#38155 = CARTESIAN_POINT ( 'NONE',  ( 13.53749999999999964, -2.886751345948125991, -5.000000000000000000 ) ) ;
#38156 = CARTESIAN_POINT ( 'NONE',  ( 17.62500000000000000, 6.123233995736764310E-16, -4.999999999999998224 ) ) ;
#38157 = CARTESIAN_POINT ( 'NONE',  ( 13.72500000122903074, 2.886751345948129099, -4.999999999999998224 ) ) ;
#38158 = CARTESIAN_POINT ( 'NONE',  ( 12.36562500061451608, -6.054752690667223547, -1.112240025338166033E-15 ) ) ;
#38159 = VERTEX_POINT ( 'NONE', #56050 ) ;
#38160 = CARTESIAN_POINT ( 'NONE',  ( -1.071796769724485010, 17.05490381179669868, -25.99999999999999289 ) ) ;
#38161 = CARTESIAN_POINT ( 'NONE',  ( 2.121784821874999061, 17.00937500061451857, -33.67503911421598417 ) ) ;
#38162 = CARTESIAN_POINT ( 'NONE',  ( 4.453125000614517326, 4.541064518000418104, -2.621784821874998173 ) ) ;
#38163 = CARTESIAN_POINT ( 'NONE',  ( -7.967954043666661671E-16, 15.67812499938548143, 34.33755215474603517 ) ) ;
#38164 = CARTESIAN_POINT ( 'NONE',  ( 10.20000000000000107, 0.000000000000000000, 4.999999999999998224 ) ) ;
#38165 = DIRECTION ( 'NONE',  ( 0.000000000000000000, 0.000000000000000000, -1.000000000000000000 ) ) ;
#38166 = ORIENTED_EDGE ( 'NONE', *, *, #3334, .F. ) ;
#38167 = CARTESIAN_POINT ( 'NONE',  ( 23.69062500061451004, -3.027376345333610441, -5.243569643749999898 ) ) ;
#38168 = CARTESIAN_POINT ( 'NONE',  ( 29.51249999999999929, 2.886751345948106007, 5.000000000000033751 ) ) ;
#38169 = CARTESIAN_POINT ( 'NONE',  ( -3.756430356250000102, 18.71562499938548285, 30.00000000000000000 ) ) ;
#38170 = CARTESIAN_POINT ( 'NONE',  ( 20.29687500061451644, 6.054752690667223547, 3.707466751127219781E-16 ) ) ;
#38171 = CARTESIAN_POINT ( 'NONE',  ( 20.09062500061451573, -3.027376345333610441, -5.243569643749999898 ) ) ;
#38172 = CARTESIAN_POINT ( 'NONE',  ( -4.243569643749998122, 13.09062500061459389, -27.54997392385601174 ) ) ;
#38173 = CARTESIAN_POINT ( 'NONE',  ( 7.303125000614516082, 0.000000000000000000, 5.243569643749999010 ) ) ;
#38174 = CARTESIAN_POINT ( 'NONE',  ( 4.528125000614516615, 4.541064518000418104, 2.621784821874999949 ) ) ;
#38175 = CARTESIAN_POINT ( 'NONE',  ( 25.35937500061451644, 0.000000000000000000, 4.756430356249998326 ) ) ;
#38176 = CARTESIAN_POINT ( 'NONE',  ( 21.62812500061451360, 4.541064518000418104, 2.621784821874999949 ) ) ;
#38177 = CYLINDRICAL_SURFACE ( 'NONE', #15023, 3.999999999999996447 ) ;
#38178 = CARTESIAN_POINT ( 'NONE',  ( 3.756430356250000102, 18.94062499938548427, 30.00000000000000000 ) ) ;
#38179 = CARTESIAN_POINT ( 'NONE',  ( 14.33437500061451786, 6.421520780324663323E-16, -5.243569643749999010 ) ) ;
#38180 = CARTESIAN_POINT ( 'NONE',  ( 14.48437500061451821, 4.541064518000418104, 2.621784821874999949 ) ) ;
#38181 = CARTESIAN_POINT ( 'NONE',  ( 22.32187500061451502, -6.054752690667223547, -1.112240025338166033E-15 ) ) ;
#38182 = VERTEX_POINT ( 'NONE', #73038 ) ;
#38183 = CARTESIAN_POINT ( 'NONE',  ( -4.243569643749998122, 11.34687500061451892, 32.45002607614398471 ) ) ;
#38184 = CARTESIAN_POINT ( 'NONE',  ( 3.778125000614519280, -4.541064518000419881, 2.621784821874995952 ) ) ;
#38185 = CARTESIAN_POINT ( 'NONE',  ( 26.35312500061451857, -4.541064518000417216, -2.621784821875001281 ) ) ;
#38186 = CARTESIAN_POINT ( 'NONE',  ( 26.16562500061451502, 3.027376345333611329, 5.243569643749999010 ) ) ;
#38187 = CARTESIAN_POINT ( 'NONE',  ( 1.071796769724495002, 15.10759618943233562, 34.00000000000000000 ) ) ;
#38188 = LINE ( 'NONE', #10125, #19331 ) ;
#38189 = CARTESIAN_POINT ( 'NONE',  ( 4.809375000614516615, -4.541064518000417216, -2.621784821875001281 ) ) ;
#38190 = CARTESIAN_POINT ( 'NONE',  ( 15.26250000122903216, 0.000000000000000000, 4.999999999999998224 ) ) ;
#38191 = CARTESIAN_POINT ( 'NONE',  ( 9.112500001229033586, -4.330127018922190985, -2.500000000000001332 ) ) ;
#38192 = CARTESIAN_POINT ( 'NONE',  ( 29.13750000122903216, 4.330127018922191873, 2.499999999999999556 ) ) ;
#38193 = CARTESIAN_POINT ( 'NONE',  ( 2.000000000000000444, 16.11874999877096570, 26.53589838486224650 ) ) ;
#38194 = CARTESIAN_POINT ( 'NONE',  ( 19.10625000122903216, 4.330127018922192761, -2.499999999999997780 ) ) ;
#38195 = CARTESIAN_POINT ( 'NONE',  ( 12.34687500061452070, -3.027376345333614438, 5.243569643749998122 ) ) ;
#38196 = CARTESIAN_POINT ( 'NONE',  ( 11.88749999999999929, 5.773502691896255534, 3.535250795749688401E-16 ) ) ;
#38197 = VERTEX_POINT ( 'NONE', #5442 ) ;
#38198 = CARTESIAN_POINT ( 'NONE',  ( 19.26562500061451644, 3.027376345333613106, -5.243569643749998122 ) ) ;
#38199 = CARTESIAN_POINT ( 'NONE',  ( 16.84687500061451715, -3.027376345333614438, 5.243569643749998122 ) ) ;
#38200 = CARTESIAN_POINT ( 'NONE',  ( 6.103125000614515905, -4.541064518000417216, -2.621784821875001281 ) ) ;
#38201 = CARTESIAN_POINT ( 'NONE',  ( 21.23437500061451644, 4.541064518000418104, 2.621784821874999949 ) ) ;
#38202 = CARTESIAN_POINT ( 'NONE',  ( 5.803125000614517859, 4.541064518000418104, -2.621784821874998173 ) ) ;
#38203 = CARTESIAN_POINT ( 'NONE',  ( 20.81249999999999645, 2.886751345948157077, -4.999999999999949374 ) ) ;
#38204 = CARTESIAN_POINT ( 'NONE',  ( 7.725000001229034297, -5.773502691896255534, -1.060575238724906372E-15 ) ) ;
#38205 = CARTESIAN_POINT ( 'NONE',  ( 23.65312500061451573, -4.541064518000417216, -2.621784821875001281 ) ) ;
#38206 = CARTESIAN_POINT ( 'NONE',  ( -3.999999999999999112, 18.76250000122903216, -30.00000000000000000 ) ) ;
#38207 = CARTESIAN_POINT ( 'NONE',  ( 6.787500001229032520, -4.330127018922194537, 2.499999999999995559 ) ) ;
#38208 = CARTESIAN_POINT ( 'NONE',  ( 19.22812500061451502, 6.421520780324663323E-16, -5.243569643749999010 ) ) ;
#38209 = CARTESIAN_POINT ( 'NONE',  ( 14.57812500061451644, -4.541064518000419881, 2.621784821874995952 ) ) ;
#38210 = CARTESIAN_POINT ( 'NONE',  ( 24.94687500061451502, -2.746126346562646425, 4.756430356249996549 ) ) ;
#38211 = CARTESIAN_POINT ( 'NONE',  ( 15.48749999999999893, 5.773502691896255534, 3.535250795749688894E-16 ) ) ;
#38212 = CARTESIAN_POINT ( 'NONE',  ( 11.13750000122903216, 4.330127018922191873, 2.499999999999999556 ) ) ;
#38213 = CARTESIAN_POINT ( 'NONE',  ( 8.540625000614518569, 6.054752690667223547, 3.707466751127219781E-16 ) ) ;
#38214 = CARTESIAN_POINT ( 'NONE',  ( 11.31562500061451892, 3.027376345333611329, 5.243569643749999010 ) ) ;
#38215 = EDGE_CURVE ( 'NONE', #18194, #18095, #29226, .T. ) ;
#38216 = CARTESIAN_POINT ( 'NONE',  ( 21.03750000122903074, 4.330127018922191873, 2.499999999999999556 ) ) ;
#38217 = CARTESIAN_POINT ( 'NONE',  ( 4.243569643749999898, 14.64687500061451964, -27.54997392385601529 ) ) ;
#38218 = CARTESIAN_POINT ( 'NONE',  ( 20.14687500061451786, -3.027376345333610441, -5.243569643749999898 ) ) ;
#38219 = CARTESIAN_POINT ( 'NONE',  ( 21.26249999999999574, 2.886751345948129099, -4.999999999999997335 ) ) ;
#38220 = CARTESIAN_POINT ( 'NONE',  ( 4.987500001229032698, -4.330127018922194537, 2.499999999999995559 ) ) ;
#38221 = CARTESIAN_POINT ( 'NONE',  ( 5.259375000614518569, -4.541064518000417216, -2.621784821875001281 ) ) ;
#38222 = CARTESIAN_POINT ( 'NONE',  ( 21.79687500061451644, -3.027376345333614438, 5.243569643749998122 ) ) ;
#38223 = CARTESIAN_POINT ( 'NONE',  ( 5.212500000000002132, 2.886751345948126879, 4.999999999999998224 ) ) ;
#38224 = CARTESIAN_POINT ( 'NONE',  ( 18.85312500061451502, 4.541064518000418104, -2.621784821874998173 ) ) ;
#38225 = CARTESIAN_POINT ( 'NONE',  ( 12.01875000122903181, 2.886751345948126879, 4.999999999999999112 ) ) ;
#38226 = CARTESIAN_POINT ( 'NONE',  ( 13.35000000000000142, 0.000000000000000000, 4.999999999999998224 ) ) ;
#38227 = CARTESIAN_POINT ( 'NONE',  ( 4.544497808834801589, -2.085075457992688897, -4.544497808831748920 ) ) ;
#38228 = CARTESIAN_POINT ( 'NONE',  ( 27.60937500061451644, 0.000000000000000000, 5.243569643749999010 ) ) ;
#38229 = CARTESIAN_POINT ( 'NONE',  ( 20.74687500061451217, 0.000000000000000000, 4.756430356249998326 ) ) ;
#38230 = VECTOR ( 'NONE', #33492, 1000.000000000000000 ) ;
#38231 = CARTESIAN_POINT ( 'NONE',  ( 13.86562500061451431, 3.027376345333613106, -5.243569643749998122 ) ) ;
#38232 = CARTESIAN_POINT ( 'NONE',  ( 13.69687500061451679, -3.027376345333614438, 5.243569643749998122 ) ) ;
#38233 = ORIENTED_EDGE ( 'NONE', *, *, #33218, .F. ) ;
#38234 = CARTESIAN_POINT ( 'NONE',  ( 10.70625000122903536, 0.000000000000000000, 4.999999999999998224 ) ) ;
#38235 = CARTESIAN_POINT ( 'NONE',  ( 22.94062500061451715, 6.054752690667223547, 3.707466751127219781E-16 ) ) ;
#38236 = FACE_OUTER_BOUND ( 'NONE', #9222, .T. ) ;
#38237 = CARTESIAN_POINT ( 'NONE',  ( 1.626862140677534273E-15, 11.67500000122903181, -26.00000000000000355 ) ) ;
#38238 = CARTESIAN_POINT ( 'NONE',  ( 12.52500000000000213, -4.330127018922194537, 2.499999999999995559 ) ) ;
#38239 = CARTESIAN_POINT ( 'NONE',  ( 23.10000000122903074, -2.886751345948125991, -5.000000000000000000 ) ) ;
#38240 = CARTESIAN_POINT ( 'NONE',  ( 18.02812500061451573, 4.541064518000418104, 2.621784821874999949 ) ) ;
#38241 = ORIENTED_EDGE ( 'NONE', *, *, #24606, .T. ) ;
#38242 = CARTESIAN_POINT ( 'NONE',  ( 21.26249999999999574, 2.886751345948129099, -4.999999999999998224 ) ) ;
#38243 = CARTESIAN_POINT ( 'NONE',  ( 23.89687500061451786, 6.054752690667223547, 3.707466751127219781E-16 ) ) ;
#38244 = ORIENTED_EDGE ( 'NONE', *, *, #69367, .F. ) ;
#38245 = CARTESIAN_POINT ( 'NONE',  ( 19.98749999999999716, 5.773502691896255534, 3.535250795749688401E-16 ) ) ;
#38246 = CARTESIAN_POINT ( 'NONE',  ( 9.815625000614518925, 3.027376345333613106, -5.243569643749998122 ) ) ;
#38247 = CARTESIAN_POINT ( 'NONE',  ( 12.30000000000000249, 4.330127018922192761, -2.499999999999997780 ) ) ;
#38248 = CARTESIAN_POINT ( 'NONE',  ( 13.13437500061451679, -2.746126346562646425, 4.756430356249996549 ) ) ;
#38249 = CARTESIAN_POINT ( 'NONE',  ( 16.12500000000000000, -4.330127018922194537, 2.499999999999995559 ) ) ;
#38250 = CARTESIAN_POINT ( 'NONE',  ( 24.78750000000000497, -2.886751345948125991, -5.000000000000000000 ) ) ;
#38251 = CARTESIAN_POINT ( 'NONE',  ( 4.243569643749999898, 19.09062500061451573, 32.45002607614398471 ) ) ;
#38252 = CARTESIAN_POINT ( 'NONE',  ( 3.984375000614517326, 6.421520780324663323E-16, -5.243569643749999010 ) ) ;
#38253 = CARTESIAN_POINT ( 'NONE',  ( 16.32187500061451502, 3.027376345333611329, 5.243569643749999010 ) ) ;
#38254 = CARTESIAN_POINT ( 'NONE',  ( 29.78437500061451715, 4.541064518000418104, 2.621784821874999949 ) ) ;
#38255 = ORIENTED_EDGE ( 'NONE', *, *, #13474, .T. ) ;
#38256 = CARTESIAN_POINT ( 'NONE',  ( 25.30312500061451431, 0.000000000000000000, 5.243569643749999010 ) ) ;
#38257 = CARTESIAN_POINT ( 'NONE',  ( 27.15937500061451360, 0.000000000000000000, 5.243569643749999010 ) ) ;
#38259 = EDGE_CURVE ( 'NONE', #59156, #57451, #1357, .T. ) ;
#38258 = CARTESIAN_POINT ( 'NONE',  ( 17.00625000122903074, 0.000000000000000000, 4.999999999999998224 ) ) ;
#38260 = CARTESIAN_POINT ( 'NONE',  ( 14.92500000000000071, 6.123233995736764310E-16, -4.999999999999998224 ) ) ;
#38261 = CARTESIAN_POINT ( 'NONE',  ( 12.47812500061451502, 6.421520780324663323E-16, -5.243569643749999010 ) ) ;
#38262 = CARTESIAN_POINT ( 'NONE',  ( 3.722276561693393937, 3.338418630728691827, 4.014037966420130665 ) ) ;
#38263 = CARTESIAN_POINT ( 'NONE',  ( 3.242103837493086330E-14, 11.33750000000000213, 26.00000000000000711 ) ) ;
#38264 = CARTESIAN_POINT ( 'NONE',  ( 28.00312500061451715, 0.000000000000000000, 5.243569643749999010 ) ) ;
#38265 = CARTESIAN_POINT ( 'NONE',  ( 15.75000000122902932, -2.886751345948129988, 4.999999999999997335 ) ) ;
#38266 = LINE ( 'NONE', #26094, #47788 ) ;
#38267 = CARTESIAN_POINT ( 'NONE',  ( 14.37187500061451928, 2.746126346562645981, -4.756430356249997438 ) ) ;
#38268 = CARTESIAN_POINT ( 'NONE',  ( 4.378125000614518925, 6.421520780324663323E-16, -5.243569643749999010 ) ) ;
#38269 = CARTESIAN_POINT ( 'NONE',  ( 21.60937500061451644, 4.541064518000418104, -2.621784821874998173 ) ) ;
#38270 = CARTESIAN_POINT ( 'NONE',  ( 2.121784821874999061, 16.55937500061451573, 26.32496088578401583 ) ) ;
#38271 = CARTESIAN_POINT ( 'NONE',  ( 22.73437500061451644, -4.541064518000419881, 2.621784821874995952 ) ) ;
#38272 = CARTESIAN_POINT ( 'NONE',  ( 29.63437500061451502, 6.421520780324663323E-16, -5.243569643749999010 ) ) ;
#38273 = CARTESIAN_POINT ( 'NONE',  ( -4.243569643749998122, 18.09687500061451715, 32.45002607614398471 ) ) ;
#38274 = CARTESIAN_POINT ( 'NONE',  ( 11.27812500061451573, 4.541064518000418104, 2.621784821874999949 ) ) ;
#38275 = CARTESIAN_POINT ( 'NONE',  ( 3.150000001229034119, -2.886751345948129988, 4.999999999999997335 ) ) ;
#38276 = CARTESIAN_POINT ( 'NONE',  ( 6.946875000614517681, -3.027376345333614438, 5.243569643749998122 ) ) ;
#38277 = CARTESIAN_POINT ( 'NONE',  ( 12.93750000000000178, -2.886751345948130876, 4.999999999999996447 ) ) ;
#38278 = CARTESIAN_POINT ( 'NONE',  ( 8.840625000614515727, -3.027376345333610441, -5.243569643749999898 ) ) ;
#38279 = CARTESIAN_POINT ( 'NONE',  ( 13.28437500061451715, -4.541064518000419881, 2.621784821874995952 ) ) ;
#38280 = CARTESIAN_POINT ( 'NONE',  ( 28.70625000122903003, 0.000000000000000000, 4.999999999999998224 ) ) ;
#38281 = CARTESIAN_POINT ( 'NONE',  ( 21.82500000122903572, 2.886751345948129099, -4.999999999999998224 ) ) ;
#38282 = CARTESIAN_POINT ( 'NONE',  ( 7.171875000614517326, 3.027376345333613106, -5.243569643749998122 ) ) ;
#38283 = CARTESIAN_POINT ( 'NONE',  ( 10.49062500061451431, -3.027376345333614438, 5.243569643749998122 ) ) ;
#38284 = CARTESIAN_POINT ( 'NONE',  ( 26.98125000122903216, -4.330127018922194537, 2.499999999999995559 ) ) ;
#38285 = CARTESIAN_POINT ( 'NONE',  ( 21.64687500061451786, 6.054752690667223547, 3.707466751127219781E-16 ) ) ;
#38286 = FACE_OUTER_BOUND ( 'NONE', #62334, .T. ) ;
#38287 =( BOUNDED_CURVE ( )  B_SPLINE_CURVE ( 2, ( #41313, #35032, #63471, #6963, #1797, #24307, #46854 ),
 .UNSPECIFIED., .F., .F. ) 
 B_SPLINE_CURVE_WITH_KNOTS ( ( 3, 2, 2, 3 ),
 ( 0.07000000000000000666, 0.07333333333333333370, 0.07666666666666664687, 0.07999999999999998779 ),
 .UNSPECIFIED. ) 
 CURVE ( )  GEOMETRIC_REPRESENTATION_ITEM ( )  RATIONAL_B_SPLINE_CURVE ( ( 1.000000000000000000, 0.8660254037844387076, 1.000000000000000000, 0.8660254037844387076, 1.000000000000000000, 0.8660254037844392627, 0.9999999999999994449 ) ) 
 REPRESENTATION_ITEM ( '' )  );
#38288 = CARTESIAN_POINT ( 'NONE',  ( -0.6906555412606038002, 4.953935347589259131, 33.94230526677440452 ) ) ;
#38289 = CARTESIAN_POINT ( 'NONE',  ( 29.22187500061451715, 3.027376345333612662, -5.243569643749998122 ) ) ;
#38290 = CARTESIAN_POINT ( 'NONE',  ( -3.000416591977282496E-16, 11.19687500061451679, -34.90005215228797653 ) ) ;
#38291 = CARTESIAN_POINT ( 'NONE',  ( 16.08750000122903501, 4.330127018922191873, 2.499999999999999556 ) ) ;
#38292 = CARTESIAN_POINT ( 'NONE',  ( -4.243569643749997233, 14.44062500061451715, -27.54997392385601174 ) ) ;
#38293 = CARTESIAN_POINT ( 'NONE',  ( 18.67500000122903714, 2.886751345948129099, -4.999999999999998224 ) ) ;
#38294 = CARTESIAN_POINT ( 'NONE',  ( 10.97812500061451679, -4.541064518000419881, 2.621784821874995952 ) ) ;
#38295 = VECTOR ( 'NONE', #7873, 1000.000000000000000 ) ;
#38296 = VERTEX_POINT ( 'NONE', #34224 ) ;
#38297 = CARTESIAN_POINT ( 'NONE',  ( 13.23750000000000071, 5.773502691896255534, 3.535250795749688894E-16 ) ) ;
#38298 = CARTESIAN_POINT ( 'NONE',  ( -1.999999999999997113, 13.77500000000000036, 33.46410161513775705 ) ) ;
#38299 = CARTESIAN_POINT ( 'NONE',  ( 23.87812500061451715, 4.541064518000418104, 2.621784821874999949 ) ) ;
#38300 = CARTESIAN_POINT ( 'NONE',  ( 10.09687500061451715, -3.027376345333614438, 5.243569643749998122 ) ) ;
#38301 = CARTESIAN_POINT ( 'NONE',  ( -2.498395430326213790E-14, 17.05624999877096926, 26.00000000000000000 ) ) ;
#38302 = CARTESIAN_POINT ( 'NONE',  ( 10.57500000122903572, 2.886751345948129099, -4.999999999999998224 ) ) ;
#38303 = CARTESIAN_POINT ( 'NONE',  ( 18.41250000122903430, 0.000000000000000000, 4.999999999999998224 ) ) ;
#38304 = CLOSED_SHELL ( 'NONE', ( #2216, #48570, #64448, #6708, #20115, #50433, #8046, #28701, #58821, #58549, #46169, #50768, #15966, #72319, #71451, #52232, #11530, #5648, #63632, #36115, #68116, #44592, #8217, #938, #40897, #9715, #18812, #38595, #7613, #67122, #65303, #48014, #1343, #21552, #1345, #31744, #26322, #29765, #18778, #12039, #31479, #67767, #63978, #42410, #69023, #63739, #5062, #45529, #63989, #63916, #58073, #13339, #30169, #9477, #58970, #24046, #56340, #26141, #28884, #36517, #68685, #34396, #20596, #10857, #53442, #10366, #8427, #70238, #47871, #18911, #56194, #63573, #11058, #6771, #36396, #3882, #34249, #39935, #43142, #21784, #32588, #43797, #59626, #4259, #38917, #70188, #46405, #64940, #49491, #59332, #53414, #31611, #8789, #54092, #11967, #35596, #8710, #58147, #27806, #12217, #43240, #46440, #59400, #26635, #22141, #30413, #30589, #13175, #14823, #15303, #61928, #13081, #52220, #72490, #41168 ) ) ;
#38305 = CARTESIAN_POINT ( 'NONE',  ( 15.59062500061451573, -3.027376345333610441, -5.243569643749999898 ) ) ;
#38306 = CARTESIAN_POINT ( 'NONE',  ( 17.87812500061451715, 6.421520780324663323E-16, -5.243569643749999010 ) ) ;
#38307 = CARTESIAN_POINT ( 'NONE',  ( 26.58750000122903145, -4.330127018922194537, 2.499999999999995559 ) ) ;
#38308 =( BOUNDED_CURVE ( )  B_SPLINE_CURVE ( 2, ( #71155, #20165, #9832, #10563, #43458, #37903, #37169, #48999, #27195, #54899, #32733, #26832, #71530, #20905, #25728, #70790, #60059, #4665, #54172, #15000, #71896, #48266, #43823, #65981, #42719, #15361, #59695, #44192, #26092, #3200, #10198, #66347, #32362, #3569, #37537, #65240, #14629, #61168, #15725, #60421, #9102, #21269, #9470, #4307, #31640, #32000, #55270, #49366, #38264, #48630, #33091, #54535, #3937, #60792, #49730, #20527, #72257, #21634, #66723, #16095, #38644, #5750, #68534, #218, #22723, #51177, #16818, #62971, #45276, #40101, #45997, #67809, #22367, #68176, #72985, #40455, #581, #23086, #17183, #45643, #62614, #17539, #61891, #28284, #39373, #12367, #6471, #944, #23451, #39742, #34171, #28639, #67093, #17895, #29006, #72623, #12011, #67455, #50816, #55630, #33816, #51543, #34534, #11296, #57064, #62259, #5024, #27561, #56360, #11656, #50092, #27925, #56707, #6108, #50458, #22007, #44563, #16452, #39010, #61525, #10923, #33450, #55994, #5387, #44919, #64789, #41185, #7549, #58143, #2027, #18978, #64425, #24538, #47082, #29368, #35262, #53344, #24171, #13437, #41539, #69973, #35987, #30083, #46723, #7916, #70337, #30453, #52982, #58871, #2378, #18620, #24896, #52621, #47441, #42266, #69258, #69616, #19343, #7193, #64057, #58506, #41898, #29721, #35623, #13817, #36357, #34902, #8281, #25261, #30811, #2742, #47808, #57429, #63694, #19714, #6833, #51900, #1298, #23808, #46359, #68893, #13085, #18250, #40823, #63340, #12726, #1662, #57784, #52259, #20445, #4217, #66257, #15635, #36714, #54811, #31914, #53716, #9382, #48175, #55184, #37080, #65895, #43733, #37814, #37454, #54450, #59236, #8644, #71070, #72169, #14180, #49278, #42630, #32277, #54088, #48910, #31173, #42995, #38176, #3849, #59973, #65154, #3486, #26370, #26004, #59604, #3108, #60700, #48543, #71441, #20816, #15275, #4579, #43371, #27109, #60334, #9743, #26745, #65526, #21548, #71811, #49642, #21181, #14912, #10113, #31548, #44103, #32643, #25637, #70699, #20074, #14544, #9018, #61078, #34085, #33005, #44475, #5298, #4940, #28202, #21919, #45189, #39654, #27474, #11923, #40012, #50731, #55906, #22639, #56626, #27844, #16732, #33370, #67006, #67721, #72900, #6020, #45556, #68087, #16006, #28555, #854, #33731, #134, #50006, #39287, #17454, #17094, #22996, #62173, #61801, #11204, #38555, #10476, #50375, #51451, #66629, #51090, #16367, #11570, #22282, #44834, #67369, #62526, #34448, #23361, #55544, #38922, #56277, #5666, #486, #56976, #72531, #6380, #28913, #61441, #10834, #58785, #69172, #12998, #24808, #63608, #41451, #7105, #53255, #35534, #30366, #36271, #58055, #12641, #58417, #63247, #30723, #63969, #13352, #7464, #35893, #52895, #52532, #40363, #7830, #29634, #2654, #69886, #64337, #13729, #29990, #24446, #18889, #57341, #8195, #19251, #62882, #2292, #57700, #18532, #45909, #24083, #1940, #47353, #40732, #41806, #41097, #68440, #17803, #52172, #46994, #12278, #18163, #69530, #34810, #35176, #6746, #29279, #51809, #1212, #23718, #1574, #46268, #68807, #46630, #25921, #55098, #31461, #70985, #48461, #65435, #9296, #54728, #14826, #37368, #59891, #3762, #15549, #20361, #38092, #42912, #31829, #20728, #59518, #32560, #54367, #60615, #48093, #26286, #21098, #48823, #43649, #71354, #14462, #64706, #4131, #43287, #65807, #15189, #54004, #37727, #8931, #25172, #49195, #66173, #53627, #26661, #3400, #60247, #9661, #32195, #42544, #71728, #36995, #10024, #47713, #70252, #19624, #42181, #14090, #36630, #59151, #8560, #31088, #3019, #25550, #19991, #70617, #65070, #21461, #39928, #17005, #49919, #5211, #39562, #45103, #4498, #50646, #67998, #11480, #22198, #27752, #34359, #10753, #50291, #38841, #72815, #55823, #49558, #60992, #61715, #66917, #33643, #67639, #16286, #44752, #44392, #4853, #5580, #33284, #62087, #56540, #5933, #27027, #34003, #11840, #67286, #39201, #38466, #16645, #28467, #56187, #51002, #28117, #11114, #50, #72079, #44016, #61356, #62442, #66538, #400, #32923, #22555, #22908, #45466, #17371, #15918, #10391, #55461, #27387, #72443, #21827, #6296, #24727, #69804, #45824, #13272, #46184, #23999, #46547, #69088, #51364, #57252, #2212, #68723, #7021, #23638, #6666, #57973, #63163, #46911, #35810, #58332, #28825, #24364, #1493, #23274, #52088, #17721, #47270, #29194, #56891, #63881, #69450, #51728, #18083, #766, #68360, #41724, #18807, #18449, #40281, #7743, #62802, #41371, #40644, #57618, #30279, #52811, #13639, #12195, #34722, #12558, #1129, #19170, #64251, #35093, #29552, #41014, #63529, #7380, #12916, #35449, #29911, #52451, #1857, #2935, #36183, #9209, #30639, #25837, #72642, #59066, #37281, #48739, #53539, #22025, #31745, #3676, #48374, #54282, #20642, #42825, #53171, #26200, #2568, #14008, #48008, #47631, #70901, #64621, #66744, #70536, #20273, #55649, #10584, #25088, #71262, #19911, #8840, #5045, #14377, #65349, #44212, #31006, #16114, #42099, #27581, #70164, #42464, #14739, #25464, #38666, #19541, #31376, #64986, #59803, #61189, #36546, #3310, #33111, #36912, #50113, #44582, #67114, #59432, #58701, #8471, #53917, #8111, #50836, #11674, #67828, #236, #599, #46016, #56724, #28657, #10945, #16837, #34920, #5770, #68194, #23104, #51560, #45661, #17911, #67474, #56378, #12028, #11315, #33467, #17557, #23825, #34190, #50477, #57447, #39391, #16471, #23470 ),
 .UNSPECIFIED., .F., .F. ) 
 B_SPLINE_CURVE_WITH_KNOTS ( ( 3, 2, 2, 2, 2, 2, 2, 2, 2, 2, 2, 2, 2, 2, 2, 2, 2, 2, 2, 2, 2, 2, 2, 2, 2, 2, 2, 2, 2, 2, 2, 2, 2, 2, 2, 2, 2, 2, 2, 2, 2, 2, 2, 2, 2, 2, 2, 2, 2, 2, 2, 2, 2, 2, 2, 2, 2, 2, 2, 2, 2, 2, 2, 2, 2, 2, 2, 2, 2, 2, 2, 2, 2, 2, 2, 2, 2, 2, 2, 2, 2, 2, 2, 2, 2, 2, 2, 2, 2, 2, 2, 2, 2, 2, 2, 2, 2, 2, 2, 2, 2, 2, 2, 2, 2, 2, 2, 2, 2, 2, 2, 2, 2, 2, 2, 2, 2, 2, 2, 2, 2, 2, 2, 2, 2, 2, 2, 2, 2, 2, 2, 2, 2, 2, 2, 2, 2, 2, 2, 2, 2, 2, 2, 2, 2, 2, 2, 2, 2, 2, 2, 2, 2, 2, 2, 2, 2, 2, 2, 2, 2, 2, 2, 2, 2, 2, 2, 2, 2, 2, 2, 2, 2, 2, 2, 2, 2, 2, 2, 2, 2, 2, 2, 2, 2, 2, 2, 2, 2, 2, 2, 2, 2, 2, 2, 2, 2, 2, 2, 2, 2, 2, 2, 2, 2, 2, 2, 2, 2, 2, 2, 2, 2, 2, 2, 2, 2, 2, 2, 2, 2, 2, 2, 2, 2, 2, 2, 2, 2, 2, 2, 2, 2, 2, 2, 2, 2, 2, 2, 2, 2, 2, 2, 2, 2, 2, 2, 2, 2, 2, 2, 2, 2, 2, 2, 2, 2, 2, 2, 2, 2, 2, 2, 2, 2, 2, 2, 2, 2, 2, 2, 2, 2, 2, 2, 2, 2, 2, 2, 2, 2, 2, 2, 2, 2, 2, 2, 2, 2, 2, 2, 2, 2, 2, 2, 2, 2, 2, 2, 2, 2, 2, 2, 2, 2, 2, 2, 2, 2, 2, 2, 2, 2, 2, 2, 2, 2, 2, 2, 2, 2, 2, 2, 2, 2, 2, 2, 2, 2, 2, 2, 2, 2, 3 ),
 ( 0.000000000000000000, 0.002777777777777777884, 0.005555555555555555768, 0.008333333333333333218, 0.01111111111111111154, 0.01388888888888888812, 0.01666666666666666644, 0.01944444444444444475, 0.02222222222222222307, 0.02500000000000000139, 0.02777777777777777624, 0.03055555555555555455, 0.03333333333333333287, 0.03611111111111111466, 0.03888888888888888951, 0.04166666666666666435, 0.04444444444444444614, 0.04722222222222222099, 0.05000000000000000278, 0.05277777777777777762, 0.05555555555555555247, 0.05833333333333333426, 0.06111111111111110911, 0.06388888888888888395, 0.06666666666666666574, 0.06944444444444444753, 0.07222222222222222932, 0.07499999999999999722, 0.07777777777777777901, 0.08055555555555556080, 0.08333333333333332871, 0.08611111111111111049, 0.08888888888888889228, 0.09166666666666666019, 0.09444444444444444198, 0.09722222222222222376, 0.1000000000000000056, 0.1027777777777777735, 0.1055555555555555552, 0.1083333333333333370, 0.1111111111111111049, 0.1138888888888888729, 0.1166666666666666685, 0.1194444444444444503, 0.1222222222222222182, 0.1250000000000000000, 0.1277777777777777679, 0.1305555555555555636, 0.1333333333333333315, 0.1361111111111110994, 0.1388888888888888951, 0.1416666666666666630, 0.1444444444444444586, 0.1472222222222222543, 0.1499999999999999944, 0.1527777777777777901, 0.1555555555555555580, 0.1583333333333333259, 0.1611111111111111216, 0.1638888888888888895, 0.1666666666666666574, 0.1694444444444444531, 0.1722222222222222210, 0.1749999999999999889, 0.1777777777777777846, 0.1805555555555555525, 0.1833333333333333204, 0.1861111111111111160, 0.1888888888888888840, 0.1916666666666666796, 0.1944444444444444475, 0.1972222222222222154, 0.2000000000000000111, 0.2027777777777777790, 0.2055555555555555469, 0.2083333333333333426, 0.2111111111111111105, 0.2138888888888888784, 0.2166666666666666741, 0.2194444444444444420, 0.2222222222222222099, 0.2250000000000000056, 0.2277777777777777457, 0.2305555555555555414, 0.2333333333333333370, 0.2361111111111111049, 0.2388888888888889006, 0.2416666666666666685, 0.2444444444444444364, 0.2472222222222222321, 0.2500000000000000000, 0.2527777777777777679, 0.2555555555555555358, 0.2583333333333333592, 0.2611111111111111271, 0.2638888888888888951, 0.2666666666666666630, 0.2694444444444444309, 0.2722222222222221988, 0.2750000000000000222, 0.2777777777777777901, 0.2805555555555555580, 0.2833333333333333259, 0.2861111111111110938, 0.2888888888888889173, 0.2916666666666666852, 0.2944444444444445086, 0.2972222222222222210, 0.2999999999999999889, 0.3027777777777777568, 0.3055555555555555802, 0.3083333333333333481, 0.3111111111111111160, 0.3138888888888888840, 0.3166666666666666519, 0.3194444444444444198, 0.3222222222222222432, 0.3250000000000000111, 0.3277777777777777790, 0.3305555555555554914, 0.3333333333333333148, 0.3361111111111110827, 0.3388888888888889062, 0.3416666666666666741, 0.3444444444444444420, 0.3472222222222222099, 0.3499999999999999778, 0.3527777777777778012, 0.3555555555555555691, 0.3583333333333333370, 0.3611111111111111049, 0.3638888888888888729, 0.3666666666666666408, 0.3694444444444444642, 0.3722222222222222321, 0.3750000000000000000, 0.3777777777777777679, 0.3805555555555555358, 0.3833333333333333592, 0.3861111111111111271, 0.3888888888888888951, 0.3916666666666666630, 0.3944444444444444309, 0.3972222222222221988, 0.4000000000000000222, 0.4027777777777777901, 0.4055555555555555580, 0.4083333333333333259, 0.4111111111111110938, 0.4138888888888889173, 0.4166666666666666852, 0.4194444444444445086, 0.4222222222222222210, 0.4249999999999999889, 0.4277777777777777568, 0.4305555555555555802, 0.4333333333333333481, 0.4361111111111111160, 0.4388888888888888840, 0.4416666666666666519, 0.4444444444444444198, 0.4472222222222222432, 0.4500000000000000111, 0.4527777777777777790, 0.4555555555555554914, 0.4583333333333333148, 0.4611111111111110827, 0.4638888888888889062, 0.4666666666666666741, 0.4694444444444444420, 0.4722222222222222099, 0.4749999999999999778, 0.4777777777777778012, 0.4805555555555555691, 0.4833333333333333370, 0.4861111111111111049, 0.4888888888888888729, 0.4916666666666666408, 0.4944444444444444642, 0.4972222222222222321, 0.5000000000000000000, 0.5027777777777777679, 0.5055555555555555358, 0.5083333333333333037, 0.5111111111111110716, 0.5138888888888888395, 0.5166666666666667185, 0.5194444444444444864, 0.5222222222222222543, 0.5250000000000000222, 0.5277777777777777901, 0.5305555555555555580, 0.5333333333333333259, 0.5361111111111110938, 0.5388888888888888618, 0.5416666666666667407, 0.5444444444444443976, 0.5472222222222222765, 0.5500000000000000444, 0.5527777777777778123, 0.5555555555555555802, 0.5583333333333333481, 0.5611111111111111160, 0.5638888888888888840, 0.5666666666666666519, 0.5694444444444444198, 0.5722222222222221877, 0.5749999999999999556, 0.5777777777777778345, 0.5805555555555556024, 0.5833333333333333703, 0.5861111111111111382, 0.5888888888888890172, 0.5916666666666666741, 0.5944444444444444420, 0.5972222222222222099, 0.5999999999999999778, 0.6027777777777777457, 0.6055555555555555136, 0.6083333333333332815, 0.6111111111111111605, 0.6138888888888889284, 0.6166666666666666963, 0.6194444444444444642, 0.6222222222222222321, 0.6250000000000001110, 0.6277777777777777679, 0.6305555555555555358, 0.6333333333333333037, 0.6361111111111110716, 0.6388888888888888395, 0.6416666666666667185, 0.6444444444444444864, 0.6472222222222222543, 0.6500000000000000222, 0.6527777777777777901, 0.6555555555555555580, 0.6583333333333333259, 0.6611111111111109828, 0.6638888888888888618, 0.6666666666666666297, 0.6694444444444443976, 0.6722222222222221655, 0.6750000000000000444, 0.6777777777777778123, 0.6805555555555555802, 0.6833333333333333481, 0.6861111111111111160, 0.6888888888888888840, 0.6916666666666666519, 0.6944444444444444198, 0.6972222222222221877, 0.6999999999999999556, 0.7027777777777777235, 0.7055555555555556024, 0.7083333333333332593, 0.7111111111111111382, 0.7138888888888889062, 0.7166666666666666741, 0.7194444444444444420, 0.7222222222222222099, 0.7249999999999999778, 0.7277777777777777457, 0.7305555555555555136, 0.7333333333333332815, 0.7361111111111111605, 0.7388888888888889284, 0.7416666666666666963, 0.7444444444444444642, 0.7472222222222222321, 0.7500000000000000000, 0.7527777777777777679, 0.7555555555555555358, 0.7583333333333333037, 0.7611111111111110716, 0.7638888888888888395, 0.7666666666666667185, 0.7694444444444444864, 0.7722222222222222543, 0.7750000000000000222, 0.7777777777777777901, 0.7805555555555555580, 0.7833333333333333259, 0.7861111111111110938, 0.7888888888888888618, 0.7916666666666667407, 0.7944444444444443976, 0.7972222222222222765, 0.8000000000000000444, 0.8027777777777778123, 0.8055555555555555802, 0.8083333333333333481, 0.8111111111111111160, 0.8138888888888888840, 0.8166666666666666519, 0.8194444444444444198, 0.8222222222222221877, 0.8249999999999999556, 0.8277777777777778345, 0.8305555555555556024, 0.8333333333333333703, 0.8361111111111111382, 0.8388888888888890172, 0.8416666666666666741, 0.8444444444444444420, 0.8472222222222222099, 0.8499999999999999778, 0.8527777777777777457, 0.8555555555555555136, 0.8583333333333332815, 0.8611111111111111605, 0.8638888888888889284, 0.8666666666666666963, 0.8694444444444444642, 0.8722222222222222321, 0.8749999999999998890, 0.8777777777777777679, 0.8805555555555555358, 0.8833333333333333037, 0.8861111111111110716, 0.8888888888888888395, 0.8916666666666667185, 0.8944444444444444864, 0.8972222222222222543, 0.9000000000000000222, 0.9027777777777777901, 0.9055555555555555580, 0.9083333333333333259, 0.9111111111111109828, 0.9138888888888888618, 0.9166666666666666297, 0.9194444444444443976, 0.9222222222222221655, 0.9243558487027168091 ),
 .UNSPECIFIED. ) 
 CURVE ( )  GEOMETRIC_REPRESENTATION_ITEM ( )  RATIONAL_B_SPLINE_CURVE ( ( 1.000000000000000000, 0.8660254037844387076, 1.000000000000000000, 0.8660254037844387076, 1.000000000000000000, 0.8660254037844387076, 1.000000000000000000, 0.8660254037844387076, 1.000000000000000000, 0.8660254037844387076, 1.000000000000000000, 0.8660254037844387076, 1.000000000000000000, 0.8660254037844387076, 1.000000000000000000, 0.8660254037844387076, 1.000000000000000000, 0.8660254037844387076, 1.000000000000000000, 0.8660254037844387076, 1.000000000000000000, 0.8660254037844387076, 1.000000000000000000, 0.8660254037844387076, 1.000000000000000000, 0.8660254037844387076, 1.000000000000000000, 0.8660254037844387076, 1.000000000000000000, 0.8660254037844387076, 1.000000000000000000, 0.8660254037844387076, 1.000000000000000000, 0.8660254037844387076, 1.000000000000000000, 0.8660254037844387076, 1.000000000000000000, 0.8660254037844387076, 1.000000000000000000, 0.8660254037844387076, 1.000000000000000000, 0.8660254037844387076, 1.000000000000000000, 0.8660254037844387076, 1.000000000000000000, 0.8660254037844387076, 1.000000000000000000, 0.8660254037844387076, 1.000000000000000000, 0.8660254037844387076, 1.000000000000000000, 0.8660254037844387076, 1.000000000000000000, 0.8660254037844387076, 1.000000000000000000, 0.8660254037844387076, 1.000000000000000000, 0.8660254037844387076, 1.000000000000000000, 0.8660254037844387076, 1.000000000000000000, 0.8660254037844387076, 1.000000000000000000, 0.8660254037844387076, 1.000000000000000000, 0.8660254037844387076, 1.000000000000000000, 0.8660254037844387076, 1.000000000000000000, 0.8660254037844387076, 1.000000000000000000, 0.8660254037844387076, 1.000000000000000000, 0.8660254037844387076, 1.000000000000000000, 0.8660254037844387076, 1.000000000000000000, 0.8660254037844387076, 1.000000000000000000, 0.8660254037844387076, 1.000000000000000000, 0.8660254037844387076, 1.000000000000000000, 0.8660254037844387076, 1.000000000000000000, 0.8660254037844387076, 1.000000000000000000, 0.8660254037844387076, 1.000000000000000000, 0.8660254037844387076, 1.000000000000000000, 0.8660254037844387076, 1.000000000000000000, 0.8660254037844387076, 1.000000000000000000, 0.8660254037844387076, 1.000000000000000000, 0.8660254037844387076, 1.000000000000000000, 0.8660254037844387076, 1.000000000000000000, 0.8660254037844387076, 1.000000000000000000, 0.8660254037844387076, 1.000000000000000000, 0.8660254037844387076, 1.000000000000000000, 0.8660254037844387076, 1.000000000000000000, 0.8660254037844387076, 1.000000000000000000, 0.8660254037844387076, 1.000000000000000000, 0.8660254037844387076, 1.000000000000000000, 0.8660254037844387076, 1.000000000000000000, 0.8660254037844387076, 1.000000000000000000, 0.8660254037844387076, 1.000000000000000000, 0.8660254037844387076, 1.000000000000000000, 0.8660254037844387076, 1.000000000000000000, 0.8660254037844387076, 1.000000000000000000, 0.8660254037844387076, 1.000000000000000000, 0.8660254037844387076, 1.000000000000000000, 0.8660254037844387076, 1.000000000000000000, 0.8660254037844387076, 1.000000000000000000, 0.8660254037844387076, 1.000000000000000000, 0.8660254037844387076, 1.000000000000000000, 0.8660254037844387076, 1.000000000000000000, 0.8660254037844387076, 1.000000000000000000, 0.8660254037844387076, 1.000000000000000000, 0.8660254037844387076, 1.000000000000000000, 0.8660254037844387076, 1.000000000000000000, 0.8660254037844387076, 1.000000000000000000, 0.8660254037844387076, 1.000000000000000000, 0.8660254037844387076, 1.000000000000000000, 0.8660254037844387076, 1.000000000000000000, 0.8660254037844387076, 1.000000000000000000, 0.8660254037844387076, 1.000000000000000000, 0.8660254037844387076, 1.000000000000000000, 0.8660254037844387076, 1.000000000000000000, 0.8660254037844387076, 1.000000000000000000, 0.8660254037844387076, 1.000000000000000000, 0.8660254037844387076, 1.000000000000000000, 0.8660254037844387076, 1.000000000000000000, 0.8660254037844387076, 1.000000000000000000, 0.8660254037844387076, 1.000000000000000000, 0.8660254037844387076, 1.000000000000000000, 0.8660254037844387076, 1.000000000000000000, 0.8660254037844387076, 1.000000000000000000, 0.8660254037844387076, 1.000000000000000000, 0.8660254037844387076, 1.000000000000000000, 0.8660254037844387076, 1.000000000000000000, 0.8660254037844387076, 1.000000000000000000, 0.8660254037844387076, 1.000000000000000000, 0.8660254037844387076, 1.000000000000000000, 0.8660254037844387076, 1.000000000000000000, 0.8660254037844387076, 1.000000000000000000, 0.8660254037844387076, 1.000000000000000000, 0.8660254037844387076, 1.000000000000000000, 0.8660254037844387076, 1.000000000000000000, 0.8660254037844387076, 1.000000000000000000, 0.8660254037844387076, 1.000000000000000000, 0.8660254037844387076, 1.000000000000000000, 0.8660254037844387076, 1.000000000000000000, 0.8660254037844387076, 1.000000000000000000, 0.8660254037844387076, 1.000000000000000000, 0.8660254037844387076, 1.000000000000000000, 0.8660254037844387076, 1.000000000000000000, 0.8660254037844387076, 1.000000000000000000, 0.8660254037844387076, 1.000000000000000000, 0.8660254037844387076, 1.000000000000000000, 0.8660254037844387076, 1.000000000000000000, 0.8660254037844387076, 1.000000000000000000, 0.8660254037844387076, 1.000000000000000000, 0.8660254037844387076, 1.000000000000000000, 0.8660254037844387076, 1.000000000000000000, 0.8660254037844387076, 1.000000000000000000, 0.8660254037844387076, 1.000000000000000000, 0.8660254037844387076, 1.000000000000000000, 0.8660254037844387076, 1.000000000000000000, 0.8660254037844387076, 1.000000000000000000, 0.8660254037844387076, 1.000000000000000000, 0.8660254037844387076, 1.000000000000000000, 0.8660254037844387076, 1.000000000000000000, 0.8660254037844387076, 1.000000000000000000, 0.8660254037844387076, 1.000000000000000000, 0.8660254037844387076, 1.000000000000000000, 0.8660254037844387076, 1.000000000000000000, 0.8660254037844387076, 1.000000000000000000, 0.8660254037844387076, 1.000000000000000000, 0.8660254037844387076, 1.000000000000000000, 0.8660254037844387076, 1.000000000000000000, 0.8660254037844387076, 1.000000000000000000, 0.8660254037844387076, 1.000000000000000000, 0.8660254037844387076, 1.000000000000000000, 0.8660254037844387076, 1.000000000000000000, 0.8660254037844387076, 1.000000000000000000, 0.8660254037844387076, 1.000000000000000000, 0.8660254037844387076, 1.000000000000000000, 0.8660254037844387076, 1.000000000000000000, 0.8660254037844387076, 1.000000000000000000, 0.8660254037844387076, 1.000000000000000000, 0.8660254037844387076, 1.000000000000000000, 0.8660254037844387076, 1.000000000000000000, 0.8660254037844387076, 1.000000000000000000, 0.8660254037844387076, 1.000000000000000000, 0.8660254037844387076, 1.000000000000000000, 0.8660254037844387076, 1.000000000000000000, 0.8660254037844387076, 1.000000000000000000, 0.8660254037844387076, 1.000000000000000000, 0.8660254037844387076, 1.000000000000000000, 0.8660254037844387076, 1.000000000000000000, 0.8660254037844387076, 1.000000000000000000, 0.8660254037844387076, 1.000000000000000000, 0.8660254037844387076, 1.000000000000000000, 0.8660254037844387076, 1.000000000000000000, 0.8660254037844387076, 1.000000000000000000, 0.8660254037844387076, 1.000000000000000000, 0.8660254037844387076, 1.000000000000000000, 0.8660254037844387076, 1.000000000000000000, 0.8660254037844387076, 1.000000000000000000, 0.8660254037844387076, 1.000000000000000000, 0.8660254037844387076, 1.000000000000000000, 0.8660254037844387076, 1.000000000000000000, 0.8660254037844387076, 1.000000000000000000, 0.8660254037844387076, 1.000000000000000000, 0.8660254037844387076, 1.000000000000000000, 0.8660254037844387076, 1.000000000000000000, 0.8660254037844387076, 1.000000000000000000, 0.8660254037844387076, 1.000000000000000000, 0.8660254037844387076, 1.000000000000000000, 0.8660254037844387076, 1.000000000000000000, 0.8660254037844387076, 1.000000000000000000, 0.8660254037844387076, 1.000000000000000000, 0.8660254037844387076, 1.000000000000000000, 0.8660254037844387076, 1.000000000000000000, 0.8660254037844387076, 1.000000000000000000, 0.8660254037844387076, 1.000000000000000000, 0.8660254037844387076, 1.000000000000000000, 0.8660254037844387076, 1.000000000000000000, 0.8660254037844387076, 1.000000000000000000, 0.8660254037844387076, 1.000000000000000000, 0.8660254037844387076, 1.000000000000000000, 0.8660254037844387076, 1.000000000000000000, 0.8660254037844387076, 1.000000000000000000, 0.8660254037844387076, 1.000000000000000000, 0.8660254037844387076, 1.000000000000000000, 0.8660254037844387076, 1.000000000000000000, 0.8660254037844387076, 1.000000000000000000, 0.8660254037844387076, 1.000000000000000000, 0.8660254037844387076, 1.000000000000000000, 0.8660254037844387076, 1.000000000000000000, 0.8660254037844387076, 1.000000000000000000, 0.8660254037844387076, 1.000000000000000000, 0.8660254037844387076, 1.000000000000000000, 0.8660254037844387076, 1.000000000000000000, 0.8660254037844387076, 1.000000000000000000, 0.8660254037844387076, 1.000000000000000000, 0.8660254037844387076, 1.000000000000000000, 0.8660254037844387076, 1.000000000000000000, 0.8660254037844387076, 1.000000000000000000, 0.8660254037844387076, 1.000000000000000000, 0.8660254037844387076, 1.000000000000000000, 0.8660254037844387076, 1.000000000000000000, 0.8660254037844387076, 1.000000000000000000, 0.8660254037844387076, 1.000000000000000000, 0.8660254037844387076, 1.000000000000000000, 0.8660254037844387076, 1.000000000000000000, 0.8660254037844387076, 1.000000000000000000, 0.8660254037844387076, 1.000000000000000000, 0.8660254037844387076, 1.000000000000000000, 0.8660254037844387076, 1.000000000000000000, 0.8660254037844387076, 1.000000000000000000, 0.8660254037844387076, 1.000000000000000000, 0.8660254037844387076, 1.000000000000000000, 0.8660254037844387076, 1.000000000000000000, 0.8660254037844387076, 1.000000000000000000, 0.8660254037844387076, 1.000000000000000000, 0.8660254037844387076, 1.000000000000000000, 0.8660254037844387076, 1.000000000000000000, 0.8660254037844387076, 1.000000000000000000, 0.8660254037844387076, 1.000000000000000000, 0.8660254037844387076, 1.000000000000000000, 0.8660254037844387076, 1.000000000000000000, 0.8660254037844387076, 1.000000000000000000, 0.8660254037844387076, 1.000000000000000000, 0.8660254037844387076, 1.000000000000000000, 0.8660254037844387076, 1.000000000000000000, 0.8660254037844387076, 1.000000000000000000, 0.8660254037844387076, 1.000000000000000000, 0.8660254037844387076, 1.000000000000000000, 0.8660254037844387076, 1.000000000000000000, 0.8660254037844387076, 1.000000000000000000, 0.8660254037844387076, 1.000000000000000000, 0.8660254037844387076, 1.000000000000000000, 0.8660254037844387076, 1.000000000000000000, 0.8660254037844387076, 1.000000000000000000, 0.8660254037844387076, 1.000000000000000000, 0.8660254037844387076, 1.000000000000000000, 0.8660254037844387076, 1.000000000000000000, 0.8660254037844387076, 1.000000000000000000, 0.8660254037844387076, 1.000000000000000000, 0.8660254037844387076, 1.000000000000000000, 0.8660254037844387076, 1.000000000000000000, 0.8660254037844387076, 1.000000000000000000, 0.8660254037844387076, 1.000000000000000000, 0.8660254037844387076, 1.000000000000000000, 0.8660254037844387076, 1.000000000000000000, 0.8660254037844387076, 1.000000000000000000, 0.8660254037844387076, 1.000000000000000000, 0.8660254037844387076, 1.000000000000000000, 0.8660254037844387076, 1.000000000000000000, 0.8660254037844387076, 1.000000000000000000, 0.8660254037844387076, 1.000000000000000000, 0.8660254037844387076, 1.000000000000000000, 0.8660254037844387076, 1.000000000000000000, 0.8660254037844387076, 1.000000000000000000, 0.8660254037844387076, 1.000000000000000000, 0.8660254037844387076, 1.000000000000000000, 0.8660254037844387076, 1.000000000000000000, 0.8660254037844387076, 1.000000000000000000, 0.8660254037844387076, 1.000000000000000000, 0.8660254037844387076, 1.000000000000000000, 0.8660254037844387076, 1.000000000000000000, 0.8660254037844387076, 1.000000000000000000, 0.8660254037844387076, 1.000000000000000000, 0.8660254037844387076, 1.000000000000000000, 0.8660254037844387076, 1.000000000000000000, 0.8660254037844387076, 1.000000000000000000, 0.8660254037844387076, 1.000000000000000000, 0.8660254037844387076, 1.000000000000000000, 0.8660254037844387076, 1.000000000000000000, 0.8660254037844387076, 1.000000000000000000, 0.8660254037844387076, 1.000000000000000000, 0.8660254037844387076, 1.000000000000000000, 0.8660254037844387076, 1.000000000000000000, 0.8660254037844387076, 1.000000000000000000, 0.8660254037844387076, 1.000000000000000000, 0.8660254037844387076, 1.000000000000000000, 0.8660254037844387076, 1.000000000000000000, 0.8660254037844387076, 1.000000000000000000, 0.8660254037844387076, 1.000000000000000000, 0.8660254037844387076, 1.000000000000000000, 0.8660254037844387076, 1.000000000000000000, 0.8660254037844387076, 1.000000000000000000, 0.8660254037844387076, 1.000000000000000000, 0.8660254037844387076, 1.000000000000000000, 0.8660254037844387076, 1.000000000000000000, 0.8660254037844387076, 1.000000000000000000, 0.8660254037844387076, 1.000000000000000000, 0.8660254037844387076, 1.000000000000000000, 0.8660254037844387076, 1.000000000000000000, 0.8660254037844387076, 1.000000000000000000, 0.8660254037844387076, 1.000000000000000000, 0.8660254037844387076, 1.000000000000000000, 0.8660254037844387076, 1.000000000000000000, 0.8660254037844387076, 1.000000000000000000, 0.8660254037844387076, 1.000000000000000000, 0.8660254037844387076, 1.000000000000000000, 0.8660254037844387076, 1.000000000000000000, 0.8660254037844387076, 1.000000000000000000, 0.8660254037844387076, 1.000000000000000000, 0.8660254037844387076, 1.000000000000000000, 0.8660254037844387076, 1.000000000000000000, 0.8660254037844387076, 1.000000000000000000, 0.8660254037844387076, 1.000000000000000000, 0.8660254037844387076, 1.000000000000000000, 0.8660254037844387076, 1.000000000000000000, 0.8660254037844387076, 1.000000000000000000, 0.8660254037844387076, 1.000000000000000000, 0.8660254037844387076, 1.000000000000000000, 0.8660254037844387076, 1.000000000000000000, 0.8660254037844387076, 1.000000000000000000, 0.8660254037844387076, 1.000000000000000000, 0.8660254037844387076, 1.000000000000000000, 0.8660254037844387076, 1.000000000000000000, 0.8660254037844387076, 1.000000000000000000, 0.8660254037844387076, 1.000000000000000000, 0.8660254037844387076, 1.000000000000000000, 0.8660254037844387076, 1.000000000000000000, 0.8660254037844387076, 1.000000000000000000, 0.8660254037844387076, 1.000000000000000000, 0.8660254037844387076, 1.000000000000000000, 0.8660254037844387076, 1.000000000000000000, 0.8660254037844387076, 1.000000000000000000, 0.8660254037844387076, 1.000000000000000000, 0.8660254037844387076, 1.000000000000000000, 0.8660254037844387076, 1.000000000000000000, 0.8660254037844387076, 1.000000000000000000, 0.8660254037844387076, 1.000000000000000000, 0.8970933713683293398, 0.9522730444008626893 ) ) 
 REPRESENTATION_ITEM ( '' )  );
#38309 = AXIS2_PLACEMENT_3D ( 'NONE', #61700, #72800, #44001 ) ;
#38310 = CARTESIAN_POINT ( 'NONE',  ( 29.02500000122903145, 2.886751345948129099, -4.999999999999998224 ) ) ;
#38311 = CARTESIAN_POINT ( 'NONE',  ( 23.55000000000000071, 4.330127018922192761, -2.499999999999997780 ) ) ;
#38312 = CARTESIAN_POINT ( 'NONE',  ( 1.878215178124997609, 13.91562499938548392, 33.25316411605952993 ) ) ;
#38313 = CARTESIAN_POINT ( 'NONE',  ( 24.64687500061451431, -3.027376345333610441, -5.243569643749999898 ) ) ;
#38314 = CARTESIAN_POINT ( 'NONE',  ( 1.626862140677534273E-15, 12.01250000000000107, -26.00000000000000355 ) ) ;
#38315 = CARTESIAN_POINT ( 'NONE',  ( 11.73750000122903181, -4.330127018922194537, 2.499999999999995559 ) ) ;
#38316 = CARTESIAN_POINT ( 'NONE',  ( 4.612500000000002487, 2.886751345948129099, -4.999999999999998224 ) ) ;
#38317 = EDGE_CURVE ( 'NONE', #18378, #1784, #33867, .T. ) ;
#38318 = FACE_OUTER_BOUND ( 'NONE', #72955, .T. ) ;
#38319 = CARTESIAN_POINT ( 'NONE',  ( 4.734375000614518214, -4.541064518000419881, 2.621784821874995952 ) ) ;
#38320 = CARTESIAN_POINT ( 'NONE',  ( 26.42812500061451431, 6.421520780324663323E-16, -5.243569643749999010 ) ) ;
#38321 =( BOUNDED_CURVE ( )  B_SPLINE_CURVE ( 2, ( #60265, #9679, #3039, #25570, #42561, #32212, #54746 ),
 .UNSPECIFIED., .F., .F. ) 
 B_SPLINE_CURVE_WITH_KNOTS ( ( 3, 2, 2, 3 ),
 ( 0.6333333333333333037, 0.6361111111111110716, 0.6388888888888889506, 0.6416666666666668295 ),
 .UNSPECIFIED. ) 
 CURVE ( )  GEOMETRIC_REPRESENTATION_ITEM ( )  RATIONAL_B_SPLINE_CURVE ( ( 1.000000000000000000, 0.8660254037844387076, 1.000000000000000000, 0.8660254037844387076, 1.000000000000000000, 0.8660254037844333785, 1.000000000000005329 ) ) 
 REPRESENTATION_ITEM ( '' )  );
#38322 = CARTESIAN_POINT ( 'NONE',  ( -3.756430356250000990, 13.01562499938548534, 32.16877607737301048 ) ) ;
#38323 = CARTESIAN_POINT ( 'NONE',  ( 11.33437500061451608, 4.541064518000418104, 2.621784821874999949 ) ) ;
#38324 = CARTESIAN_POINT ( 'NONE',  ( 3.678016528196605073, -3.387136381216779402, 3.825344076974688257 ) ) ;
#38325 = CARTESIAN_POINT ( 'NONE',  ( 3.084375000614519191, 6.421520780324663323E-16, -5.243569643749999010 ) ) ;
#38326 = CARTESIAN_POINT ( 'NONE',  ( 8.821875000614518569, -6.054752690667223547, -1.112240025338166033E-15 ) ) ;
#38327 = CARTESIAN_POINT ( 'NONE',  ( 28.02187500061451431, 3.027376345333611329, 5.243569643749999010 ) ) ;
#38328 = CARTESIAN_POINT ( 'NONE',  ( 4.243569643749999898, 12.34062500061459389, 32.45002607614398471 ) ) ;
#38329 = CARTESIAN_POINT ( 'NONE',  ( 22.50000000000000000, -4.330127018922190985, -2.500000000000001332 ) ) ;
#38330 = ORIENTED_EDGE ( 'NONE', *, *, #68955, .F. ) ;
#38331 = CARTESIAN_POINT ( 'NONE',  ( 29.39999999999999858, 4.330127018922192761, -2.499999999999997780 ) ) ;
#38332 = CARTESIAN_POINT ( 'NONE',  ( 3.937500000000000444, -2.886751345948129988, 4.999999999999997335 ) ) ;
#38333 = VERTEX_POINT ( 'NONE', #57117 ) ;
#38334 = CARTESIAN_POINT ( 'NONE',  ( 18.47812500061451857, 4.541064518000418104, 2.621784821874999949 ) ) ;
#38335 = CARTESIAN_POINT ( 'NONE',  ( 10.86562500061451431, 3.027376345333611329, 5.243569643749999010 ) ) ;
#38336 = CARTESIAN_POINT ( 'NONE',  ( 22.50937500061451502, 2.746126346562643317, 4.756430356249998326 ) ) ;
#38337 = CARTESIAN_POINT ( 'NONE',  ( 6.684375000614518392, 6.421520780324663323E-16, -5.243569643749999010 ) ) ;
#38338 = CARTESIAN_POINT ( 'NONE',  ( 18.11250000122903359, -4.330127018922190985, -2.500000000000001332 ) ) ;
#38339 = VECTOR ( 'NONE', #70525, 1000.000000000000000 ) ;
#38340 = CARTESIAN_POINT ( 'NONE',  ( 4.000000000000000000, 19.73749999999999716, 27.69059892324149885 ) ) ;
#38341 = CARTESIAN_POINT ( 'NONE',  ( 7.771875000614516971, 3.027376345333611329, 5.243569643749999010 ) ) ;
#38342 = CARTESIAN_POINT ( 'NONE',  ( 12.53437500061451537, 6.421520780324663323E-16, -5.243569643749999010 ) ) ;
#38343 = CARTESIAN_POINT ( 'NONE',  ( 23.82187500061451502, 3.027376345333613106, -5.243569643749998122 ) ) ;
#38344 = DIRECTION ( 'NONE',  ( 0.000000000000000000, 0.000000000000000000, -1.000000000000000000 ) ) ;
#38345 = ORIENTED_EDGE ( 'NONE', *, *, #36974, .T. ) ;
#38346 = CARTESIAN_POINT ( 'NONE',  ( 12.33750000000000036, 5.773502691896255534, 3.535250795749688894E-16 ) ) ;
#38347 = CARTESIAN_POINT ( 'NONE',  ( 16.99687500061451573, -3.027376345333610441, -5.243569643749999898 ) ) ;
#38348 = VECTOR ( 'NONE', #33593, 1000.000000000000000 ) ;
#38349 = CARTESIAN_POINT ( 'NONE',  ( 9.684375000614517504, -4.541064518000419881, 2.621784821874995952 ) ) ;
#38350 = CARTESIAN_POINT ( 'NONE',  ( 2.655984681222220721E-16, 14.10312499938548392, 25.66244784525396483 ) ) ;
#38351 = CARTESIAN_POINT ( 'NONE',  ( 20.58750000000000213, -2.886751345948129988, 4.999999999999997335 ) ) ;
#38352 = CARTESIAN_POINT ( 'NONE',  ( 3.999999999999998668, 16.96249999999999858, 32.30940107675850470 ) ) ;
#38353 = CARTESIAN_POINT ( 'NONE',  ( -4.243569643749999898, 10.82187500061451857, -32.45002607614398471 ) ) ;
#38354 = CARTESIAN_POINT ( 'NONE',  ( 22.58437500061451431, 4.119189519843966529, 2.378215178124999607 ) ) ;
#38355 = CARTESIAN_POINT ( 'NONE',  ( 12.51562500061451821, 3.027376345333613106, -5.243569643749998122 ) ) ;
#38356 = CARTESIAN_POINT ( 'NONE',  ( 3.337499999999999911, 5.773502691896255534, 3.535250795749688894E-16 ) ) ;
#38357 = CARTESIAN_POINT ( 'NONE',  ( -1.999999999999997113, 19.28750000122903430, -26.53589838486224295 ) ) ;
#38358 = CARTESIAN_POINT ( 'NONE',  ( 28.35937500061451289, 4.541064518000418104, -2.621784821874998173 ) ) ;
#38359 = CARTESIAN_POINT ( 'NONE',  ( 11.06250000000000000, 2.886751345948126879, 4.999999999999999112 ) ) ;
#38360 = CARTESIAN_POINT ( 'NONE',  ( -3.999999999999999556, 15.57500000122903216, 27.69059892324149530 ) ) ;
#38361 = CARTESIAN_POINT ( 'NONE',  ( 11.36250000122903536, -4.330127018922190985, -2.500000000000001332 ) ) ;
#38362 = AXIS2_PLACEMENT_3D ( 'NONE', #69373, #8028, #57172 ) ;
#38363 = CARTESIAN_POINT ( 'NONE',  ( 22.17187500061451644, 3.027376345333611329, 5.243569643749999010 ) ) ;
#38364 = CARTESIAN_POINT ( 'NONE',  ( 15.04687500061451644, -3.027376345333614438, 5.243569643749998122 ) ) ;
#38365 = DIRECTION ( 'NONE',  ( -1.000000000000000000, -0.000000000000000000, -0.000000000000000000 ) ) ;
#38366 = VERTEX_POINT ( 'NONE', #23505 ) ;
#38367 = CARTESIAN_POINT ( 'NONE',  ( 16.34062500061451573, -3.027376345333614438, 5.243569643749998122 ) ) ;
#38368 = VECTOR ( 'NONE', #9101, 1000.000000000000000 ) ;
#38369 = CARTESIAN_POINT ( 'NONE',  ( 29.17500000122903714, 2.886751345948126879, 4.999999999999999112 ) ) ;
#38370 = CARTESIAN_POINT ( 'NONE',  ( 15.75937500061451857, 4.541064518000418104, -2.621784821874998173 ) ) ;
#38371 = CARTESIAN_POINT ( 'NONE',  ( 2.516032931661824179, 9.680092174376738967, -24.54948276669228591 ) ) ;
#38372 = CARTESIAN_POINT ( 'NONE',  ( 15.92812500061451608, -4.541064518000419881, 2.621784821874995952 ) ) ;
#38373 = FACE_BOUND ( 'NONE', #7615, .T. ) ;
#38374 = EDGE_CURVE ( 'NONE', #58126, #40801, #50512, .T. ) ;
#38375 = CARTESIAN_POINT ( 'NONE',  ( 27.57187500061451857, 3.027376345333611329, 5.243569643749999010 ) ) ;
#38376 = CARTESIAN_POINT ( 'NONE',  ( 4.243569643749999898, 13.24062500061451786, 32.45002607614398471 ) ) ;
#38377 = CARTESIAN_POINT ( 'NONE',  ( 16.43437500061451573, -4.541064518000419881, 2.621784821874995952 ) ) ;
#38378 = CARTESIAN_POINT ( 'NONE',  ( 15.18750000122903465, 4.330127018922191873, 2.499999999999999556 ) ) ;
#38379 = CARTESIAN_POINT ( 'NONE',  ( 10.05937500061451750, 0.000000000000000000, 4.756430356249998326 ) ) ;
#38380 = EDGE_CURVE ( 'NONE', #20653, #42194, #44968, .T. ) ;
#38381 = CARTESIAN_POINT ( 'NONE',  ( 2.121784821874999061, 19.25937500061451857, -33.67503911421598417 ) ) ;
#38382 = CARTESIAN_POINT ( 'NONE',  ( 20.78437500061451715, 4.541064518000418104, 2.621784821874999949 ) ) ;
#38383 = CARTESIAN_POINT ( 'NONE',  ( 22.87500000122903288, 2.886751345948126879, 4.999999999999999112 ) ) ;
#38384 = CARTESIAN_POINT ( 'NONE',  ( 16.84687500061451715, -3.027376345333614438, 5.243569643749998122 ) ) ;
#38385 = CARTESIAN_POINT ( 'NONE',  ( 13.56562500061451892, 3.027376345333611329, 5.243569643749999010 ) ) ;
#38386 = CARTESIAN_POINT ( 'NONE',  ( 4.243569643749999898, 12.43437500061451750, 30.00000000000000000 ) ) ;
#38387 = CARTESIAN_POINT ( 'NONE',  ( 17.16562500061451502, 3.027376345333611329, 5.243569643749999010 ) ) ;
#38388 = ORIENTED_EDGE ( 'NONE', *, *, #14786, .T. ) ;
#38389 = EDGE_LOOP ( 'NONE', ( #2440, #21001, #695, #25704 ) ) ;
#38390 = CARTESIAN_POINT ( 'NONE',  ( 19.61249999999999716, 2.886751345948126879, 4.999999999999999112 ) ) ;
#38391 = CARTESIAN_POINT ( 'NONE',  ( 30.00000000000000000, 0.000000000000000000, 4.999999999999998224 ) ) ;
#38392 = CARTESIAN_POINT ( 'NONE',  ( 24.62812500061451715, 6.421520780324663323E-16, -5.243569643749999010 ) ) ;
#38393 = CARTESIAN_POINT ( 'NONE',  ( 6.028125000614517504, -4.541064518000419881, 2.621784821874995952 ) ) ;
#38394 = CARTESIAN_POINT ( 'NONE',  ( 17.73750000122903359, 6.123233995736764310E-16, -4.999999999999998224 ) ) ;
#38395 = CARTESIAN_POINT ( 'NONE',  ( 22.52812500061451573, 4.541064518000418104, 2.621784821874999949 ) ) ;
#38396 = CARTESIAN_POINT ( 'NONE',  ( 23.69999999999999929, 0.000000000000000000, 4.999999999999998224 ) ) ;
#38397 = CARTESIAN_POINT ( 'NONE',  ( 25.79062500061451502, -3.027376345333614438, 5.243569643749998122 ) ) ;
#38398 = CARTESIAN_POINT ( 'NONE',  ( 5.015625000614518214, 3.027376345333611329, 5.243569643749999010 ) ) ;
#38399 = ORIENTED_EDGE ( 'NONE', *, *, #11801, .T. ) ;
#38400 = CARTESIAN_POINT ( 'NONE',  ( 23.72812500061451502, 6.421520780324663323E-16, -5.243569643749999010 ) ) ;
#38401 = CARTESIAN_POINT ( 'NONE',  ( 4.898587196589412829E-16, 27.50000000000000000, 34.00000000000000000 ) ) ;
#38402 = AXIS2_PLACEMENT_3D ( 'NONE', #16902, #28016, #16185 ) ;
#38403 = CARTESIAN_POINT ( 'NONE',  ( 10.80937500061451928, 4.119189519843966529, -2.378215178124998275 ) ) ;
#38404 = CARTESIAN_POINT ( 'NONE',  ( 11.06250000122903288, 4.330127018922192761, -2.499999999999997780 ) ) ;
#38405 = CARTESIAN_POINT ( 'NONE',  ( -3.999999999999999556, 12.87500000122903465, -32.30940107675850470 ) ) ;
#38406 = CARTESIAN_POINT ( 'NONE',  ( -4.243569643749999898, 18.50937500061451857, -30.00000000000000000 ) ) ;
#38407 = AXIS2_PLACEMENT_3D ( 'NONE', #14443, #10735, #43632 ) ;
#38408 = EDGE_CURVE ( 'NONE', #71251, #20715, #51448, .T. ) ;
#38409 = CARTESIAN_POINT ( 'NONE',  ( 10.35000000000000142, -4.330127018922190985, -2.500000000000001332 ) ) ;
#38411 = CARTESIAN_POINT ( 'NONE',  ( 10.80937500061451928, 4.541064518000418104, -2.621784821874998173 ) ) ;
#38410 = VECTOR ( 'NONE', #23249, 1000.000000000000000 ) ;
#38412 = CARTESIAN_POINT ( 'NONE',  ( 6.412500001229036073, -4.330127018922190985, -2.500000000000001332 ) ) ;
#38413 = CARTESIAN_POINT ( 'NONE',  ( 12.12187500061451573, 3.027376345333613106, -5.243569643749998122 ) ) ;
#38414 = CARTESIAN_POINT ( 'NONE',  ( 6.384375000614516793, 4.541064518000418104, 2.621784821874999949 ) ) ;
#38415 = DIRECTION ( 'NONE',  ( 0.000000000000000000, 0.000000000000000000, 1.000000000000000000 ) ) ;
#38416 = DIRECTION ( 'NONE',  ( -0.000000000000000000, -1.000000000000000000, -0.000000000000000000 ) ) ;
#38417 = CARTESIAN_POINT ( 'NONE',  ( 10.47187500061451715, 3.027376345333611329, 5.243569643749999010 ) ) ;
#38418 = CARTESIAN_POINT ( 'NONE',  ( 3.617702362022032325, -3.451409801779584452, 3.617702362022032325 ) ) ;
#38419 = CARTESIAN_POINT ( 'NONE',  ( 18.74062500061451431, -3.027376345333610441, -5.243569643749999898 ) ) ;
#38420 = CARTESIAN_POINT ( 'NONE',  ( 45.00000000000000000, 0.000000000000000000, 0.000000000000000000 ) ) ;
#38421 = CARTESIAN_POINT ( 'NONE',  ( -4.243569643749999898, 19.35312500061459318, 30.00000000000000000 ) ) ;
#38422 = CARTESIAN_POINT ( 'NONE',  ( 23.85937500061451644, 4.541064518000418104, -2.621784821874998173 ) ) ;
#38423 = CARTESIAN_POINT ( 'NONE',  ( -3.999999999999999112, 13.81250000122903465, -30.00000000000000000 ) ) ;
#38424 = CARTESIAN_POINT ( 'NONE',  ( 29.28750000122903074, -4.330127018922194537, 2.499999999999995559 ) ) ;
#38425 = CARTESIAN_POINT ( 'NONE',  ( 19.99687500061451217, -4.119189519843965641, -2.378215178125001383 ) ) ;
#38426 = CARTESIAN_POINT ( 'NONE',  ( 24.44062500061451715, -3.027376345333614438, 5.243569643749998122 ) ) ;
#38427 = CARTESIAN_POINT ( 'NONE',  ( 17.16562500061451502, 3.027376345333611329, 5.243569643749999010 ) ) ;
#38428 = CARTESIAN_POINT ( 'NONE',  ( 13.44375000122903252, -2.886751345948129988, 4.999999999999997335 ) ) ;
#38429 = CARTESIAN_POINT ( 'NONE',  ( 13.80937500061451750, -4.541064518000417216, -2.621784821875001281 ) ) ;
#38430 = CARTESIAN_POINT ( 'NONE',  ( 7.396875000614516082, -4.119189519843965641, -2.378215178125001383 ) ) ;
#38431 = CARTESIAN_POINT ( 'NONE',  ( 26.70000000122903572, -2.886751345948125991, -5.000000000000000000 ) ) ;
#38432 = CARTESIAN_POINT ( 'NONE',  ( 4.621875000614516615, 3.027376345333611329, 5.243569643749999010 ) ) ;
#38433 = CARTESIAN_POINT ( 'NONE',  ( 15.15937500061451715, -4.541064518000417216, -2.621784821875001281 ) ) ;
#38434 = CARTESIAN_POINT ( 'NONE',  ( 21.18749999999999645, -2.886751345948126435, -5.000000000000000000 ) ) ;
#38435 = CARTESIAN_POINT ( 'NONE',  ( -6.275039685470489619E-15, 18.31250000000000000, -26.00000000000000355 ) ) ;
#38436 = CARTESIAN_POINT ( 'NONE',  ( 3.675000001229035362, -5.773502691896255534, -1.060575238724906372E-15 ) ) ;
#38437 = CARTESIAN_POINT ( 'NONE',  ( 24.68437500061451573, 6.421520780324663323E-16, -5.243569643749999010 ) ) ;
#38438 = CARTESIAN_POINT ( 'NONE',  ( 17.67187500061451644, 3.027376345333611329, 5.243569643749999010 ) ) ;
#38439 = CARTESIAN_POINT ( 'NONE',  ( 3.756430356250000546, 15.04062499938548392, 27.83122392262697886 ) ) ;
#38440 = CARTESIAN_POINT ( 'NONE',  ( 27.59999999999999787, 4.330127018922192761, -2.499999999999997780 ) ) ;
#38441 = CARTESIAN_POINT ( 'NONE',  ( 4.125000001229034652, -5.773502691896255534, -1.060575238724906372E-15 ) ) ;
#38442 = CARTESIAN_POINT ( 'NONE',  ( 5.400000000000002132, -4.330127018922190985, -2.500000000000001332 ) ) ;
#38443 = CARTESIAN_POINT ( 'NONE',  ( 29.37187500061451928, 2.746126346562643317, 4.756430356249998326 ) ) ;
#38444 = CARTESIAN_POINT ( 'NONE',  ( 19.97812500061451502, -4.541064518000419881, 2.621784821874995952 ) ) ;
#38445 = CARTESIAN_POINT ( 'NONE',  ( 10.05000000000000071, 4.330127018922192761, -2.499999999999997780 ) ) ;
#38446 = CARTESIAN_POINT ( 'NONE',  ( 3.740625000614516527, -3.027376345333614438, 5.243569643749998122 ) ) ;
#38447 = CARTESIAN_POINT ( 'NONE',  ( 19.57500000000000284, 4.330127018922191873, 2.499999999999999556 ) ) ;
#38448 = CARTESIAN_POINT ( 'NONE',  ( 45.00000000000000000, 0.000000000000000000, 0.000000000000000000 ) ) ;
#38449 = CARTESIAN_POINT ( 'NONE',  ( 23.85000000122903430, -2.886751345948129988, 4.999999999999997335 ) ) ;
#38450 = CARTESIAN_POINT ( 'NONE',  ( 5.989600911063004851, 8.007829439449656306, 30.40685004427880855 ) ) ;
#38451 = CARTESIAN_POINT ( 'NONE',  ( 28.80937500061451573, 4.541064518000418104, -2.621784821874998173 ) ) ;
#38452 = VECTOR ( 'NONE', #31319, 1000.000000000000000 ) ;
#38453 = ORIENTED_EDGE ( 'NONE', *, *, #71543, .T. ) ;
#38454 = CARTESIAN_POINT ( 'NONE',  ( 18.10312500061451502, 0.000000000000000000, 5.243569643749999010 ) ) ;
#38455 = CARTESIAN_POINT ( 'NONE',  ( 25.45312500061451644, -4.541064518000417216, -2.621784821875001281 ) ) ;
#38456 = CARTESIAN_POINT ( 'NONE',  ( 22.54687500061451999, 6.054752690667223547, 3.707466751127219781E-16 ) ) ;
#38457 = CARTESIAN_POINT ( 'NONE',  ( 7.275000000000000355, 6.123233995736764310E-16, -4.999999999999998224 ) ) ;
#38458 = CARTESIAN_POINT ( 'NONE',  ( 8.540625000614518569, 6.054752690667223547, 3.707466751127219781E-16 ) ) ;
#38459 = CARTESIAN_POINT ( 'NONE',  ( 27.06562500061451004, 3.027376345333611329, 5.243569643749999010 ) ) ;
#38460 = CARTESIAN_POINT ( 'NONE',  ( 15.83437500061451608, 4.541064518000418104, 2.621784821874999949 ) ) ;
#38461 = CARTESIAN_POINT ( 'NONE',  ( 19.62187500061451573, -6.054752690667223547, -1.112240025338166033E-15 ) ) ;
#38462 = CARTESIAN_POINT ( 'NONE',  ( 34.99999999999999289, 0.000000000000000000, 0.000000000000000000 ) ) ;
#38463 = CARTESIAN_POINT ( 'NONE',  ( -4.243569643749999898, 10.82187500061451857, 27.54997392385601529 ) ) ;
#38464 = CARTESIAN_POINT ( 'NONE',  ( 22.23750000122903003, 6.123233995736764310E-16, -4.999999999999998224 ) ) ;
#38465 = CARTESIAN_POINT ( 'NONE',  ( 17.44687500061451502, -2.746126346562641984, -4.756430356249999214 ) ) ;
#38466 = CARTESIAN_POINT ( 'NONE',  ( 11.65312500061451573, 4.541064518000418104, -2.621784821874998173 ) ) ;
#38467 = CARTESIAN_POINT ( 'NONE',  ( 7.846875000614518036, -3.027376345333614438, 5.243569643749998122 ) ) ;
#38468 = CARTESIAN_POINT ( 'NONE',  ( 8.334375000614516082, -4.541064518000419881, 2.621784821874995952 ) ) ;
#38469 =( BOUNDED_CURVE ( )  B_SPLINE_CURVE ( 2, ( #34309, #28775, #51315, #45779, #33234, #68314, #16593, #27698, #10701 ),
 .UNSPECIFIED., .F., .F. ) 
 B_SPLINE_CURVE_WITH_KNOTS ( ( 3, 2, 2, 2, 3 ),
 ( 0.05434782608695652717, 0.05797101449275362389, 0.06521739130434782428, 0.07246376811594203160, 0.07608695652173913526 ),
 .UNSPECIFIED. ) 
 CURVE ( )  GEOMETRIC_REPRESENTATION_ITEM ( )  RATIONAL_B_SPLINE_CURVE ( ( 0.9330127018922194093, 0.9330127018922194093, 1.000000000000000000, 0.8660254037844387076, 1.000000000000000000, 0.8660254037844387076, 1.000000000000000000, 0.9330127018922191873, 0.9330127018922192983 ) ) 
 REPRESENTATION_ITEM ( '' )  );
#38470 = ORIENTED_EDGE ( 'NONE', *, *, #48083, .T. ) ;
#38471 = EDGE_CURVE ( 'NONE', #24589, #5140, #3783, .T. ) ;
#38472 = CARTESIAN_POINT ( 'NONE',  ( 26.97187500061451360, 3.027376345333613106, -5.243569643749998122 ) ) ;
#38473 = CARTESIAN_POINT ( 'NONE',  ( 18.44062500061451715, 6.054752690667223547, 3.707466751127219781E-16 ) ) ;
#38474 = CARTESIAN_POINT ( 'NONE',  ( 29.02500000122903145, 2.886751345948129099, -4.999999999999998224 ) ) ;
#38475 = CARTESIAN_POINT ( 'NONE',  ( 3.159375000614518036, 4.541064518000418104, -2.621784821874998173 ) ) ;
#38476 = CARTESIAN_POINT ( 'NONE',  ( 24.75937500061451502, 4.541064518000418104, -2.621784821874998173 ) ) ;
#38477 = CARTESIAN_POINT ( 'NONE',  ( 19.64062500061451644, -3.027376345333610441, -5.243569643749999898 ) ) ;
#38478 = CARTESIAN_POINT ( 'NONE',  ( -2.000000000000000000, 10.92500000000000071, 26.53589838486224650 ) ) ;
#38479 = CARTESIAN_POINT ( 'NONE',  ( 23.69062500061451004, -3.027376345333610441, -5.243569643749999898 ) ) ;
#38480 = CARTESIAN_POINT ( 'NONE',  ( 5.737500001229033586, 4.330127018922191873, 2.499999999999999556 ) ) ;
#38481 = VERTEX_POINT ( 'NONE', #53403 ) ;
#38482 = CARTESIAN_POINT ( 'NONE',  ( 29.66249999999999432, -5.773502691896255534, -1.060575238724906372E-15 ) ) ;
#38483 = CARTESIAN_POINT ( 'NONE',  ( -3.999999999999999556, 15.91249999999999964, -32.30940107675850470 ) ) ;
#38484 = CARTESIAN_POINT ( 'NONE',  ( 3.756430356250000102, 18.15312499938548285, 30.00000000000000000 ) ) ;
#38485 = CARTESIAN_POINT ( 'NONE',  ( 5.109375000614518214, 0.000000000000000000, 5.243569643749999010 ) ) ;
#38486 = CYLINDRICAL_SURFACE ( 'NONE', #71515, 4.999999999999998224 ) ;
#38487 = CARTESIAN_POINT ( 'NONE',  ( 11.95312500061451644, -4.541064518000417216, -2.621784821875001281 ) ) ;
#38488 = CARTESIAN_POINT ( 'NONE',  ( 5.484375000614518214, 4.541064518000418104, 2.621784821874999949 ) ) ;
#38489 = CARTESIAN_POINT ( 'NONE',  ( 25.65000000122903145, -2.886751345948129988, 4.999999999999997335 ) ) ;
#38490 = CARTESIAN_POINT ( 'NONE',  ( 15.90937500061451892, 0.000000000000000000, 5.243569643749999010 ) ) ;
#38491 = CARTESIAN_POINT ( 'NONE',  ( 28.56562500061451715, -6.054752690667223547, -1.112240025338166033E-15 ) ) ;
#38492 = CARTESIAN_POINT ( 'NONE',  ( 30.00000000000000000, 0.000000000000000000, 4.999999999999998224 ) ) ;
#38493 = CARTESIAN_POINT ( 'NONE',  ( 26.18437500061451573, 4.541064518000418104, 2.621784821874999949 ) ) ;
#38494 = CARTESIAN_POINT ( 'NONE',  ( 14.40000000000000036, -4.330127018922190985, -2.500000000000001332 ) ) ;
#38495 = CARTESIAN_POINT ( 'NONE',  ( 13.11562500061451786, 3.027376345333611329, 5.243569643749999010 ) ) ;
#38496 = ORIENTED_EDGE ( 'NONE', *, *, #37306, .F. ) ;
#38497 = CARTESIAN_POINT ( 'NONE',  ( 11.12812500061451715, 6.421520780324663323E-16, -5.243569643749999010 ) ) ;
#38498 = CARTESIAN_POINT ( 'NONE',  ( 7.490625000614516082, -3.027376345333610441, -5.243569643749999898 ) ) ;
#38499 = CARTESIAN_POINT ( 'NONE',  ( 18.98437500061451644, 4.119189519843966529, 2.378215178124999607 ) ) ;
#38500 = CARTESIAN_POINT ( 'NONE',  ( 8.925000000000002487, -4.330127018922194537, 2.499999999999995559 ) ) ;
#38501 = CARTESIAN_POINT ( 'NONE',  ( 4.875000001229034652, 2.886751345948126879, 4.999999999999999112 ) ) ;
#38502 = CARTESIAN_POINT ( 'NONE',  ( 17.47499999999999787, -4.330127018922194537, 2.499999999999995559 ) ) ;
#38503 = EDGE_CURVE ( 'NONE', #37474, #60642, #65518, .T. ) ;
#38504 = CARTESIAN_POINT ( 'NONE',  ( 18.53437500061451715, 4.541064518000418104, 2.621784821874999949 ) ) ;
#38505 = CARTESIAN_POINT ( 'NONE',  ( 13.61250000122903359, -4.330127018922190985, -2.500000000000001332 ) ) ;
#38506 = CARTESIAN_POINT ( 'NONE',  ( 20.21250000000000213, -5.773502691896255534, -1.060575238724906372E-15 ) ) ;
#38507 = VECTOR ( 'NONE', #43967, 1000.000000000000000 ) ;
#38508 = CARTESIAN_POINT ( 'NONE',  ( 4.243569643749999010, 15.56562500061451715, -32.45002607614398471 ) ) ;
#38509 = CARTESIAN_POINT ( 'NONE',  ( 0.000000000000000000, 20.00000000000000000, -30.00000000000000000 ) ) ;
#38510 = CYLINDRICAL_SURFACE ( 'NONE', #7658, 4.999999999999998224 ) ;
#38511 = CARTESIAN_POINT ( 'NONE',  ( 28.37812500061451715, 4.541064518000418104, 2.621784821874999949 ) ) ;
#38512 = CARTESIAN_POINT ( 'NONE',  ( 28.38749999999999929, -2.886751345948126435, -5.000000000000000000 ) ) ;
#38513 = CARTESIAN_POINT ( 'NONE',  ( 17.62500000000000000, 6.123233995736764310E-16, -4.999999999999998224 ) ) ;
#38514 = CARTESIAN_POINT ( 'NONE',  ( 13.69687500061451679, -3.027376345333614438, 5.243569643749998122 ) ) ;
#38515 =( BOUNDED_CURVE ( )  B_SPLINE_CURVE ( 2, ( #70298, #42224, #61400, #10794, #32603, #42954, #72487, #10434, #33329 ),
 .UNSPECIFIED., .F., .F. ) 
 B_SPLINE_CURVE_WITH_KNOTS ( ( 3, 2, 2, 2, 3 ),
 ( 0.01086956521739130578, 0.01449275362318840597, 0.02173913043478260809, 0.02898550724637680848, 0.03260869565217391908 ),
 .UNSPECIFIED. ) 
 CURVE ( )  GEOMETRIC_REPRESENTATION_ITEM ( )  RATIONAL_B_SPLINE_CURVE ( ( 0.9330127018922194093, 0.9330127018922194093, 1.000000000000000000, 0.8660254037844387076, 1.000000000000000000, 0.8660254037844387076, 1.000000000000000000, 0.9330127018922191873, 0.9330127018922192983 ) ) 
 REPRESENTATION_ITEM ( '' )  );
#38516 = CARTESIAN_POINT ( 'NONE',  ( 26.21249999999999858, 2.886751345948129099, -4.999999999999998224 ) ) ;
#38517 = CARTESIAN_POINT ( 'NONE',  ( 10.34062500061451750, 6.054752690667223547, 3.707466751127219781E-16 ) ) ;
#38518 = CARTESIAN_POINT ( 'NONE',  ( 28.28437500061451360, 5.492252693125287522, 3.363034840372157021E-16 ) ) ;
#38519 = CARTESIAN_POINT ( 'NONE',  ( 21.38437500061451502, -4.541064518000419881, 2.621784821874995952 ) ) ;
#38520 = CARTESIAN_POINT ( 'NONE',  ( 12.68437500061451573, -2.746126346562646425, 4.756430356249996549 ) ) ;
#38521 = CARTESIAN_POINT ( 'NONE',  ( 7.790625000614518569, -3.027376345333614438, 5.243569643749998122 ) ) ;
#38522 = CARTESIAN_POINT ( 'NONE',  ( 12.15937500061451892, 4.541064518000418104, -2.621784821874998173 ) ) ;
#38523 = EDGE_LOOP ( 'NONE', ( #52115, #9665, #65862, #16932 ) ) ;
#38524 = CARTESIAN_POINT ( 'NONE',  ( 22.43437500061451573, 6.421520780324663323E-16, -5.243569643749999010 ) ) ;
#38525 = DIRECTION ( 'NONE',  ( 0.000000000000000000, 0.000000000000000000, 1.000000000000000000 ) ) ;
#38526 = CARTESIAN_POINT ( 'NONE',  ( 65.00000000000000000, 0.000000000000000000, 0.000000000000000000 ) ) ;
#38527 = CARTESIAN_POINT ( 'NONE',  ( 5.362500000000003375, -5.773502691896255534, -1.060575238724906372E-15 ) ) ;
#38528 = CARTESIAN_POINT ( 'NONE',  ( 14.10000000122903252, -2.886751345948125991, -5.000000000000000000 ) ) ;
#38529 = CARTESIAN_POINT ( 'NONE',  ( 20.79375000122903216, -2.886751345948126435, -5.000000000000000000 ) ) ;
#38530 = CARTESIAN_POINT ( 'NONE',  ( 10.98750000122903536, 6.123233995736764310E-16, -4.999999999999998224 ) ) ;
#38531 = ORIENTED_EDGE ( 'NONE', *, *, #64823, .T. ) ;
#38532 = CARTESIAN_POINT ( 'NONE',  ( 12.41249999999999964, 2.886751345948126879, 4.999999999999999112 ) ) ;
#38533 = CARTESIAN_POINT ( 'NONE',  ( 17.21249999999999858, 2.886751345948129099, -4.999999999999998224 ) ) ;
#38534 = CARTESIAN_POINT ( 'NONE',  ( 12.82500000122903394, 2.886751345948129099, -4.999999999999998224 ) ) ;
#38535 = CARTESIAN_POINT ( 'NONE',  ( 11.27812500061451573, 4.541064518000418104, 2.621784821874999949 ) ) ;
#38536 = ORIENTED_EDGE ( 'NONE', *, *, #14554, .T. ) ;
#38537 = CARTESIAN_POINT ( 'NONE',  ( 10.12500000000000178, 4.330127018922191873, 2.499999999999999556 ) ) ;
#38538 = CYLINDRICAL_SURFACE ( 'NONE', #20673, 3.999999999999996447 ) ;
#38539 = CARTESIAN_POINT ( 'NONE',  ( -4.243569643749999898, 13.52187500061451786, -32.45002607614398471 ) ) ;
#38540 = CARTESIAN_POINT ( 'NONE',  ( 3.403125000614518836, -4.541064518000417216, -2.621784821875001281 ) ) ;
#38541 = CARTESIAN_POINT ( 'NONE',  ( 3.756430356250000102, 14.44062499938548250, 30.00000000000000000 ) ) ;
#38542 = CARTESIAN_POINT ( 'NONE',  ( 8.737500000000002487, 5.773502691896255534, 3.535250795749688894E-16 ) ) ;
#38543 = CARTESIAN_POINT ( 'NONE',  ( 3.862500001229035362, 4.330127018922192761, -2.499999999999997780 ) ) ;
#38544 = ORIENTED_EDGE ( 'NONE', *, *, #71436, .F. ) ;
#38545 = CARTESIAN_POINT ( 'NONE',  ( 24.74062500061451786, 6.054752690667223547, 3.707466751127219781E-16 ) ) ;
#38546 = CARTESIAN_POINT ( 'NONE',  ( 29.28750000122903074, -4.330127018922194537, 2.499999999999995559 ) ) ;
#38547 = VECTOR ( 'NONE', #49482, 1000.000000000000000 ) ;
#38548 = CARTESIAN_POINT ( 'NONE',  ( 2.655984681222220721E-16, 19.95312499938548356, 25.66244784525396483 ) ) ;
#38549 = CARTESIAN_POINT ( 'NONE',  ( 22.05937500061451573, 4.541064518000418104, -2.621784821874998173 ) ) ;
#38550 = CARTESIAN_POINT ( 'NONE',  ( 17.87812500061451715, 6.421520780324663323E-16, -5.243569643749999010 ) ) ;
#38551 = CARTESIAN_POINT ( 'NONE',  ( -4.243569643749999898, 10.80312500061459424, -30.00000000000000000 ) ) ;
#38552 = CARTESIAN_POINT ( 'NONE',  ( 5.653125000614517504, -4.541064518000417216, -2.621784821875001281 ) ) ;
#38553 = CARTESIAN_POINT ( 'NONE',  ( 3.290625000614516793, -3.027376345333614438, 5.243569643749998122 ) ) ;
#38554 = CARTESIAN_POINT ( 'NONE',  ( 23.14687500061451786, -2.746126346562646425, 4.756430356249996549 ) ) ;
#38555 = CARTESIAN_POINT ( 'NONE',  ( 18.85312500061451502, 4.541064518000418104, -2.621784821874998173 ) ) ;
#38556 = CARTESIAN_POINT ( 'NONE',  ( 7.396875000614519635, -2.746126346562646425, 4.756430356249996549 ) ) ;
#38557 = CARTESIAN_POINT ( 'NONE',  ( 3.756430356249998770, 18.45312499938548001, 32.16877607737302469 ) ) ;
#38558 = CARTESIAN_POINT ( 'NONE',  ( 14.22187500061451537, -6.054752690667223547, -1.112240025338166033E-15 ) ) ;
#38559 = CARTESIAN_POINT ( 'NONE',  ( 14.33437500061451786, 6.421520780324663323E-16, -5.243569643749999010 ) ) ;
#38560 = CARTESIAN_POINT ( 'NONE',  ( 23.29687500061451644, -3.027376345333610441, -5.243569643749999898 ) ) ;
#38561 = VERTEX_POINT ( 'NONE', #30142 ) ;
#38562 = CARTESIAN_POINT ( 'NONE',  ( -3.000416591977282496E-16, 12.99687500061451750, 25.09994784771203058 ) ) ;
#38563 = CARTESIAN_POINT ( 'NONE',  ( 3.590625000614518836, 6.054752690667223547, 3.707466751127219781E-16 ) ) ;
#38564 = CARTESIAN_POINT ( 'NONE',  ( 26.54062500061451146, 6.054752690667223547, 3.707466751127219781E-16 ) ) ;
#38565 = CARTESIAN_POINT ( 'NONE',  ( 25.75312500061451715, 0.000000000000000000, 5.243569643749999010 ) ) ;
#38566 = CARTESIAN_POINT ( 'NONE',  ( 8.437500001229034652, 4.330127018922191873, 2.499999999999999556 ) ) ;
#38567 = CARTESIAN_POINT ( 'NONE',  ( 3.999999999999998668, 18.91249999999999787, 27.69059892324149175 ) ) ;
#38568 = CARTESIAN_POINT ( 'NONE',  ( 5.146875000614517859, -3.027376345333614438, 5.243569643749998122 ) ) ;
#38569 = DIRECTION ( 'NONE',  ( 1.000000000000000000, 0.000000000000000000, 0.000000000000000000 ) ) ;
#38570 = CARTESIAN_POINT ( 'NONE',  ( 12.18750000122903465, -4.330127018922194537, 2.499999999999995559 ) ) ;
#38571 = CARTESIAN_POINT ( 'NONE',  ( 8.400000001229035007, 5.773502691896255534, 3.535250795749688894E-16 ) ) ;
#38572 = CARTESIAN_POINT ( 'NONE',  ( 3.478125000614517237, 6.421520780324663323E-16, -5.243569643749999010 ) ) ;
#38573 = CARTESIAN_POINT ( 'NONE',  ( -4.000000000000000888, 15.40624999877096535, 32.30940107675850470 ) ) ;
#38574 = CARTESIAN_POINT ( 'NONE',  ( 19.55625000122903145, 4.330127018922192761, -2.499999999999997780 ) ) ;
#38575 = CARTESIAN_POINT ( 'NONE',  ( 12.15937500061451892, 4.541064518000418104, -2.621784821874998173 ) ) ;
#38576 = CARTESIAN_POINT ( 'NONE',  ( 26.00625000122903074, 0.000000000000000000, 4.999999999999998224 ) ) ;
#38577 = ORIENTED_EDGE ( 'NONE', *, *, #20103, .T. ) ;
#38578 = CARTESIAN_POINT ( 'NONE',  ( 19.97812500061451502, -4.541064518000419881, 2.621784821874995952 ) ) ;
#38579 = CARTESIAN_POINT ( 'NONE',  ( 13.02187500061451608, 3.027376345333613106, -5.243569643749998122 ) ) ;
#38580 = CARTESIAN_POINT ( 'NONE',  ( 5.503125000614516260, 0.000000000000000000, 5.243569643749999010 ) ) ;
#38581 = CARTESIAN_POINT ( 'NONE',  ( 21.34687500061451715, -3.027376345333614438, 5.243569643749998122 ) ) ;
#38582 = CARTESIAN_POINT ( 'NONE',  ( 6.253125000614517148, 4.541064518000418104, -2.621784821874998173 ) ) ;
#38583 = CARTESIAN_POINT ( 'NONE',  ( -1.243387493232115393E-14, 16.15624999877096712, 26.00000000000000000 ) ) ;
#38584 = CARTESIAN_POINT ( 'NONE',  ( 5.550000001229032698, -2.886751345948125991, -5.000000000000000000 ) ) ;
#38585 = CARTESIAN_POINT ( 'NONE',  ( 22.15312500061451573, 0.000000000000000000, 5.243569643749999010 ) ) ;
#38586 = CARTESIAN_POINT ( 'NONE',  ( 3.999999999999998668, 18.57500000122903216, -32.30940107675850470 ) ) ;
#38587 = CARTESIAN_POINT ( 'NONE',  ( 7.987500001229032698, 4.330127018922191873, 2.499999999999999556 ) ) ;
#38588 = CARTESIAN_POINT ( 'NONE',  ( 16.41562500061451857, -6.054752690667223547, -1.112240025338166033E-15 ) ) ;
#38589 = CARTESIAN_POINT ( 'NONE',  ( 14.95312500061451644, 0.000000000000000000, 5.243569643749999010 ) ) ;
#38590 = CARTESIAN_POINT ( 'NONE',  ( 27.04687500061451644, 5.492252693125287522, 3.363034840372157021E-16 ) ) ;
#38591 = CARTESIAN_POINT ( 'NONE',  ( 16.83749999999999858, 5.773502691896255534, 3.535250795749688894E-16 ) ) ;
#38592 = CARTESIAN_POINT ( 'NONE',  ( 10.57500000122903572, 2.886751345948129099, -4.999999999999998224 ) ) ;
#38593 = CARTESIAN_POINT ( 'NONE',  ( 8.465625000614515727, 3.027376345333613106, -5.243569643749998122 ) ) ;
#38594 = CARTESIAN_POINT ( 'NONE',  ( 10.34062500061451750, 6.054752690667223547, 3.707466751127219781E-16 ) ) ;
#38595 = ADVANCED_FACE ( 'NONE', ( #31233 ), #2795, .T. ) ;
#38596 = CARTESIAN_POINT ( 'NONE',  ( 21.78750000122903074, 6.123233995736764310E-16, -4.999999999999998224 ) ) ;
#38597 = CARTESIAN_POINT ( 'NONE',  ( -2.121784821874999949, 14.38437500061451679, -33.67503911421598417 ) ) ;
#38598 = DIRECTION ( 'NONE',  ( 0.000000000000000000, 0.000000000000000000, -1.000000000000000000 ) ) ;
#38599 = CARTESIAN_POINT ( 'NONE',  ( 5.212500001229032343, 4.330127018922192761, -2.499999999999997780 ) ) ;
#38600 = AXIS2_PLACEMENT_3D ( 'NONE', #26371, #48911, #20817 ) ;
#38601 = CARTESIAN_POINT ( 'NONE',  ( 4.471875000614518925, 3.027376345333613106, -5.243569643749998122 ) ) ;
#38602 = CARTESIAN_POINT ( 'NONE',  ( 21.15937500061451715, 4.541064518000418104, -2.621784821874998173 ) ) ;
#38603 = CARTESIAN_POINT ( 'NONE',  ( 8.849999999999999645, 0.000000000000000000, 4.999999999999998224 ) ) ;
#38604 = CARTESIAN_POINT ( 'NONE',  ( 16.64062500061451289, 6.054752690667223547, 3.707466751127219781E-16 ) ) ;
#38605 = B_SPLINE_CURVE_WITH_KNOTS ( 'NONE', 3,
 ( #27466, #66997, #43725, #72160, #44826, #22274, #60325, #49270, #32635, #66248 ),
 .UNSPECIFIED., .F., .F.,
 ( 4, 3, 3, 4 ),
 ( 4.336808689942017255E-19, 5.718089424411147026E-05, 8.577416319149967013E-05, 0.0001143682889712568761 ),
 .UNSPECIFIED. ) ;
#38606 = CARTESIAN_POINT ( 'NONE',  ( 11.45625000122903181, 4.330127018922192761, -2.499999999999997780 ) ) ;
#38607 = CARTESIAN_POINT ( 'NONE',  ( -1.071796769724488563, 15.59240381056766722, -26.00000000000000000 ) ) ;
#38608 = FACE_OUTER_BOUND ( 'NONE', #64694, .T. ) ;
#38609 = CARTESIAN_POINT ( 'NONE',  ( 29.07187500061451502, -6.054752690667223547, -1.112240025338166033E-15 ) ) ;
#38610 = CARTESIAN_POINT ( 'NONE',  ( 20.48437500061451289, -2.746126346562641984, -4.756430356249999214 ) ) ;
#38611 = CARTESIAN_POINT ( 'NONE',  ( 14.54062500061451679, -3.027376345333614438, 5.243569643749998122 ) ) ;
#38612 = CARTESIAN_POINT ( 'NONE',  ( 12.27187500061451786, 3.027376345333611329, 5.243569643749999010 ) ) ;
#38613 = ORIENTED_EDGE ( 'NONE', *, *, #71856, .T. ) ;
#38614 = CARTESIAN_POINT ( 'NONE',  ( 22.27499999999999858, 4.330127018922191873, 2.499999999999999556 ) ) ;
#38615 = CARTESIAN_POINT ( 'NONE',  ( 23.69062500061451004, -3.027376345333610441, -5.243569643749999898 ) ) ;
#38616 = CARTESIAN_POINT ( 'NONE',  ( 3.242103837493086330E-14, 11.33750000000000213, -34.00000000000000000 ) ) ;
#38617 = LINE ( 'NONE', #48973, #54928 ) ;
#38618 = CARTESIAN_POINT ( 'NONE',  ( 12.78749999999999964, 5.773502691896255534, 3.535250795749688894E-16 ) ) ;
#38619 = CARTESIAN_POINT ( 'NONE',  ( 25.27500000122903145, -5.773502691896255534, -1.060575238724906372E-15 ) ) ;
#38620 = CARTESIAN_POINT ( 'NONE',  ( 19.15312500061451573, -4.541064518000417216, -2.621784821875001281 ) ) ;
#38621 = CARTESIAN_POINT ( 'NONE',  ( 12.83437500061451786, -2.746126346562642428, -4.756430356249999214 ) ) ;
#38622 = VERTEX_POINT ( 'NONE', #36044 ) ;
#38623 = CARTESIAN_POINT ( 'NONE',  ( 20.88749999999999929, 5.773502691896255534, 3.535250795749688894E-16 ) ) ;
#38624 = CARTESIAN_POINT ( 'NONE',  ( 22.43437500061451573, 6.421520780324663323E-16, -5.243569643749999010 ) ) ;
#38625 = CARTESIAN_POINT ( 'NONE',  ( 28.56562500061451715, -6.054752690667223547, -1.112240025338166033E-15 ) ) ;
#38626 = VERTEX_POINT ( 'NONE', #53035 ) ;
#38627 = CARTESIAN_POINT ( 'NONE',  ( 3.999999999999998668, 18.01249999999999929, -32.30940107675850470 ) ) ;
#38628 = CARTESIAN_POINT ( 'NONE',  ( 10.15312500061451750, -4.541064518000417216, -2.621784821875001281 ) ) ;
#38629 = CARTESIAN_POINT ( 'NONE',  ( 3.390184931900214860, 3.675138926287994767, 3.390184931900133147 ) ) ;
#38630 = CARTESIAN_POINT ( 'NONE',  ( 14.74687500061451573, 4.119189519843966529, -2.378215178124998275 ) ) ;
#38631 = CARTESIAN_POINT ( 'NONE',  ( 16.87500000000000000, 4.330127018922191873, 2.499999999999999556 ) ) ;
#38632 = CARTESIAN_POINT ( 'NONE',  ( 25.42500000000000071, 4.330127018922191873, 2.499999999999999556 ) ) ;
#38633 = CARTESIAN_POINT ( 'NONE',  ( 3.505568899737581567, -3.565293584294087825, -3.783441448803638529 ) ) ;
#38634 = CARTESIAN_POINT ( 'NONE',  ( 4.021875000614516082, 3.027376345333613106, -5.243569643749998122 ) ) ;
#38635 = CARTESIAN_POINT ( 'NONE',  ( 27.42187500061451644, 3.027376345333613106, -5.243569643749998122 ) ) ;
#38636 = ORIENTED_EDGE ( 'NONE', *, *, #43935, .T. ) ;
#38637 = CARTESIAN_POINT ( 'NONE',  ( 25.67812500061451431, 4.541064518000418104, 2.621784821874999949 ) ) ;
#38638 = CARTESIAN_POINT ( 'NONE',  ( 27.72187500061451715, -6.054752690667223547, -1.112240025338166033E-15 ) ) ;
#38639 = CARTESIAN_POINT ( 'NONE',  ( -2.121784821874996840, 18.97812500061459318, -26.32496088578401583 ) ) ;
#38640 = CARTESIAN_POINT ( 'NONE',  ( 14.84999999999999964, -4.330127018922190985, -2.500000000000001332 ) ) ;
#38641 = CARTESIAN_POINT ( 'NONE',  ( 10.60312500061451679, -4.541064518000417216, -2.621784821875001281 ) ) ;
#38642 = CARTESIAN_POINT ( 'NONE',  ( 3.999999999999998668, 17.35624999877096641, 32.30940107675850470 ) ) ;
#38643 = CARTESIAN_POINT ( 'NONE',  ( 7.124999999999999112, -4.330127018922194537, 2.499999999999995559 ) ) ;
#38644 = CARTESIAN_POINT ( 'NONE',  ( 27.55312500061451786, 0.000000000000000000, 5.243569643749999010 ) ) ;
#38645 = CARTESIAN_POINT ( 'NONE',  ( 16.98750000122903359, 4.330127018922191873, 2.499999999999999556 ) ) ;
#38646 = CARTESIAN_POINT ( 'NONE',  ( 28.88437500061451502, -2.746126346562646425, 4.756430356249996549 ) ) ;
#38647 = CARTESIAN_POINT ( 'NONE',  ( 14.74687500061451573, -2.746126346562642428, -4.756430356249999214 ) ) ;
#38648 = CARTESIAN_POINT ( 'NONE',  ( 4.265625000614517326, -6.054752690667223547, -1.112240025338166033E-15 ) ) ;
#38649 = CARTESIAN_POINT ( 'NONE',  ( 21.23437500061451644, 4.541064518000418104, 2.621784821874999949 ) ) ;
#38650 = CARTESIAN_POINT ( 'NONE',  ( -3.000416591977282496E-16, 15.24687500061451928, 25.09994784771203058 ) ) ;
#38651 = CARTESIAN_POINT ( 'NONE',  ( 21.23437500061451644, 4.541064518000418104, 2.621784821874999949 ) ) ;
#38652 = CARTESIAN_POINT ( 'NONE',  ( 3.600000000000002309, -4.330127018922190985, -2.500000000000001332 ) ) ;
#38653 = CARTESIAN_POINT ( 'NONE',  ( -4.243569643749999898, 19.85937500061451644, 30.00000000000000000 ) ) ;
#38654 = CARTESIAN_POINT ( 'NONE',  ( 9.028125000614517504, 4.541064518000418104, 2.621784821874999949 ) ) ;
#38655 = CARTESIAN_POINT ( 'NONE',  ( 8.099999999999999645, -4.330127018922190985, -2.500000000000001332 ) ) ;
#38656 = EDGE_CURVE ( 'NONE', #69731, #493, #44344, .T. ) ;
#38657 = CARTESIAN_POINT ( 'NONE',  ( 7.959375000614516971, -4.541064518000417216, -2.621784821875001281 ) ) ;
#38658 = DIRECTION ( 'NONE',  ( 0.000000000000000000, 0.000000000000000000, 1.000000000000000000 ) ) ;
#38659 = ADVANCED_FACE ( 'NONE', ( #24590 ), #12781, .F. ) ;
#38660 = CARTESIAN_POINT ( 'NONE',  ( 7.678125000614516082, 4.541064518000418104, 2.621784821874999949 ) ) ;
#38661 = CARTESIAN_POINT ( 'NONE',  ( 12.53437500061451537, 6.421520780324663323E-16, -5.243569643749999010 ) ) ;
#38662 = CARTESIAN_POINT ( 'NONE',  ( 25.72499999999999787, 6.123233995736764310E-16, -4.999999999999998224 ) ) ;
#38663 = CARTESIAN_POINT ( 'NONE',  ( 20.81250000122903643, -4.330127018922190985, -2.500000000000001332 ) ) ;
#38664 = CARTESIAN_POINT ( 'NONE',  ( 7.059375000614518392, -4.541064518000417216, -2.621784821875001281 ) ) ;
#38665 = CARTESIAN_POINT ( 'NONE',  ( 10.56562500061451715, -6.054752690667223547, -1.112240025338166033E-15 ) ) ;
#38666 = CARTESIAN_POINT ( 'NONE',  ( 6.590625000614520168, -3.027376345333610441, -5.243569643749999898 ) ) ;
#38667 = CARTESIAN_POINT ( 'NONE',  ( 26.04375000122902861, -2.886751345948129988, 4.999999999999997335 ) ) ;
#38668 = CARTESIAN_POINT ( 'NONE',  ( 19.28437500061451360, 6.421520780324663323E-16, -5.243569643749999010 ) ) ;
#38669 = CARTESIAN_POINT ( 'NONE',  ( 4.000000000000000000, 13.10000000122903430, 32.30940107675849760 ) ) ;
#38670 = CARTESIAN_POINT ( 'NONE',  ( 12.06562500061451537, 3.027376345333613106, -5.243569643749998122 ) ) ;
#38671 = AXIS2_PLACEMENT_3D ( 'NONE', #4688, #26115, #54558 ) ;
#38672 = CARTESIAN_POINT ( 'NONE',  ( 28.50937500061451502, 0.000000000000000000, 5.243569643749999010 ) ) ;
#38673 = CARTESIAN_POINT ( 'NONE',  ( -4.243569643749998122, 12.69687500061451857, -27.54997392385601174 ) ) ;
#38674 = EDGE_CURVE ( 'NONE', #52475, #3090, #19035, .T. ) ;
#38675 = CARTESIAN_POINT ( 'NONE',  ( 15.78750000122903430, -4.330127018922194537, 2.499999999999995559 ) ) ;
#38676 = CARTESIAN_POINT ( 'NONE',  ( -3.000416591977282496E-16, 14.29062500061451679, -34.90005215228797653 ) ) ;
#38677 = CARTESIAN_POINT ( 'NONE',  ( 14.28750000122903430, 4.330127018922191873, 2.499999999999999556 ) ) ;
#38678 = CARTESIAN_POINT ( 'NONE',  ( 11.20312500061451644, 4.541064518000418104, -2.621784821874998173 ) ) ;
#38679 = ORIENTED_EDGE ( 'NONE', *, *, #33576, .T. ) ;
#38680 = CARTESIAN_POINT ( 'NONE',  ( 12.75000000000000178, 4.330127018922192761, -2.499999999999997780 ) ) ;
#38681 = CYLINDRICAL_SURFACE ( 'NONE', #58548, 4.999999999999998224 ) ;
#38682 = CARTESIAN_POINT ( 'NONE',  ( 22.26562500061451644, -6.054752690667223547, -1.112240025338166033E-15 ) ) ;
#38683 = CARTESIAN_POINT ( 'NONE',  ( 7.771875000614516082, 3.027376345333611329, 5.243569643749999010 ) ) ;
#38684 = EDGE_CURVE ( 'NONE', #16881, #46843, #58565, .T. ) ;
#38685 = CARTESIAN_POINT ( 'NONE',  ( 10.46250000122903323, -4.330127018922190985, -2.500000000000001332 ) ) ;
#38686 = CARTESIAN_POINT ( 'NONE',  ( 19.05000000122903359, -2.886751345948125991, -5.000000000000000000 ) ) ;
#38687 = CARTESIAN_POINT ( 'NONE',  ( 16.26562500061451289, 3.027376345333611329, 5.243569643749999010 ) ) ;
#38688 =( BOUNDED_CURVE ( )  B_SPLINE_CURVE ( 2, ( #71349, #25545, #20724, #60243, #2649, #65803, #37723 ),
 .UNSPECIFIED., .F., .F. ) 
 B_SPLINE_CURVE_WITH_KNOTS ( ( 3, 2, 2, 3 ),
 ( 0.8333333333333334814, 0.8361111111111112493, 0.8388888888888890172, 0.8416666666666667851 ),
 .UNSPECIFIED. ) 
 CURVE ( )  GEOMETRIC_REPRESENTATION_ITEM ( )  RATIONAL_B_SPLINE_CURVE ( ( 0.9999999999999946709, 0.8660254037844440367, 1.000000000000000000, 0.8660254037844387076, 1.000000000000000000, 0.8660254037844333785, 1.000000000000005329 ) ) 
 REPRESENTATION_ITEM ( '' )  );
#38689 = CARTESIAN_POINT ( 'NONE',  ( 19.07812500061451644, -4.541064518000419881, 2.621784821874995952 ) ) ;
#38690 = CARTESIAN_POINT ( 'NONE',  ( 26.06250000122903288, 0.000000000000000000, 4.999999999999998224 ) ) ;
#38691 = CARTESIAN_POINT ( 'NONE',  ( 27.26250000122903216, 4.330127018922192761, -2.499999999999997780 ) ) ;
#38692 = CARTESIAN_POINT ( 'NONE',  ( 22.05000000000000071, -4.330127018922190985, -2.500000000000001332 ) ) ;
#38693 = CARTESIAN_POINT ( 'NONE',  ( -1.878215178125001827, 14.74062499938548321, 33.25316411605952283 ) ) ;
#38694 = CARTESIAN_POINT ( 'NONE',  ( 26.07187500061451857, 3.027376345333613106, -5.243569643749998122 ) ) ;
#38695 = CARTESIAN_POINT ( 'NONE',  ( -1.626862140677534273E-15, 17.73124999877096641, 34.00000000000000000 ) ) ;
#38696 = CARTESIAN_POINT ( 'NONE',  ( 12.71250000122903145, -4.330127018922190985, -2.500000000000001332 ) ) ;
#38697 = CARTESIAN_POINT ( 'NONE',  ( 28.99687500061451573, -3.027376345333614438, 5.243569643749998122 ) ) ;
#38698 = CYLINDRICAL_SURFACE ( 'NONE', #7796, 4.999999999999998224 ) ;
#38699 = CARTESIAN_POINT ( 'NONE',  ( 4.246875000614519280, -3.027376345333614438, 5.243569643749998122 ) ) ;
#38700 = CARTESIAN_POINT ( 'NONE',  ( 24.62812500061451715, 6.421520780324663323E-16, -5.243569643749999010 ) ) ;
#38701 = CARTESIAN_POINT ( 'NONE',  ( 1.878215178124997609, 15.37812499938548427, 33.25316411605952993 ) ) ;
#38702 = CARTESIAN_POINT ( 'NONE',  ( -3.999999999999999112, 13.98124999877096641, 27.69059892324149530 ) ) ;
#38703 = CARTESIAN_POINT ( 'NONE',  ( 9.759375000614516793, -4.541064518000417216, -2.621784821875001281 ) ) ;
#38704 = LINE ( 'NONE', #27616, #57183 ) ;
#38705 = CARTESIAN_POINT ( 'NONE',  ( 3.196875000614516793, 6.054752690667223547, 3.707466751127219781E-16 ) ) ;
#38706 = CARTESIAN_POINT ( 'NONE',  ( 5.296875000614518214, -3.027376345333610441, -5.243569643749999898 ) ) ;
#38707 = CARTESIAN_POINT ( 'NONE',  ( 27.75937500061451502, -4.541064518000417216, -2.621784821875001281 ) ) ;
#38709 = CIRCLE ( 'NONE', #54047, 9.000000000000000000 ) ;
#38708 = CARTESIAN_POINT ( 'NONE',  ( -4.243569643749998122, 10.84062500061459389, 32.45002607614398471 ) ) ;
#38710 = CARTESIAN_POINT ( 'NONE',  ( 18.93750000000000000, -2.886751345948125991, -5.000000000000000000 ) ) ;
#38711 = ORIENTED_EDGE ( 'NONE', *, *, #9967, .T. ) ;
#38712 = CARTESIAN_POINT ( 'NONE',  ( 28.35000000000000142, -4.330127018922190985, -2.500000000000001332 ) ) ;
#38713 = CARTESIAN_POINT ( 'NONE',  ( 28.77187500061451431, 3.027376345333613106, -5.243569643749998122 ) ) ;
#38714 = ORIENTED_EDGE ( 'NONE', *, *, #68596, .F. ) ;
#38715 = CARTESIAN_POINT ( 'NONE',  ( 16.94062500061451715, -3.027376345333610441, -5.243569643749999898 ) ) ;
#38716 = CARTESIAN_POINT ( 'NONE',  ( 7.678125000614516082, 4.541064518000418104, 2.621784821874999949 ) ) ;
#38717 = CARTESIAN_POINT ( 'NONE',  ( 20.40937500061451360, -5.492252693125287522, -1.008910452111647106E-15 ) ) ;
#38718 = CARTESIAN_POINT ( 'NONE',  ( 5.971875000614516260, 3.027376345333611329, 5.243569643749999010 ) ) ;
#38719 = CARTESIAN_POINT ( 'NONE',  ( 17.47500000122903430, 2.886751345948126879, 4.999999999999999112 ) ) ;
#38720 = CARTESIAN_POINT ( 'NONE',  ( 7.509375000614517681, -4.541064518000417216, -2.621784821875001281 ) ) ;
#38721 = CARTESIAN_POINT ( 'NONE',  ( 11.29687500061451644, 6.054752690667223547, 3.707466751127219781E-16 ) ) ;
#38722 = CARTESIAN_POINT ( 'NONE',  ( 24.79687500061451999, 6.054752690667223547, 3.707466751127219781E-16 ) ) ;
#38723 = CARTESIAN_POINT ( 'NONE',  ( 7.429687500307258219, 0.000000000000000000, 4.878215178124998275 ) ) ;
#38724 = VERTEX_POINT ( 'NONE', #58200 ) ;
#38725 = CARTESIAN_POINT ( 'NONE',  ( 9.674999999999998934, 4.330127018922191873, 2.499999999999999556 ) ) ;
#38726 = CARTESIAN_POINT ( 'NONE',  ( 18.04687500061451999, 6.054752690667223547, 3.707466751127219781E-16 ) ) ;
#38727 =( BOUNDED_CURVE ( )  B_SPLINE_CURVE ( 2, ( #22810, #38736, #28723, #68263, #33180, #16543, #27647 ),
 .UNSPECIFIED., .F., .F. ) 
 B_SPLINE_CURVE_WITH_KNOTS ( ( 3, 2, 2, 3 ),
 ( 0.05000000000000005135, 0.05333333333333338533, 0.05666666666666670543, 0.06000000000000003941 ),
 .UNSPECIFIED. ) 
 CURVE ( )  GEOMETRIC_REPRESENTATION_ITEM ( )  RATIONAL_B_SPLINE_CURVE ( ( 0.9999999999999981126, 0.8660254037844407060, 1.000000000000000000, 0.8660254037844387076, 1.000000000000000000, 0.8660254037844370423, 1.000000000000001776 ) ) 
 REPRESENTATION_ITEM ( '' )  );
#38728 = CARTESIAN_POINT ( 'NONE',  ( 8.334375000614516082, -4.541064518000419881, 2.621784821874995952 ) ) ;
#38729 = CARTESIAN_POINT ( 'NONE',  ( -3.756430356250000102, 15.11562499938548321, 30.00000000000000000 ) ) ;
#38730 = CARTESIAN_POINT ( 'NONE',  ( 21.97500000000000142, -4.330127018922194537, 2.499999999999995559 ) ) ;
#38731 = CARTESIAN_POINT ( 'NONE',  ( 3.999999999999998668, 16.51249999999999929, 32.30940107675850470 ) ) ;
#38732 = CARTESIAN_POINT ( 'NONE',  ( -3.999999999999997335, 9.800000001229033586, -27.69059892324149530 ) ) ;
#38733 = CARTESIAN_POINT ( 'NONE',  ( 22.88437500061451857, 5.824947211148865298E-16, -4.756430356249998326 ) ) ;
#38734 = CARTESIAN_POINT ( 'NONE',  ( 11.72812500061451857, 4.541064518000418104, 2.621784821874999949 ) ) ;
#38735 = CARTESIAN_POINT ( 'NONE',  ( 27.98437500061451289, 4.541064518000418104, 2.621784821874999949 ) ) ;
#38736 = CARTESIAN_POINT ( 'NONE',  ( 28.44375000122902719, -2.886751345948149972, -4.999999999999956479 ) ) ;
#38737 = CARTESIAN_POINT ( 'NONE',  ( 27.94687500061451502, 6.054752690667223547, 3.707466751127219781E-16 ) ) ;
#38738 = CARTESIAN_POINT ( 'NONE',  ( 10.23750000000000071, -2.886751345948129988, 4.999999999999997335 ) ) ;
#38739 = CARTESIAN_POINT ( 'NONE',  ( -3.999999999999999112, 15.61250000122903359, 30.00000000000000000 ) ) ;
#38740 = CARTESIAN_POINT ( 'NONE',  ( 9.787500001229036073, 4.330127018922191873, 2.499999999999999556 ) ) ;
#38741 = CARTESIAN_POINT ( 'NONE',  ( 21.08437500061451786, 6.421520780324663323E-16, -5.243569643749999010 ) ) ;
#38742 = CARTESIAN_POINT ( 'NONE',  ( 13.28437500061451715, -4.541064518000419881, 2.621784821874995952 ) ) ;
#38743 = CARTESIAN_POINT ( 'NONE',  ( -1.071796769724488563, 12.44240381056766864, 34.00000000000000000 ) ) ;
#38744 = ORIENTED_EDGE ( 'NONE', *, *, #25043, .T. ) ;
#38745 = CARTESIAN_POINT ( 'NONE',  ( 15.40312500061451573, 0.000000000000000000, 5.243569643749999010 ) ) ;
#38746 = CARTESIAN_POINT ( 'NONE',  ( 27.56250000122902932, -4.330127018922190985, -2.500000000000001332 ) ) ;
#38747 = CARTESIAN_POINT ( 'NONE',  ( 14.44687500061451679, 6.054752690667223547, 3.707466751127219781E-16 ) ) ;
#38748 = CARTESIAN_POINT ( 'NONE',  ( 2.990625000614519191, -3.027376345333610441, -5.243569643749999898 ) ) ;
#38749 = CARTESIAN_POINT ( 'NONE',  ( 18.10312500061451502, 0.000000000000000000, 5.243569643749999010 ) ) ;
#38750 = CARTESIAN_POINT ( 'NONE',  ( 2.000000000000000444, 20.16874999877096641, 26.53589838486224650 ) ) ;
#38751 = CARTESIAN_POINT ( 'NONE',  ( 25.13437500061451502, 6.421520780324663323E-16, -5.243569643749999010 ) ) ;
#38752 = CARTESIAN_POINT ( 'NONE',  ( -2.121784821874999949, 11.62812500061451715, 26.32496088578401938 ) ) ;
#38753 = CARTESIAN_POINT ( 'NONE',  ( 16.39687500061451786, -3.027376345333614438, 5.243569643749998122 ) ) ;
#38754 = CARTESIAN_POINT ( 'NONE',  ( 14.17500000122903536, 2.886751345948129099, -4.999999999999998224 ) ) ;
#38755 = CARTESIAN_POINT ( 'NONE',  ( 9.421875000614518214, 2.746126346562645981, -4.756430356249997438 ) ) ;
#38756 = CARTESIAN_POINT ( 'NONE',  ( 4.243569643749999898, 18.24687500061451928, -27.54997392385601529 ) ) ;
#38757 = ADVANCED_FACE ( 'NONE', ( #64480 ), #47138, .F. ) ;
#38758 = CARTESIAN_POINT ( 'NONE',  ( 19.92187500061451644, 3.027376345333611329, 5.243569643749999010 ) ) ;
#38759 = CARTESIAN_POINT ( 'NONE',  ( 22.57500000122903572, -5.773502691896255534, -1.060575238724906372E-15 ) ) ;
#38760 =( BOUNDED_CURVE ( )  B_SPLINE_CURVE ( 2, ( #28420, #356, #55775, #61667, #29151, #23230, #44703 ),
 .UNSPECIFIED., .F., .T. ) 
 B_SPLINE_CURVE_WITH_KNOTS ( ( 3, 2, 2, 3 ),
 ( 0.9770077471373426192, 0.9777777777777777457, 0.9805555555555555136, 0.9812411888349016342 ),
 .UNSPECIFIED. ) 
 CURVE ( )  GEOMETRIC_REPRESENTATION_ITEM ( )  RATIONAL_B_SPLINE_CURVE ( ( 0.9463123399370627631, 0.9628607641146736951, 1.000000000000000000, 0.8660254037844387076, 1.000000000000000000, 0.9669313209691547950, 0.9501871924685547643 ) ) 
 REPRESENTATION_ITEM ( '' )  );
#38761 = CARTESIAN_POINT ( 'NONE',  ( 17.48437500061451999, 6.421520780324663323E-16, -5.243569643749999010 ) ) ;
#38762 = CARTESIAN_POINT ( 'NONE',  ( 2.121784821874999061, 12.50937500061451857, 26.32496088578401583 ) ) ;
#38763 = CARTESIAN_POINT ( 'NONE',  ( 17.09062500061451573, 6.054752690667223547, 3.707466751127219781E-16 ) ) ;
#38764 = ORIENTED_EDGE ( 'NONE', *, *, #70404, .T. ) ;
#38765 = ORIENTED_EDGE ( 'NONE', *, *, #41986, .F. ) ;
#38766 = CARTESIAN_POINT ( 'NONE',  ( 21.07499999999999929, -4.330127018922194537, 2.499999999999995559 ) ) ;
#38767 = CARTESIAN_POINT ( 'NONE',  ( 28.23750000122903359, 4.330127018922191873, 2.499999999999999556 ) ) ;
#38768 = CARTESIAN_POINT ( 'NONE',  ( 25.45312500061451644, -4.541064518000417216, -2.621784821875001281 ) ) ;
#38769 = CARTESIAN_POINT ( 'NONE',  ( 4.715625000614516615, -6.054752690667223547, -1.112240025338166033E-15 ) ) ;
#38770 = CARTESIAN_POINT ( 'NONE',  ( 16.57500000122903216, 2.886751345948126879, 4.999999999999999112 ) ) ;
#38771 = CARTESIAN_POINT ( 'NONE',  ( 22.97812500061451857, 4.541064518000418104, 2.621784821874999949 ) ) ;
#38772 = CARTESIAN_POINT ( 'NONE',  ( 19.83750000000000213, -2.886751345948125991, -5.000000000000000000 ) ) ;
#38773 = CARTESIAN_POINT ( 'NONE',  ( 26.61562500061451786, 3.027376345333611329, 5.243569643749999010 ) ) ;
#38774 = CARTESIAN_POINT ( 'NONE',  ( 4.940625000614515372, 6.054752690667223547, 3.707466751127219781E-16 ) ) ;
#38775 = ORIENTED_EDGE ( 'NONE', *, *, #52924, .T. ) ;
#38776 = CARTESIAN_POINT ( 'NONE',  ( 26.85000000122903430, 5.773502691896255534, 3.535250795749688401E-16 ) ) ;
#38777 = CARTESIAN_POINT ( 'NONE',  ( 3.290625000614516793, -3.027376345333614438, 5.243569643749998122 ) ) ;
#38778 =( BOUNDED_CURVE ( )  B_SPLINE_CURVE ( 2, ( #17029, #39587, #34026, #56563, #5959, #49582, #28493 ),
 .UNSPECIFIED., .F., .F. ) 
 B_SPLINE_CURVE_WITH_KNOTS ( ( 3, 2, 2, 3 ),
 ( 0.5500000000000000444, 0.5527777777777778123, 0.5555555555555555802, 0.5583333333333333481 ),
 .UNSPECIFIED. ) 
 CURVE ( )  GEOMETRIC_REPRESENTATION_ITEM ( )  RATIONAL_B_SPLINE_CURVE ( ( 1.000000000000000000, 0.8660254037844387076, 1.000000000000000000, 0.8660254037844387076, 1.000000000000000000, 0.8660254037844387076, 1.000000000000000000 ) ) 
 REPRESENTATION_ITEM ( '' )  );
#38779 = CARTESIAN_POINT ( 'NONE',  ( 10.43437500061451750, 4.119189519843966529, 2.378215178124999607 ) ) ;
#38780 = CYLINDRICAL_SURFACE ( 'NONE', #24096, 3.999999999999996447 ) ;
#38781 = CARTESIAN_POINT ( 'NONE',  ( -3.999999999999997335, 10.70000000122903394, -27.69059892324149175 ) ) ;
#38782 = CARTESIAN_POINT ( 'NONE',  ( -4.243569643749999898, 18.92187500061451644, -32.45002607614398471 ) ) ;
#38783 = EDGE_CURVE ( 'NONE', #40333, #8864, #69371, .T. ) ;
#38784 = CARTESIAN_POINT ( 'NONE',  ( 7.800000000000001599, 4.330127018922192761, -2.499999999999997780 ) ) ;
#38785 = CARTESIAN_POINT ( 'NONE',  ( 8.859375000614518214, -4.541064518000417216, -2.621784821875001281 ) ) ;
#38786 = CARTESIAN_POINT ( 'NONE',  ( 6.075000001229034829, 2.886751345948129099, -4.999999999999998224 ) ) ;
#38787 = CARTESIAN_POINT ( 'NONE',  ( 13.09687500061451892, 6.054752690667223547, 3.707466751127219781E-16 ) ) ;
#38788 = CARTESIAN_POINT ( 'NONE',  ( 4.021875000614516082, 3.027376345333613106, -5.243569643749998122 ) ) ;
#38789 = DIRECTION ( 'NONE',  ( 0.000000000000000000, 0.000000000000000000, -1.000000000000000000 ) ) ;
#38790 = CARTESIAN_POINT ( 'NONE',  ( 19.65000000000000213, 0.000000000000000000, 4.999999999999998224 ) ) ;
#38791 = CARTESIAN_POINT ( 'NONE',  ( 10.17187500061451999, -6.054752690667223547, -1.112240025338166033E-15 ) ) ;
#38792 = CARTESIAN_POINT ( 'NONE',  ( 13.27500000000000213, 4.330127018922191873, 2.499999999999999556 ) ) ;
#38793 = EDGE_CURVE ( 'NONE', #47914, #11866, #66561, .T. ) ;
#38794 = CARTESIAN_POINT ( 'NONE',  ( 19.41562500061451146, 3.027376345333611329, 5.243569643749999010 ) ) ;
#38795 = CARTESIAN_POINT ( 'NONE',  ( 45.00000000000000000, 6.123233995736764310E-16, -4.999999999999998224 ) ) ;
#38796 = CARTESIAN_POINT ( 'NONE',  ( 19.93125000122903145, 6.123233995736764310E-16, -4.999999999999998224 ) ) ;
#38797 = CARTESIAN_POINT ( 'NONE',  ( 24.72187500061451360, 3.027376345333613106, -5.243569643749998122 ) ) ;
#38798 = CARTESIAN_POINT ( 'NONE',  ( 1.071796769724490783, 19.41740381056767006, 26.00000000000000355 ) ) ;
#38799 = CARTESIAN_POINT ( 'NONE',  ( 28.08750000122903145, 6.123233995736764310E-16, -4.999999999999998224 ) ) ;
#38800 = CARTESIAN_POINT ( 'NONE',  ( 20.10937500061451644, 2.746126346562645981, -4.756430356249997438 ) ) ;
#38801 = CARTESIAN_POINT ( 'NONE',  ( 26.01562500061451289, 3.027376345333613106, -5.243569643749998122 ) ) ;
#38802 = CARTESIAN_POINT ( 'NONE',  ( 16.56562500061451715, 3.027376345333613106, -5.243569643749998122 ) ) ;
#38803 = CARTESIAN_POINT ( 'NONE',  ( 14.23125000122903394, 4.330127018922191873, 2.499999999999999556 ) ) ;
#38804 = CARTESIAN_POINT ( 'NONE',  ( 13.47187500061451537, 3.027376345333613106, -5.243569643749998122 ) ) ;
#38805 = CARTESIAN_POINT ( 'NONE',  ( 7.509375000614516793, 2.746126346562645981, -4.756430356249997438 ) ) ;
#38806 = CARTESIAN_POINT ( 'NONE',  ( 25.05000000122903714, 5.773502691896255534, 3.535250795749688894E-16 ) ) ;
#38807 = CARTESIAN_POINT ( 'NONE',  ( 4.171875000614517326, 3.027376345333611329, 5.243569643749999010 ) ) ;
#38808 = CARTESIAN_POINT ( 'NONE',  ( 13.35937500061451821, -4.541064518000417216, -2.621784821875001281 ) ) ;
#38809 = CARTESIAN_POINT ( 'NONE',  ( 0.000000000000000000, 27.50000000000000000, 30.00000000000000000 ) ) ;
#38810 = DIRECTION ( 'NONE',  ( 0.000000000000000000, 1.000000000000000000, 0.000000000000000000 ) ) ;
#38811 = CARTESIAN_POINT ( 'NONE',  ( 18.33749999999999858, -2.886751345948130876, 4.999999999999996447 ) ) ;
#38812 = CARTESIAN_POINT ( 'NONE',  ( 25.47187500061451715, -6.054752690667223547, -1.112240025338166033E-15 ) ) ;
#38813 = CARTESIAN_POINT ( 'NONE',  ( 15.75937500061451857, 4.541064518000418104, -2.621784821874998173 ) ) ;
#38814 = CARTESIAN_POINT ( 'NONE',  ( 3.756430356249998770, 16.76562499938548356, 32.16877607737302469 ) ) ;
#38815 = CARTESIAN_POINT ( 'NONE',  ( 27.07499999999999929, 6.123233995736764310E-16, -4.999999999999998224 ) ) ;
#38816 = CARTESIAN_POINT ( 'NONE',  ( 1.071796769724489895, 10.41740381056766473, 26.00000000000000355 ) ) ;
#38817 = CARTESIAN_POINT ( 'NONE',  ( 5.924999999999999822, 6.123233995736764310E-16, -4.999999999999998224 ) ) ;
#38818 = CARTESIAN_POINT ( 'NONE',  ( 29.74687500061451217, 5.492252693125287522, 3.363034840372157021E-16 ) ) ;
#38819 = CARTESIAN_POINT ( 'NONE',  ( 18.92812500061451431, 4.541064518000418104, 2.621784821874999949 ) ) ;
#38820 = CARTESIAN_POINT ( 'NONE',  ( 8.925000000000002487, -4.330127018922194537, 2.499999999999995559 ) ) ;
#38821 = CARTESIAN_POINT ( 'NONE',  ( 3.178125000614515638, 4.541064518000418104, 2.621784821874999949 ) ) ;
#38822 = CARTESIAN_POINT ( 'NONE',  ( 17.55000000000000071, -4.330127018922190985, -2.500000000000001332 ) ) ;
#38823 = CARTESIAN_POINT ( 'NONE',  ( -2.000000000000000000, 17.22500000000000142, 26.53589838486224650 ) ) ;
#38825 = CARTESIAN_POINT ( 'NONE',  ( 21.26250000122903572, -4.330127018922190985, -2.500000000000001332 ) ) ;
#38824 = B_SPLINE_CURVE_WITH_KNOTS ( 'NONE', 3,
 ( #38010, #33556, #67202, #50206, #39477, #28036, #27304, #27667, #32840, #21743 ),
 .UNSPECIFIED., .F., .F.,
 ( 4, 3, 3, 4 ),
 ( 1.727079271278346568E-16, 2.812506120703778600E-05, 5.881405194855023478E-05, 8.950367042444256477E-05 ),
 .UNSPECIFIED. ) ;
#38826 = CARTESIAN_POINT ( 'NONE',  ( 15.15000000000000036, 0.000000000000000000, 4.999999999999998224 ) ) ;
#38827 = CARTESIAN_POINT ( 'NONE',  ( 27.79687500061451999, -3.027376345333610441, -5.243569643749999898 ) ) ;
#38828 = ORIENTED_EDGE ( 'NONE', *, *, #54584, .T. ) ;
#38829 = CARTESIAN_POINT ( 'NONE',  ( 16.71562500061451573, 3.027376345333611329, 5.243569643749999010 ) ) ;
#38830 = CARTESIAN_POINT ( 'NONE',  ( 23.84062500061451928, 6.054752690667223547, 3.707466751127219781E-16 ) ) ;
#38831 = CARTESIAN_POINT ( 'NONE',  ( 23.44687500061451502, 6.054752690667223547, 3.707466751127219781E-16 ) ) ;
#38832 = CARTESIAN_POINT ( 'NONE',  ( 5.850000000000001421, -4.330127018922190985, -2.500000000000001332 ) ) ;
#38833 = CARTESIAN_POINT ( 'NONE',  ( 9.365625000614519635, 3.027376345333613106, -5.243569643749998122 ) ) ;
#38834 = CARTESIAN_POINT ( 'NONE',  ( 25.00312500061451715, -4.541064518000417216, -2.621784821875001281 ) ) ;
#38835 = CARTESIAN_POINT ( 'NONE',  ( 14.22187500061451537, -6.054752690667223547, -1.112240025338166033E-15 ) ) ;
#38836 = CARTESIAN_POINT ( 'NONE',  ( 18.49687500061452283, 6.054752690667223547, 3.707466751127219781E-16 ) ) ;
#38837 = CARTESIAN_POINT ( 'NONE',  ( 30.00000000000000000, 0.000000000000000000, 4.999999999999998224 ) ) ;
#38838 = CARTESIAN_POINT ( 'NONE',  ( -3.000416591977282496E-16, 19.24062500061451431, 25.09994784771203058 ) ) ;
#38839 = CARTESIAN_POINT ( 'NONE',  ( 22.08750000122903501, -4.330127018922194537, 2.499999999999995559 ) ) ;
#38840 = CARTESIAN_POINT ( 'NONE',  ( 18.00937500061451502, 4.119189519843966529, -2.378215178124998275 ) ) ;
#38841 = CARTESIAN_POINT ( 'NONE',  ( 12.51562500061451821, 3.027376345333612662, -5.243569643749998122 ) ) ;
#38842 = CARTESIAN_POINT ( 'NONE',  ( 9.159375000614515372, 0.000000000000000000, 5.243569643749999010 ) ) ;
#38843 = CARTESIAN_POINT ( 'NONE',  ( 6.571875000614517681, -6.054752690667223547, -1.112240025338166033E-15 ) ) ;
#38844 = ORIENTED_EDGE ( 'NONE', *, *, #24606, .F. ) ;
#38845 = CARTESIAN_POINT ( 'NONE',  ( 28.80937500061451573, 4.541064518000418104, -2.621784821874998173 ) ) ;
#38846 = CARTESIAN_POINT ( 'NONE',  ( 20.05312500061451431, -4.541064518000417216, -2.621784821875001281 ) ) ;
#38847 = CARTESIAN_POINT ( 'NONE',  ( 3.253125000614518036, 0.000000000000000000, 5.243569643749999010 ) ) ;
#38848 = CARTESIAN_POINT ( 'NONE',  ( 28.04062500061451502, -3.027376345333614438, 5.243569643749998122 ) ) ;
#38849 = CARTESIAN_POINT ( 'NONE',  ( 24.15937500061451715, -4.541064518000417216, -2.621784821875001281 ) ) ;
#38850 = CARTESIAN_POINT ( 'NONE',  ( 19.26562500061451644, 3.027376345333613106, -5.243569643749998122 ) ) ;
#38851 = CARTESIAN_POINT ( 'NONE',  ( -3.000416591977282496E-16, 19.29687500061451644, 25.09994784771203058 ) ) ;
#38852 = CARTESIAN_POINT ( 'NONE',  ( 25.71562500061451573, 3.027376345333611329, 5.243569643749999010 ) ) ;
#38853 = CARTESIAN_POINT ( 'NONE',  ( 3.525000001229034119, 2.886751345948126879, 4.999999999999999112 ) ) ;
#38854 = VERTEX_POINT ( 'NONE', #32332 ) ;
#38855 = CARTESIAN_POINT ( 'NONE',  ( 27.48749999999999716, -2.886751345948125991, -5.000000000000000000 ) ) ;
#38856 = CARTESIAN_POINT ( 'NONE',  ( 3.999999999999998668, 16.21250000000000213, -32.30940107675850470 ) ) ;
#38857 = CARTESIAN_POINT ( 'NONE',  ( 1.878215178124997609, 17.62812499938548427, 33.25316411605952993 ) ) ;
#38858 = CARTESIAN_POINT ( 'NONE',  ( 3.909375000614518481, -4.541064518000417216, -2.621784821875001281 ) ) ;
#38859 = CARTESIAN_POINT ( 'NONE',  ( 13.71562500061451750, -6.054752690667223547, -1.112240025338166033E-15 ) ) ;
#38860 = CARTESIAN_POINT ( 'NONE',  ( 6.459375000614518747, 0.000000000000000000, 5.243569643749999010 ) ) ;
#38861 = CARTESIAN_POINT ( 'NONE',  ( 24.56250000122903288, 4.330127018922192761, -2.499999999999997780 ) ) ;
#38862 = CARTESIAN_POINT ( 'NONE',  ( 15.72187500061451892, 3.027376345333612662, -5.243569643749998122 ) ) ;
#38863 = CARTESIAN_POINT ( 'NONE',  ( 3.159375000614518036, 4.541064518000418104, -2.621784821874998173 ) ) ;
#38864 = CARTESIAN_POINT ( 'NONE',  ( 5.000000000000000000, 39.99999999999999289, 15.00000000000000178 ) ) ;
#38865 = CARTESIAN_POINT ( 'NONE',  ( 25.69687500061451502, 6.054752690667223547, 3.707466751127219781E-16 ) ) ;
#38866 = CARTESIAN_POINT ( 'NONE',  ( 12.55312500061451786, 4.541064518000418104, -2.621784821874998173 ) ) ;
#38867 = ORIENTED_EDGE ( 'NONE', *, *, #43418, .T. ) ;
#38868 = CARTESIAN_POINT ( 'NONE',  ( 10.37812500061451715, 4.541064518000418104, 2.621784821874999949 ) ) ;
#38869 = CARTESIAN_POINT ( 'NONE',  ( 7.415625000614516793, -6.054752690667223547, -1.112240025338166033E-15 ) ) ;
#38870 = CARTESIAN_POINT ( 'NONE',  ( 19.47187500061451360, 2.746126346562643317, 4.756430356249998326 ) ) ;
#38871 = CARTESIAN_POINT ( 'NONE',  ( 8.550000000000002487, -4.330127018922190985, -2.500000000000001332 ) ) ;
#38872 = CARTESIAN_POINT ( 'NONE',  ( 2.962500001229034119, 4.330127018922192761, -2.499999999999997780 ) ) ;
#38873 = CARTESIAN_POINT ( 'NONE',  ( 18.56250000000000000, 2.886751345948129099, -4.999999999999998224 ) ) ;
#38874 = CARTESIAN_POINT ( 'NONE',  ( 18.83437500061451431, 6.421520780324663323E-16, -5.243569643749999010 ) ) ;
#38875 = CARTESIAN_POINT ( 'NONE',  ( 14.40000000122903323, -2.886751345948129988, 4.999999999999997335 ) ) ;
#38876 = CARTESIAN_POINT ( 'NONE',  ( 19.61249999999999716, 2.886751345948126879, 4.999999999999999112 ) ) ;
#38877 = CARTESIAN_POINT ( 'NONE',  ( -2.121784821874999949, 14.77812500061451750, -33.67503911421598417 ) ) ;
#38878 = CARTESIAN_POINT ( 'NONE',  ( -4.000000000000000888, 19.96250000000000213, 32.30940107675850470 ) ) ;
#38879 = CARTESIAN_POINT ( 'NONE',  ( 25.20937500061451431, 2.746126346562643317, 4.756430356249998326 ) ) ;
#38880 = DIRECTION ( 'NONE',  ( 0.000000000000000000, 0.000000000000000000, 1.000000000000000000 ) ) ;
#38881 = EDGE_CURVE ( 'NONE', #70720, #30507, #67003, .T. ) ;
#38882 = CARTESIAN_POINT ( 'NONE',  ( 27.21562500061451928, -6.054752690667223547, -1.112240025338166033E-15 ) ) ;
#38883 = CARTESIAN_POINT ( 'NONE',  ( 30.00000000000000000, 0.000000000000000000, 4.999999999999998224 ) ) ;
#38884 = CARTESIAN_POINT ( 'NONE',  ( 0.000000000000000000, 10.00000000000000000, 24.00000000000000000 ) ) ;
#38885 = CARTESIAN_POINT ( 'NONE',  ( 27.15000000000000213, 4.330127018922192761, -2.499999999999997780 ) ) ;
#38886 = CARTESIAN_POINT ( 'NONE',  ( 8.540625000614518569, 6.054752690667223547, 3.707466751127219781E-16 ) ) ;
#38887 = CARTESIAN_POINT ( 'NONE',  ( 26.25937500061451502, -5.492252693125287522, -1.008910452111647106E-15 ) ) ;
#38888 = CARTESIAN_POINT ( 'NONE',  ( 21.30937500061451573, 0.000000000000000000, 5.243569643749999010 ) ) ;
#38889 = CARTESIAN_POINT ( 'NONE',  ( 13.13437500061451502, -2.746126346562646425, 4.756430356249996549 ) ) ;
#38890 = CARTESIAN_POINT ( 'NONE',  ( 5.090625000614516615, -3.027376345333614438, 5.243569643749998122 ) ) ;
#38891 = CARTESIAN_POINT ( 'NONE',  ( 10.13437500061451679, -4.541064518000419881, 2.621784821874995952 ) ) ;
#38892 = VERTEX_POINT ( 'NONE', #9799 ) ;
#38893 = CARTESIAN_POINT ( 'NONE',  ( 22.58437500061451431, 4.541064518000418104, 2.621784821874999949 ) ) ;
#38894 = CARTESIAN_POINT ( 'NONE',  ( 28.91250000000000497, 2.886751345948099789, -5.000000000000048850 ) ) ;
#38895 = CARTESIAN_POINT ( 'NONE',  ( 28.94999999999999929, 4.330127018922192761, -2.499999999999997780 ) ) ;
#38896 = CARTESIAN_POINT ( 'NONE',  ( 4.800000000000002487, 0.000000000000000000, 4.999999999999998224 ) ) ;
#38897 = CARTESIAN_POINT ( 'NONE',  ( 14.66250000122903252, 4.330127018922192761, -2.499999999999997780 ) ) ;
#38898 = DIRECTION ( 'NONE',  ( 0.000000000000000000, 0.000000000000000000, -1.000000000000000000 ) ) ;
#38899 = CARTESIAN_POINT ( 'NONE',  ( 14.58750000122903323, 6.123233995736764310E-16, -4.999999999999998224 ) ) ;
#38900 = ORIENTED_EDGE ( 'NONE', *, *, #10308, .T. ) ;
#38901 = CARTESIAN_POINT ( 'NONE',  ( 11.66249999999999964, -5.773502691896255534, -1.060575238724906372E-15 ) ) ;
#38902 = CARTESIAN_POINT ( 'NONE',  ( 16.42500000000000071, 4.330127018922191873, 2.499999999999999556 ) ) ;
#38903 = CARTESIAN_POINT ( 'NONE',  ( 12.33750000122903145, 6.123233995736764310E-16, -4.999999999999998224 ) ) ;
#38904 = CARTESIAN_POINT ( 'NONE',  ( 10.94062500061451537, -3.027376345333614438, 5.243569643749998122 ) ) ;
#38905 = CARTESIAN_POINT ( 'NONE',  ( 8.137500000000002842, -2.886751345948125991, -5.000000000000000000 ) ) ;
#38906 = FACE_OUTER_BOUND ( 'NONE', #63070, .T. ) ;
#38907 = CARTESIAN_POINT ( 'NONE',  ( -2.121784821874999949, 15.28437500061451892, -33.67503911421598417 ) ) ;
#38908 = CARTESIAN_POINT ( 'NONE',  ( 29.13750000122903216, 4.330127018922191873, 2.499999999999999556 ) ) ;
#38909 = CARTESIAN_POINT ( 'NONE',  ( 2.655984681222220721E-16, 15.45312499938548356, 25.66244784525396483 ) ) ;
#38910 = CARTESIAN_POINT ( 'NONE',  ( 10.42500000000000071, 6.123233995736764310E-16, -4.999999999999998224 ) ) ;
#38911 = CARTESIAN_POINT ( 'NONE',  ( 3.486133158594716510E-16, 19.88749999999999929, -34.00000000000000000 ) ) ;
#38912 = ORIENTED_EDGE ( 'NONE', *, *, #10796, .T. ) ;
#38913 = CARTESIAN_POINT ( 'NONE',  ( 24.25312500061451715, 4.541064518000418104, -2.621784821874998173 ) ) ;
#38914 = CARTESIAN_POINT ( 'NONE',  ( 29.78437500061451715, 4.541064518000418104, 2.621784821874999949 ) ) ;
#38915 = CARTESIAN_POINT ( 'NONE',  ( 20.97187500061451715, -6.054752690667223547, -1.112240025338166033E-15 ) ) ;
#38916 = CARTESIAN_POINT ( 'NONE',  ( 16.26562500061451289, 3.027376345333611329, 5.243569643749999010 ) ) ;
#38917 = ADVANCED_FACE ( 'NONE', ( #48233 ), #49701, .T. ) ;
#38918 = CARTESIAN_POINT ( 'NONE',  ( 4.243569643749999010, 11.51562500061459282, -32.45002607614398471 ) ) ;
#38919 = CARTESIAN_POINT ( 'NONE',  ( 7.565625000614518036, 3.027376345333613106, -5.243569643749998122 ) ) ;
#38920 = CARTESIAN_POINT ( 'NONE',  ( 29.06250000122903288, 4.330127018922192761, -2.499999999999997780 ) ) ;
#38921 = CARTESIAN_POINT ( 'NONE',  ( 23.85937500061451644, 4.119189519843966529, -2.378215178124998275 ) ) ;
#38922 = CARTESIAN_POINT ( 'NONE',  ( 18.29062500061451502, -3.027376345333610441, -5.243569643749999898 ) ) ;
#38923 = CARTESIAN_POINT ( 'NONE',  ( 8.371875000614515727, -5.492252693125287522, -1.008910452111647106E-15 ) ) ;
#38924 = CARTESIAN_POINT ( 'NONE',  ( -1.878215178124999163, 19.09062499938548285, 26.74683588394047007 ) ) ;
#38925 = CARTESIAN_POINT ( 'NONE',  ( 16.17187500061451644, 3.027376345333613106, -5.243569643749998122 ) ) ;
#38926 = CARTESIAN_POINT ( 'NONE',  ( 14.82187500061451679, 3.027376345333613106, -5.243569643749998122 ) ) ;
#38927 = CARTESIAN_POINT ( 'NONE',  ( 22.39687500061451075, -3.027376345333610441, -5.243569643749999898 ) ) ;
#38928 = ORIENTED_EDGE ( 'NONE', *, *, #61885, .F. ) ;
#38929 = CARTESIAN_POINT ( 'NONE',  ( -2.121784821874996840, 12.73437500061451821, 33.67503911421598417 ) ) ;
#38930 = CARTESIAN_POINT ( 'NONE',  ( 3.403125000614518836, -4.541064518000417216, -2.621784821875001281 ) ) ;
#38931 = CARTESIAN_POINT ( 'NONE',  ( 27.10312500061451502, 0.000000000000000000, 5.243569643749999010 ) ) ;
#38932 = EDGE_CURVE ( 'NONE', #60154, #59530, #15330, .T. ) ;
#38933 = CARTESIAN_POINT ( 'NONE',  ( 26.99062500061451431, 6.054752690667223547, 3.707466751127219781E-16 ) ) ;
#38934 = LINE ( 'NONE', #31559, #32437 ) ;
#38935 = CARTESIAN_POINT ( 'NONE',  ( 4.000000000000000000, 17.03750000000000142, 32.30940107675849049 ) ) ;
#38936 = CARTESIAN_POINT ( 'NONE',  ( 5.371875000614516615, 3.027376345333613106, -5.243569643749998122 ) ) ;
#38937 = CARTESIAN_POINT ( 'NONE',  ( 11.55000000122903181, 5.773502691896255534, 3.535250795749688894E-16 ) ) ;
#38938 = CARTESIAN_POINT ( 'NONE',  ( 6.412500001229036073, -4.330127018922190985, -2.500000000000001332 ) ) ;
#38939 = CARTESIAN_POINT ( 'NONE',  ( 28.83750000122903145, -4.330127018922194537, 2.499999999999995559 ) ) ;
#38940 = CARTESIAN_POINT ( 'NONE',  ( 2.000000000000000444, 19.26874999877096784, 26.53589838486224650 ) ) ;
#38941 = CARTESIAN_POINT ( 'NONE',  ( 18.31875000122903430, 2.886751345948126879, 4.999999999999999112 ) ) ;
#38942 = CARTESIAN_POINT ( 'NONE',  ( 11.14687500061451608, -3.027376345333610441, -5.243569643749999898 ) ) ;
#38943 = DIRECTION ( 'NONE',  ( 0.000000000000000000, 0.000000000000000000, -1.000000000000000000 ) ) ;
#38944 = VERTEX_POINT ( 'NONE', #26061 ) ;
#38945 = CARTESIAN_POINT ( 'NONE',  ( 20.01562500061451644, -6.054752690667223547, -1.112240025338166033E-15 ) ) ;
#38946 = CARTESIAN_POINT ( 'NONE',  ( 14.48437500061451821, 4.541064518000418104, 2.621784821874999949 ) ) ;
#38947 = CARTESIAN_POINT ( 'NONE',  ( 4.603125000614518569, 0.000000000000000000, 5.243569643749999010 ) ) ;
#38948 = CARTESIAN_POINT ( 'NONE',  ( 22.99687500061452283, 6.054752690667223547, 3.707466751127219781E-16 ) ) ;
#38949 = CARTESIAN_POINT ( 'NONE',  ( 9.646875000614516082, -3.027376345333614438, 5.243569643749998122 ) ) ;
#38950 = CARTESIAN_POINT ( 'NONE',  ( 4.378125000614518925, 6.421520780324663323E-16, -5.243569643749999010 ) ) ;
#38951 = CARTESIAN_POINT ( 'NONE',  ( 10.87500000122903288, -5.773502691896255534, -1.060575238724906372E-15 ) ) ;
#38952 = CARTESIAN_POINT ( 'NONE',  ( 6.337500001229033231, -4.330127018922194537, 2.499999999999995559 ) ) ;
#38953 = CARTESIAN_POINT ( 'NONE',  ( 20.16562500061451146, 3.027376345333613106, -5.243569643749998122 ) ) ;
#38954 = CARTESIAN_POINT ( 'NONE',  ( 8.100000001229034297, -2.886751345948129988, 4.999999999999997335 ) ) ;
#38955 = CARTESIAN_POINT ( 'NONE',  ( 17.57812500061451644, 4.541064518000418104, 2.621784821874999949 ) ) ;
#38956 = CARTESIAN_POINT ( 'NONE',  ( 15.25312500061451715, 4.541064518000418104, -2.621784821874998173 ) ) ;
#38957 = CARTESIAN_POINT ( 'NONE',  ( 25.20937500061451431, 4.119189519843966529, -2.378215178124998275 ) ) ;
#38958 = CARTESIAN_POINT ( 'NONE',  ( 16.53750000000000142, -2.886751345948129988, 4.999999999999997335 ) ) ;
#38959 = CARTESIAN_POINT ( 'NONE',  ( 8.962500001229033231, 0.000000000000000000, 4.999999999999998224 ) ) ;
#38960 = CARTESIAN_POINT ( 'NONE',  ( 6.328125000614515550, 4.541064518000418104, 2.621784821874999949 ) ) ;
#38961 = APPLICATION_CONTEXT ( 'automotive_design' ) ;
#38962 =( BOUNDED_CURVE ( )  B_SPLINE_CURVE ( 2, ( #36957, #59479, #3360, #62578, #13048, #69579, #68857, #62934, #24501 ),
 .UNSPECIFIED., .F., .F. ) 
 B_SPLINE_CURVE_WITH_KNOTS ( ( 3, 2, 2, 2, 3 ),
 ( 0.4861111111111111049, 0.4907407407407407551, 0.5000000000000000000, 0.5092592592592593004, 0.5138888888888889506 ),
 .UNSPECIFIED. ) 
 CURVE ( )  GEOMETRIC_REPRESENTATION_ITEM ( )  RATIONAL_B_SPLINE_CURVE ( ( 0.9330127018922194093, 0.9330127018922194093, 1.000000000000000000, 0.8660254037844387076, 1.000000000000000000, 0.8660254037844387076, 1.000000000000000000, 0.9330127018922185211, 0.9330127018922192983 ) ) 
 REPRESENTATION_ITEM ( '' )  );
#38963 = CARTESIAN_POINT ( 'NONE',  ( 20.62500000122903288, 2.886751345948126879, 4.999999999999999112 ) ) ;
#38964 = CARTESIAN_POINT ( 'NONE',  ( 27.97500000000000142, 6.123233995736764310E-16, -4.999999999999998224 ) ) ;
#38965 = CARTESIAN_POINT ( 'NONE',  ( 4.243569643749999898, 12.43437500061451750, -30.00000000000000000 ) ) ;
#38966 = CARTESIAN_POINT ( 'NONE',  ( 9.131250001229034297, 6.123233995736764310E-16, -4.999999999999998224 ) ) ;
#38967 = AXIS2_PLACEMENT_3D ( 'NONE', #59017, #8419, #18038 ) ;
#38968 = CARTESIAN_POINT ( 'NONE',  ( 14.98125000122903216, 6.123233995736764310E-16, -4.999999999999998224 ) ) ;
#38969 = CARTESIAN_POINT ( 'NONE',  ( 3.046875000614519990, -3.027376345333610441, -5.243569643749999898 ) ) ;
#38970 = CARTESIAN_POINT ( 'NONE',  ( 20.10937500061451289, -4.541064518000417216, -2.621784821875001281 ) ) ;
#38971 = CARTESIAN_POINT ( 'NONE',  ( 27.67499999999999716, 4.330127018922191873, 2.499999999999999556 ) ) ;
#38972 = CARTESIAN_POINT ( 'NONE',  ( 16.60312500061451857, 4.541064518000418104, -2.621784821874998173 ) ) ;
#38973 = CARTESIAN_POINT ( 'NONE',  ( 11.49375000122903145, 5.773502691896255534, 3.535250795749688894E-16 ) ) ;
#38974 = CARTESIAN_POINT ( 'NONE',  ( 0.6522905807966048464, 20.75364847883808395, 33.69936292076899065 ) ) ;
#38975 = CARTESIAN_POINT ( 'NONE',  ( 13.93125000122903323, -4.330127018922194537, 2.499999999999995559 ) ) ;
#38976 = CARTESIAN_POINT ( 'NONE',  ( 29.29687500061451644, 6.054752690667223547, 3.707466751127219781E-16 ) ) ;
#38977 = CARTESIAN_POINT ( 'NONE',  ( 21.15937500061451715, 2.746126346562643317, 4.756430356249998326 ) ) ;
#38978 = CARTESIAN_POINT ( 'NONE',  ( 13.79062500061451502, -3.027376345333610441, -5.243569643749999898 ) ) ;
#38979 = CARTESIAN_POINT ( 'NONE',  ( 11.93437500061451573, -4.541064518000419881, 2.621784821874995952 ) ) ;
#38980 = EDGE_LOOP ( 'NONE', ( #58263, #44443, #71366, #3267 ) ) ;
#38981 = CARTESIAN_POINT ( 'NONE',  ( 28.90312500061451217, 0.000000000000000000, 5.243569643749999010 ) ) ;
#38982 = CARTESIAN_POINT ( 'NONE',  ( 23.35312500061451857, 4.541064518000418104, -2.621784821874998173 ) ) ;
#38983 = DIRECTION ( 'NONE',  ( 0.000000000000000000, 6.195440985631455317E-17, 1.000000000000000000 ) ) ;
#38984 = LINE ( 'NONE', #32335, #59585 ) ;
#38985 = CARTESIAN_POINT ( 'NONE',  ( 12.22499999999999964, 6.123233995736764310E-16, -4.999999999999998224 ) ) ;
#38986 = CARTESIAN_POINT ( 'NONE',  ( 22.31250000122903288, 4.330127018922192761, -2.499999999999997780 ) ) ;
#38987 = CARTESIAN_POINT ( 'NONE',  ( 15.77812500061451573, 4.541064518000418104, 2.621784821874999949 ) ) ;
#38988 = CARTESIAN_POINT ( 'NONE',  ( 13.43437500061451750, 5.492252693125287522, 3.363034840372157021E-16 ) ) ;
#38989 = ORIENTED_EDGE ( 'NONE', *, *, #53045, .T. ) ;
#38990 = CARTESIAN_POINT ( 'NONE',  ( 20.99999999999999645, 0.000000000000000000, 4.999999999999998224 ) ) ;
#38991 = CARTESIAN_POINT ( 'NONE',  ( 22.39687500061451075, -3.027376345333610441, -5.243569643749999898 ) ) ;
#38992 = CARTESIAN_POINT ( 'NONE',  ( 26.72812500061451502, -4.541064518000419881, 2.621784821874995952 ) ) ;
#38993 = ORIENTED_EDGE ( 'NONE', *, *, #62622, .T. ) ;
#38994 = CYLINDRICAL_SURFACE ( 'NONE', #15941, 4.999999999999998224 ) ;
#38995 = CARTESIAN_POINT ( 'NONE',  ( 10.04062500061451502, -3.027376345333614438, 5.243569643749998122 ) ) ;
#38996 = DIRECTION ( 'NONE',  ( 1.000000000000000000, 0.000000000000000000, 0.000000000000000000 ) ) ;
#38997 = CARTESIAN_POINT ( 'NONE',  ( 18.00000000000000355, -4.330127018922190985, -2.500000000000001332 ) ) ;
#38998 = CARTESIAN_POINT ( 'NONE',  ( 23.32499999999999929, -4.330127018922194537, 2.499999999999995559 ) ) ;
#38999 = CARTESIAN_POINT ( 'NONE',  ( 7.875000000000000000, 4.330127018922191873, 2.499999999999999556 ) ) ;
#39000 = CARTESIAN_POINT ( 'NONE',  ( 4.846875000614519813, -3.027376345333610441, -5.243569643749999898 ) ) ;
#39001 = CARTESIAN_POINT ( 'NONE',  ( 29.55937500061451573, -4.541064518000417216, -2.621784821875001281 ) ) ;
#39002 = EDGE_LOOP ( 'NONE', ( #16072, #55084, #37802, #33800 ) ) ;
#39003 = CARTESIAN_POINT ( 'NONE',  ( 23.20312500061451644, -4.541064518000417216, -2.621784821875001281 ) ) ;
#39004 = CARTESIAN_POINT ( 'NONE',  ( 25.28437500061451715, 4.541064518000418104, 2.621784821874999949 ) ) ;
#39005 = CARTESIAN_POINT ( 'NONE',  ( -3.137519842735245283E-14, 12.91250000000000142, -26.00000000000000711 ) ) ;
#39006 = CARTESIAN_POINT ( 'NONE',  ( 13.16249999999999964, 2.886751345948129099, -4.999999999999998224 ) ) ;
#39007 = CARTESIAN_POINT ( 'NONE',  ( 7.790625000614518569, -3.027376345333614438, 5.243569643749998122 ) ) ;
#39008 = CARTESIAN_POINT ( 'NONE',  ( 2.000000000000000444, 17.46874999877096712, 26.53589838486224650 ) ) ;
#39009 = CARTESIAN_POINT ( 'NONE',  ( 0.6945855708053418898, 20.89427347822356751, 33.93923227099254802 ) ) ;
#39010 = CARTESIAN_POINT ( 'NONE',  ( 25.37812500061451715, -4.541064518000419881, 2.621784821874995952 ) ) ;
#39011 = CARTESIAN_POINT ( 'NONE',  ( 22.63125000122903430, 6.123233995736764310E-16, -4.999999999999998224 ) ) ;
#39012 = CARTESIAN_POINT ( 'NONE',  ( 15.79687500061451821, 5.492252693125287522, 3.363034840372157021E-16 ) ) ;
#39013 = CARTESIAN_POINT ( 'NONE',  ( 3.440625000614518036, -3.027376345333610441, -5.243569643749999898 ) ) ;
#39014 = CARTESIAN_POINT ( 'NONE',  ( 19.05937500061451928, 0.000000000000000000, 5.243569643749999010 ) ) ;
#39015 = CARTESIAN_POINT ( 'NONE',  ( 4.243569643749999898, 13.74687500061451750, 32.45002607614398471 ) ) ;
#39016 = CARTESIAN_POINT ( 'NONE',  ( 22.54687500061451999, 6.054752690667223547, 3.707466751127219781E-16 ) ) ;
#39017 = CARTESIAN_POINT ( 'NONE',  ( 3.525000000000000355, -4.330127018922194537, 2.499999999999995559 ) ) ;
#39018 = CARTESIAN_POINT ( 'NONE',  ( -4.243569643749999898, 19.37187500061451928, 27.54997392385601529 ) ) ;
#39019 = CARTESIAN_POINT ( 'NONE',  ( 10.82812500061451644, 4.541064518000418104, 2.621784821874999949 ) ) ;
#39020 = CARTESIAN_POINT ( 'NONE',  ( 34.99999999999999289, 2.500000000000000444, 3.499999999999999112 ) ) ;
#39021 = ADVANCED_FACE ( 'NONE', ( #43791 ), #43429, .F. ) ;
#39022 = CARTESIAN_POINT ( 'NONE',  ( 6.196875000614515905, -3.027376345333610441, -5.243569643749999898 ) ) ;
#39023 = CARTESIAN_POINT ( 'NONE',  ( 30.00000000000000000, 0.000000000000000000, 0.000000000000000000 ) ) ;
#39024 = CARTESIAN_POINT ( 'NONE',  ( 7.490625000614516082, -3.027376345333610441, -5.243569643749999898 ) ) ;
#39025 = CARTESIAN_POINT ( 'NONE',  ( 11.63437500061451857, 6.421520780324663323E-16, -5.243569643749999010 ) ) ;
#39026 = CARTESIAN_POINT ( 'NONE',  ( 19.31250000122903288, 0.000000000000000000, 4.999999999999998224 ) ) ;
#39027 = CARTESIAN_POINT ( 'NONE',  ( 9.009375000614518569, 4.541064518000418104, -2.621784821874998173 ) ) ;
#39028 = CARTESIAN_POINT ( 'NONE',  ( 9.515625000614518214, 3.027376345333611329, 5.243569643749999010 ) ) ;
#39029 = LINE ( 'NONE', #44936, #36268 ) ;
#39030 = CARTESIAN_POINT ( 'NONE',  ( 25.51875000122903003, 2.886751345948126879, 4.999999999999999112 ) ) ;
#39031 = CARTESIAN_POINT ( 'NONE',  ( 19.39687500061451786, 6.054752690667223547, 3.707466751127219781E-16 ) ) ;
#39032 = CARTESIAN_POINT ( 'NONE',  ( 4.515288692908367096, 2.147595869733109897, 4.674606788361012732 ) ) ;
#39033 = CARTESIAN_POINT ( 'NONE',  ( 26.91562500061451146, 3.027376345333613106, -5.243569643749998122 ) ) ;
#39034 = CARTESIAN_POINT ( 'NONE',  ( 12.25312500061451537, 0.000000000000000000, 5.243569643749999010 ) ) ;
#39035 = CARTESIAN_POINT ( 'NONE',  ( 29.67187500061451644, 3.027376345333612662, -5.243569643749998122 ) ) ;
#39036 = CARTESIAN_POINT ( 'NONE',  ( 4.243569643749999898, 13.29687500061451999, -27.54997392385601529 ) ) ;
#39037 = CARTESIAN_POINT ( 'NONE',  ( 14.02500000122903323, -5.773502691896255534, -1.060575238724906372E-15 ) ) ;
#39038 = CARTESIAN_POINT ( 'NONE',  ( 27.92812500061451431, 4.541064518000418104, 2.621784821874999949 ) ) ;
#39039 = CARTESIAN_POINT ( 'NONE',  ( -4.243569643749999898, 16.16562500061451857, -32.45002607614398471 ) ) ;
#39040 = CARTESIAN_POINT ( 'NONE',  ( 16.27500000122903501, -5.773502691896255534, -1.060575238724906372E-15 ) ) ;
#39041 = CARTESIAN_POINT ( 'NONE',  ( 14.32500000000000107, -4.330127018922194537, 2.499999999999995559 ) ) ;
#39042 = CARTESIAN_POINT ( 'NONE',  ( 12.11250000122903181, 0.000000000000000000, 4.999999999999998224 ) ) ;
#39043 = CARTESIAN_POINT ( 'NONE',  ( 23.12812500061451360, -4.541064518000419881, 2.621784821874995952 ) ) ;
#39044 = CARTESIAN_POINT ( 'NONE',  ( 7.246875000614518392, 6.054752690667223547, 3.707466751127219781E-16 ) ) ;
#39045 = CARTESIAN_POINT ( 'NONE',  ( 9.637500001229033941, 6.123233995736764310E-16, -4.999999999999998224 ) ) ;
#39046 = CARTESIAN_POINT ( 'NONE',  ( 17.62500000122903288, -5.773502691896255534, -1.060575238724906372E-15 ) ) ;
#39047 = CARTESIAN_POINT ( 'NONE',  ( 15.25312500061451715, 4.541064518000418104, -2.621784821874998173 ) ) ;
#39048 = CARTESIAN_POINT ( 'NONE',  ( 18.59062500061451573, -3.027376345333614438, 5.243569643749998122 ) ) ;
#39049 = CARTESIAN_POINT ( 'NONE',  ( 24.63750000122903216, 4.330127018922191873, 2.499999999999999556 ) ) ;
#39050 = CARTESIAN_POINT ( 'NONE',  ( 28.12500000122902932, 2.886751345948129099, -4.999999999999998224 ) ) ;
#39051 = CARTESIAN_POINT ( 'NONE',  ( 21.78750000000000142, 5.773502691896255534, 3.535250795749688894E-16 ) ) ;
#39052 = CARTESIAN_POINT ( 'NONE',  ( 3.756430356249998770, 13.05312499938548321, 32.16877607737302469 ) ) ;
#39053 = CARTESIAN_POINT ( 'NONE',  ( 25.05937500061451573, -4.541064518000417216, -2.621784821875001281 ) ) ;
#39054 = CARTESIAN_POINT ( 'NONE',  ( 25.83750000122903501, 6.123233995736764310E-16, -4.999999999999998224 ) ) ;
#39055 = CARTESIAN_POINT ( 'NONE',  ( 13.05000000122903536, -2.886751345948129988, 4.999999999999997335 ) ) ;
#39056 = CARTESIAN_POINT ( 'NONE',  ( 27.34687500061451360, -3.027376345333610441, -5.243569643749999898 ) ) ;
#39057 = DIRECTION ( 'NONE',  ( -1.000000000000000000, -0.000000000000000000, -0.000000000000000000 ) ) ;
#39058 = CARTESIAN_POINT ( 'NONE',  ( 5.484375000614518214, 4.541064518000418104, 2.621784821874999949 ) ) ;
#39059 = CARTESIAN_POINT ( 'NONE',  ( 23.80312500061451786, 4.541064518000418104, -2.621784821874998173 ) ) ;
#39060 = CARTESIAN_POINT ( 'NONE',  ( 1.878215178125000495, 14.17812499938548321, 26.74683588394047007 ) ) ;
#39061 = CARTESIAN_POINT ( 'NONE',  ( 30.00000000000000000, 6.123233995736764310E-16, -4.999999999999998224 ) ) ;
#39062 = CARTESIAN_POINT ( 'NONE',  ( 9.684375000614517504, -4.541064518000419881, 2.621784821874995952 ) ) ;
#39063 = CARTESIAN_POINT ( 'NONE',  ( 4.947905662033538654, -0.7326246900418315056, 4.992941444957970099 ) ) ;
#39064 = CARTESIAN_POINT ( 'NONE',  ( 29.42812500061451431, -4.541064518000419881, 2.621784821874995952 ) ) ;
#39065 = CARTESIAN_POINT ( 'NONE',  ( 7.284375000614518036, 4.541064518000418104, 2.621784821874999949 ) ) ;
#39066 = CARTESIAN_POINT ( 'NONE',  ( 28.32187500061451502, 3.027376345333613106, -5.243569643749998122 ) ) ;
#39067 = DIRECTION ( 'NONE',  ( -1.000000000000000000, -0.000000000000000000, -0.000000000000000000 ) ) ;
#39068 = CARTESIAN_POINT ( 'NONE',  ( 20.06250000000000000, 2.886751345948126879, 4.999999999999999112 ) ) ;
#39069 = ORIENTED_EDGE ( 'NONE', *, *, #53290, .T. ) ;
#39070 = CARTESIAN_POINT ( 'NONE',  ( 28.23750000000000426, -2.886751345948129988, 4.999999999999997335 ) ) ;
#39071 = CARTESIAN_POINT ( 'NONE',  ( 27.94687500061451502, 6.054752690667223547, 3.707466751127219781E-16 ) ) ;
#39072 = ORIENTED_EDGE ( 'NONE', *, *, #3334, .T. ) ;
#39073 = CARTESIAN_POINT ( 'NONE',  ( 17.69062500061451715, -3.027376345333614438, 5.243569643749998122 ) ) ;
#39074 = CARTESIAN_POINT ( 'NONE',  ( 8.728125000614518569, -4.541064518000419881, 2.621784821874995952 ) ) ;
#39075 = CARTESIAN_POINT ( 'NONE',  ( 20.74687500061451217, 0.000000000000000000, 4.756430356249998326 ) ) ;
#39076 = CARTESIAN_POINT ( 'NONE',  ( 5.784375000614517148, 6.421520780324663323E-16, -5.243569643749999010 ) ) ;
#39077 = CARTESIAN_POINT ( 'NONE',  ( 16.61250000122903359, 0.000000000000000000, 4.999999999999998224 ) ) ;
#39078 = DIRECTION ( 'NONE',  ( -0.000000000000000000, -1.000000000000000000, -0.000000000000000000 ) ) ;
#39079 = CARTESIAN_POINT ( 'NONE',  ( 7.359375000614516438, 0.000000000000000000, 5.243569643749999010 ) ) ;
#39080 = CARTESIAN_POINT ( 'NONE',  ( 12.49687500061451573, -3.027376345333610441, -5.243569643749999898 ) ) ;
#39081 = CARTESIAN_POINT ( 'NONE',  ( 20.59687500061451360, -3.027376345333610441, -5.243569643749999898 ) ) ;
#39082 = EDGE_CURVE ( 'NONE', #11533, #11468, #1409, .T. ) ;
#39083 = CARTESIAN_POINT ( 'NONE',  ( -3.999999999999997335, 16.43750000000000000, 32.30940107675850470 ) ) ;
#39084 = ORIENTED_EDGE ( 'NONE', *, *, #23045, .F. ) ;
#39085 = CARTESIAN_POINT ( 'NONE',  ( 3.871875000614519280, -6.054752690667223547, -1.112240025338166033E-15 ) ) ;
#39086 = CARTESIAN_POINT ( 'NONE',  ( 11.43750000000000000, 5.773502691896255534, 3.535250795749688894E-16 ) ) ;
#39087 = CARTESIAN_POINT ( 'NONE',  ( 7.921875000614517326, -6.054752690667223547, -1.112240025338166033E-15 ) ) ;
#39088 = CARTESIAN_POINT ( 'NONE',  ( -3.756430356250001434, 15.15312499938548463, 32.16877607737301048 ) ) ;
#39089 = CARTESIAN_POINT ( 'NONE',  ( 22.01249999999999574, -5.773502691896255534, -1.060575238724906372E-15 ) ) ;
#39090 = CARTESIAN_POINT ( 'NONE',  ( 18.62812500061451715, -4.541064518000419881, 2.621784821874995952 ) ) ;
#39091 = CARTESIAN_POINT ( 'NONE',  ( -4.000000000000000888, 16.36250000000000071, 32.30940107675850470 ) ) ;
#39092 = CARTESIAN_POINT ( 'NONE',  ( 16.27499999999999858, 6.123233995736764310E-16, -4.999999999999998224 ) ) ;
#39093 = CARTESIAN_POINT ( 'NONE',  ( 22.39687500061451075, -2.746126346562642428, -4.756430356249999214 ) ) ;
#39094 = CARTESIAN_POINT ( 'NONE',  ( 8.915625000614515017, 3.027376345333613106, -5.243569643749998122 ) ) ;
#39095 = CARTESIAN_POINT ( 'NONE',  ( 29.37187500061451928, 3.027376345333611329, 5.243569643749999010 ) ) ;
#39096 = CARTESIAN_POINT ( 'NONE',  ( 29.29687500061451644, 6.054752690667223547, 3.707466751127219781E-16 ) ) ;
#39097 = CARTESIAN_POINT ( 'NONE',  ( 9.899999999999998579, -4.330127018922190985, -2.500000000000001332 ) ) ;
#39098 = CARTESIAN_POINT ( 'NONE',  ( 8.484601909799253346E-16, 15.72500000122903252, 34.61880215351700230 ) ) ;
#39099 = CARTESIAN_POINT ( 'NONE',  ( 8.887500001229033941, 4.330127018922191873, 2.499999999999999556 ) ) ;
#39100 = CARTESIAN_POINT ( 'NONE',  ( 20.67187500061451289, 3.027376345333613106, -5.243569643749998122 ) ) ;
#39101 = CARTESIAN_POINT ( 'NONE',  ( 13.05937500061451750, 4.541064518000418104, -2.621784821874998173 ) ) ;
#39102 = DIRECTION ( 'NONE',  ( -1.000000000000000000, -0.000000000000000000, -0.000000000000000000 ) ) ;
#39103 = VERTEX_POINT ( 'NONE', #54870 ) ;
#39104 = CARTESIAN_POINT ( 'NONE',  ( 14.42812500061451786, 4.541064518000418104, 2.621784821874999949 ) ) ;
#39105 = CARTESIAN_POINT ( 'NONE',  ( 25.27500000122903145, -5.773502691896255534, -1.060575238724906372E-15 ) ) ;
#39106 = CARTESIAN_POINT ( 'NONE',  ( 14.93437500061451750, 4.541064518000418104, 2.621784821874999949 ) ) ;
#39107 = CARTESIAN_POINT ( 'NONE',  ( 27.16875000122903216, 2.886751345948164182, -4.999999999999937828 ) ) ;
#39108 = CARTESIAN_POINT ( 'NONE',  ( 16.49062500061451786, -3.027376345333610441, -5.243569643749999898 ) ) ;
#39109 = CARTESIAN_POINT ( 'NONE',  ( 1.999999999999997335, 20.01874999877096428, 33.46410161513775705 ) ) ;
#39110 = CARTESIAN_POINT ( 'NONE',  ( 27.12187500061451573, 3.027376345333611329, 5.243569643749999010 ) ) ;
#39111 = CARTESIAN_POINT ( 'NONE',  ( -2.121784821874999949, 11.17812500061451786, 26.32496088578401938 ) ) ;
#39112 = CARTESIAN_POINT ( 'NONE',  ( 14.93437500061451750, 4.541064518000418104, 2.621784821874999949 ) ) ;
#39113 = CARTESIAN_POINT ( 'NONE',  ( 15.26250000122903216, 0.000000000000000000, 4.999999999999998224 ) ) ;
#39114 = CARTESIAN_POINT ( 'NONE',  ( 7.509375000614517681, -4.119189519843965641, -2.378215178125001383 ) ) ;
#39115 = CARTESIAN_POINT ( 'NONE',  ( 4.243569643749999898, 19.18437500061451928, -30.00000000000000000 ) ) ;
#39116 =( BOUNDED_CURVE ( )  B_SPLINE_CURVE ( 2, ( #60047, #65600, #9458, #31988, #54522, #26448, #19054, #41612, #13517 ),
 .UNSPECIFIED., .F., .F. ) 
 B_SPLINE_CURVE_WITH_KNOTS ( ( 3, 2, 2, 2, 3 ),
 ( 0.8804347826086956763, 0.8840579710144927938, 0.8913043478260869179, 0.8985507246376811530, 0.9021739130434782705 ),
 .UNSPECIFIED. ) 
 CURVE ( )  GEOMETRIC_REPRESENTATION_ITEM ( )  RATIONAL_B_SPLINE_CURVE ( ( 0.9330127018922194093, 0.9330127018922194093, 1.000000000000000000, 0.8660254037844387076, 1.000000000000000000, 0.8660254037844387076, 1.000000000000000000, 0.9330127018922194093, 0.9330127018922194093 ) ) 
 REPRESENTATION_ITEM ( '' )  );
#39117 = CARTESIAN_POINT ( 'NONE',  ( 20.37187500061451573, 3.027376345333611329, 5.243569643749999010 ) ) ;
#39118 = CARTESIAN_POINT ( 'NONE',  ( 18.93750000122903288, -4.330127018922194537, 2.499999999999995559 ) ) ;
#39119 = CARTESIAN_POINT ( 'NONE',  ( 17.59687500061451715, 6.054752690667223547, 3.707466751127219781E-16 ) ) ;
#39120 = CARTESIAN_POINT ( 'NONE',  ( 2.121784821875001281, 12.35937500061451821, 33.67503911421598417 ) ) ;
#39121 = CARTESIAN_POINT ( 'NONE',  ( 16.56562500061451715, 3.027376345333613106, -5.243569643749998122 ) ) ;
#39122 = ORIENTED_EDGE ( 'NONE', *, *, #16801, .T. ) ;
#39123 = ORIENTED_EDGE ( 'NONE', *, *, #56109, .T. ) ;
#39124 = CARTESIAN_POINT ( 'NONE',  ( 20.47500000000000142, 4.330127018922191873, 2.499999999999999556 ) ) ;
#39125 = CARTESIAN_POINT ( 'NONE',  ( 29.83125000061451715, 0.000000000000000000, 5.243569643749999010 ) ) ;
#39126 = CARTESIAN_POINT ( 'NONE',  ( 24.77812500061451217, 4.541064518000418104, 2.621784821874999949 ) ) ;
#39127 = CARTESIAN_POINT ( 'NONE',  ( 3.703125000614516882, 0.000000000000000000, 5.243569643749999010 ) ) ;
#39128 = CARTESIAN_POINT ( 'NONE',  ( 17.66250000122903430, -4.330127018922190985, -2.500000000000001332 ) ) ;
#39129 = CARTESIAN_POINT ( 'NONE',  ( 21.92812500061451431, 6.421520780324663323E-16, -5.243569643749999010 ) ) ;
#39130 = CARTESIAN_POINT ( 'NONE',  ( 20.92500000000000071, 4.330127018922191873, 2.499999999999999556 ) ) ;
#39131 = CARTESIAN_POINT ( 'NONE',  ( 24.66562500061451502, 3.027376345333613106, -5.243569643749998122 ) ) ;
#39132 = CARTESIAN_POINT ( 'NONE',  ( 5.390625000614518214, 6.054752690667223547, 3.707466751127219781E-16 ) ) ;
#39133 = VERTEX_POINT ( 'NONE', #49335 ) ;
#39134 = CARTESIAN_POINT ( 'NONE',  ( 3.965625000614515727, 3.027376345333613106, -5.243569643749998122 ) ) ;
#39135 = CARTESIAN_POINT ( 'NONE',  ( 11.52187500061451608, -5.492252693125287522, -1.008910452111647106E-15 ) ) ;
#39136 = FACE_OUTER_BOUND ( 'NONE', #67832, .T. ) ;
#39137 = CARTESIAN_POINT ( 'NONE',  ( -1.999999999999997113, 11.63750000122903394, -26.53589838486224295 ) ) ;
#39138 = CARTESIAN_POINT ( 'NONE',  ( -2.121784821874996840, 18.58437500061451786, -26.32496088578401583 ) ) ;
#39139 = STYLED_ITEM ( 'NONE', ( #64437 ), #54116 ) ;
#39140 = CARTESIAN_POINT ( 'NONE',  ( 8.699999999999999289, 4.330127018922192761, -2.499999999999997780 ) ) ;
#39141 = EDGE_CURVE ( 'NONE', #16877, #29218, #37136, .T. ) ;
#39142 = CARTESIAN_POINT ( 'NONE',  ( 4.612500001229032698, -4.330127018922190985, -2.500000000000001332 ) ) ;
#39143 = CARTESIAN_POINT ( 'NONE',  ( 13.28437500061451715, -4.541064518000419881, 2.621784821874995952 ) ) ;
#39144 = CARTESIAN_POINT ( 'NONE',  ( 23.70000000122903216, 5.773502691896255534, 3.535250795749688401E-16 ) ) ;
#39145 = CARTESIAN_POINT ( 'NONE',  ( 3.084375000614519191, 6.421520780324663323E-16, -5.243569643749999010 ) ) ;
#39146 = LINE ( 'NONE', #66865, #35019 ) ;
#39147 = DIRECTION ( 'NONE',  ( 0.000000000000000000, 0.000000000000000000, 1.000000000000000000 ) ) ;
#39148 = CARTESIAN_POINT ( 'NONE',  ( 9.646875000614516082, -3.027376345333614438, 5.243569643749998122 ) ) ;
#39149 = CARTESIAN_POINT ( 'NONE',  ( 45.00000000000000000, 6.123233995736764310E-16, -4.999999999999998224 ) ) ;
#39150 = CARTESIAN_POINT ( 'NONE',  ( 20.39062500061451644, -3.027376345333614438, 5.243569643749998122 ) ) ;
#39151 = CARTESIAN_POINT ( 'NONE',  ( -1.071796769724504328, 12.55490381179670045, -26.00000000000001066 ) ) ;
#39152 =( BOUNDED_CURVE ( )  B_SPLINE_CURVE ( 2, ( #32788, #22062, #16152, #55325, #4719, #44249, #37228 ),
 .UNSPECIFIED., .F., .F. ) 
 B_SPLINE_CURVE_WITH_KNOTS ( ( 3, 2, 2, 3 ),
 ( 0.2750000000000000777, 0.2777777777777778456, 0.2805555555555556135, 0.2833333333333333814 ),
 .UNSPECIFIED. ) 
 CURVE ( )  GEOMETRIC_REPRESENTATION_ITEM ( )  RATIONAL_B_SPLINE_CURVE ( ( 0.9999999999999973355, 0.8660254037844413721, 1.000000000000000000, 0.8660254037844387076, 1.000000000000000000, 0.8660254037844360431, 1.000000000000002665 ) ) 
 REPRESENTATION_ITEM ( '' )  );
#39153 = CARTESIAN_POINT ( 'NONE',  ( -2.121784821874996840, 18.07812500061459104, 33.67503911421598417 ) ) ;
#39154 = CARTESIAN_POINT ( 'NONE',  ( 24.64687500061451431, -3.027376345333610441, -5.243569643749999898 ) ) ;
#39155 = EDGE_CURVE ( 'NONE', #29422, #42476, #8951, .T. ) ;
#39156 = DIRECTION ( 'NONE',  ( -1.000000000000000000, -0.000000000000000000, -0.000000000000000000 ) ) ;
#39157 =( BOUNDED_CURVE ( )  B_SPLINE_CURVE ( 2, ( #40618, #6996, #12533, #23972, #5804, #45332, #23869, #17239, #56760 ),
 .UNSPECIFIED., .F., .F. ) 
 B_SPLINE_CURVE_WITH_KNOTS ( ( 3, 2, 2, 2, 3 ),
 ( 0.5108695652173913526, 0.5144927536231883591, 0.5217391304347825942, 0.5289855072463768293, 0.5326086956521739468 ),
 .UNSPECIFIED. ) 
 CURVE ( )  GEOMETRIC_REPRESENTATION_ITEM ( )  RATIONAL_B_SPLINE_CURVE ( ( 0.9330127018922192983, 0.9330127018922202975, 1.000000000000000000, 0.8660254037844387076, 1.000000000000000000, 0.8660254037844387076, 1.000000000000000000, 0.9330127018922194093, 0.9330127018922194093 ) ) 
 REPRESENTATION_ITEM ( '' )  );
#39158 = CARTESIAN_POINT ( 'NONE',  ( 29.17500000122903714, 2.886751345948126879, 4.999999999999999112 ) ) ;
#39159 = CARTESIAN_POINT ( 'NONE',  ( 20.33437500061451786, -2.746126346562646425, 4.756430356249996549 ) ) ;
#39160 = CARTESIAN_POINT ( 'NONE',  ( 25.94062500061451715, -3.027376345333610441, -5.243569643749999898 ) ) ;
#39161 = CARTESIAN_POINT ( 'NONE',  ( 14.54062500061451679, -3.027376345333614438, 5.243569643749998122 ) ) ;
#39162 = CARTESIAN_POINT ( 'NONE',  ( 13.29375000122903394, 5.773502691896255534, 3.535250795749688894E-16 ) ) ;
#39163 = CARTESIAN_POINT ( 'NONE',  ( 11.74687500061451573, 6.054752690667223547, 3.707466751127219781E-16 ) ) ;
#39164 = CARTESIAN_POINT ( 'NONE',  ( 28.49999999999999645, 4.330127018922192761, -2.499999999999997780 ) ) ;
#39165 = CARTESIAN_POINT ( 'NONE',  ( 24.45000000122903572, -2.886751345948125991, -5.000000000000000000 ) ) ;
#39166 = CARTESIAN_POINT ( 'NONE',  ( 7.781250001229034652, 6.123233995736764310E-16, -4.999999999999998224 ) ) ;
#39167 = CARTESIAN_POINT ( 'NONE',  ( 14.22187500061451537, -6.054752690667223547, -1.112240025338166033E-15 ) ) ;
#39168 = CARTESIAN_POINT ( 'NONE',  ( 29.55937500061451573, -4.541064518000417216, -2.621784821875001281 ) ) ;
#39169 = CARTESIAN_POINT ( 'NONE',  ( 3.155232096411749065, -4.128743534138908267, -2.848806427449918743 ) ) ;
#39170 = CARTESIAN_POINT ( 'NONE',  ( 25.88437500061451502, -4.541064518000419881, 2.621784821874995952 ) ) ;
#39171 = CARTESIAN_POINT ( 'NONE',  ( 14.18437500061451750, -4.541064518000419881, 2.621784821874995952 ) ) ;
#39172 = CARTESIAN_POINT ( 'NONE',  ( 1.878215178124997609, 16.27812499938548285, 33.25316411605952993 ) ) ;
#39173 = CARTESIAN_POINT ( 'NONE',  ( 28.19999999999999929, 0.000000000000000000, 4.999999999999998224 ) ) ;
#39174 = CARTESIAN_POINT ( 'NONE',  ( 3.825000001229032609, 2.886751345948129099, -4.999999999999998224 ) ) ;
#39175 = CARTESIAN_POINT ( 'NONE',  ( 5.625000000000001776, 4.330127018922191873, 2.499999999999999556 ) ) ;
#39176 = CARTESIAN_POINT ( 'NONE',  ( 29.33437500061451431, 4.119189519843966529, 2.378215178124999607 ) ) ;
#39177 = CARTESIAN_POINT ( 'NONE',  ( 20.12812500061451715, 6.421520780324663323E-16, -5.243569643749999010 ) ) ;
#39178 = CARTESIAN_POINT ( 'NONE',  ( 10.57500000000000107, 4.330127018922191873, 2.499999999999999556 ) ) ;
#39179 = CARTESIAN_POINT ( 'NONE',  ( 15.48749999999999893, 5.773502691896255534, 3.535250795749688401E-16 ) ) ;
#39180 = CARTESIAN_POINT ( 'NONE',  ( 17.81250000000000355, 2.886751345948126879, 4.999999999999999112 ) ) ;
#39181 = CARTESIAN_POINT ( 'NONE',  ( -4.243569643749997233, 13.09062500061451750, 32.45002607614398471 ) ) ;
#39182 =( BOUNDED_CURVE ( )  B_SPLINE_CURVE ( 2, ( #26611, #49149, #66124, #55049, #4451, #6623, #24586 ),
 .UNSPECIFIED., .F., .T. ) 
 B_SPLINE_CURVE_WITH_KNOTS ( ( 3, 2, 2, 3 ),
 ( 0.8666666666666666963, 0.8694444444444444642, 0.8722222222222222321, 0.8750000000000000000 ),
 .UNSPECIFIED. ) 
 CURVE ( )  GEOMETRIC_REPRESENTATION_ITEM ( )  RATIONAL_B_SPLINE_CURVE ( ( 1.000000000000000000, 0.8660254037844387076, 1.000000000000000000, 0.8660254037844387076, 1.000000000000000000, 0.8660254037844387076, 1.000000000000000000 ) ) 
 REPRESENTATION_ITEM ( '' )  );
#39183 = CARTESIAN_POINT ( 'NONE',  ( 1.999999999999997335, 18.27499999999999858, 33.46410161513775705 ) ) ;
#39184 = CARTESIAN_POINT ( 'NONE',  ( 21.93750000122903288, 4.330127018922191873, 2.499999999999999556 ) ) ;
#39185 = CARTESIAN_POINT ( 'NONE',  ( -3.999999999999999112, 10.10000000000000142, -30.00000000000000000 ) ) ;
#39186 = CARTESIAN_POINT ( 'NONE',  ( 27.19687500061451857, -3.027376345333614438, 5.243569643749998122 ) ) ;
#39187 = ORIENTED_EDGE ( 'NONE', *, *, #2612, .T. ) ;
#39188 = CARTESIAN_POINT ( 'NONE',  ( 17.20312500061451644, 0.000000000000000000, 5.243569643749999010 ) ) ;
#39189 = CARTESIAN_POINT ( 'NONE',  ( 22.04062500061451502, 6.054752690667223547, 3.707466751127219781E-16 ) ) ;
#39190 = CARTESIAN_POINT ( 'NONE',  ( 22.88437500061451857, 6.421520780324663323E-16, -5.243569643749999010 ) ) ;
#39191 = CARTESIAN_POINT ( 'NONE',  ( 7.050000000000000711, 0.000000000000000000, 4.999999999999998224 ) ) ;
#39192 = CARTESIAN_POINT ( 'NONE',  ( 9.215625000614515727, -6.054752690667223547, -1.112240025338166033E-15 ) ) ;
#39193 = CARTESIAN_POINT ( 'NONE',  ( 24.74062500061451786, 6.054752690667223547, 3.707466751127219781E-16 ) ) ;
#39194 = CARTESIAN_POINT ( 'NONE',  ( 15.68437500061451573, 6.421520780324663323E-16, -5.243569643749999010 ) ) ;
#39195 = CARTESIAN_POINT ( 'NONE',  ( 19.50937500061451857, 0.000000000000000000, 5.243569643749999010 ) ) ;
#39196 = DIRECTION ( 'NONE',  ( -1.000000000000000000, -0.000000000000000000, -0.000000000000000000 ) ) ;
#39197 = CARTESIAN_POINT ( 'NONE',  ( 2.121784821874999061, 17.85312500061451502, 26.32496088578401583 ) ) ;
#39198 = EDGE_CURVE ( 'NONE', #32936, #12269, #16490, .T. ) ;
#39199 = CARTESIAN_POINT ( 'NONE',  ( 21.82500000122903572, 2.886751345948129099, -4.999999999999998224 ) ) ;
#39200 = CARTESIAN_POINT ( 'NONE',  ( 17.33437500061451431, -4.119189519843968306, 2.378215178124996054 ) ) ;
#39201 = CARTESIAN_POINT ( 'NONE',  ( 11.69062500061451537, 6.054752690667223547, 3.707466751127219781E-16 ) ) ;
#39202 = CARTESIAN_POINT ( 'NONE',  ( 5.934375000614517504, 4.541064518000418104, 2.621784821874999949 ) ) ;
#39203 = CARTESIAN_POINT ( 'NONE',  ( 4.396875000614516971, -3.027376345333610441, -5.243569643749999898 ) ) ;
#39204 = EDGE_LOOP ( 'NONE', ( #19838, #72818, #44161, #19467 ) ) ;
#39205 = CARTESIAN_POINT ( 'NONE',  ( 27.12187500061451573, 3.027376345333611329, 5.243569643749999010 ) ) ;
#39206 = CARTESIAN_POINT ( 'NONE',  ( 19.71562500061451928, 3.027376345333613106, -5.243569643749998122 ) ) ;
#39207 = CARTESIAN_POINT ( 'NONE',  ( 26.10000000122903430, -2.886751345948129988, 4.999999999999997335 ) ) ;
#39208 = B_SPLINE_CURVE_WITH_KNOTS ( 'NONE', 3,
 ( #33438, #10552, #38633, #21623, #49354, #11285, #50081, #33806, #61878, #61157 ),
 .UNSPECIFIED., .F., .F.,
 ( 4, 3, 3, 4 ),
 ( 0.000000000000000000, 7.861372412303096113E-05, 0.0001572277528824084529, 0.0002833172372400243359 ),
 .UNSPECIFIED. ) ;
#39209 = CARTESIAN_POINT ( 'NONE',  ( 26.84062500061451573, -3.027376345333610441, -5.243569643749999898 ) ) ;
#39210 = VECTOR ( 'NONE', #18559, 1000.000000000000000 ) ;
#39211 = CARTESIAN_POINT ( 'NONE',  ( 23.07187500061451857, 3.027376345333611329, 5.243569643749999010 ) ) ;
#39212 = CARTESIAN_POINT ( 'NONE',  ( 18.96562500061451573, 3.027376345333611329, 5.243569643749999010 ) ) ;
#39213 = CARTESIAN_POINT ( 'NONE',  ( -3.999999999999999112, 10.10000000000000142, 30.00000000000000000 ) ) ;
#39214 = CARTESIAN_POINT ( 'NONE',  ( 24.21562500061451573, 3.027376345333613106, -5.243569643749998122 ) ) ;
#39215 = CARTESIAN_POINT ( 'NONE',  ( 5.587500001229033231, 6.123233995736764310E-16, -4.999999999999998224 ) ) ;
#39216 = ORIENTED_EDGE ( 'NONE', *, *, #45678, .F. ) ;
#39217 = CARTESIAN_POINT ( 'NONE',  ( 27.03750000000000142, -2.886751345948125991, -5.000000000000000000 ) ) ;
#39218 = CARTESIAN_POINT ( 'NONE',  ( 8.484601909799253346E-16, 14.71250000000000036, -25.38119784648299770 ) ) ;
#39219 = CARTESIAN_POINT ( 'NONE',  ( -1.878215178124999163, 18.30312499938548143, 26.74683588394047007 ) ) ;
#39220 = CARTESIAN_POINT ( 'NONE',  ( 5.896875000614518747, 6.054752690667223547, 3.707466751127219781E-16 ) ) ;
#39221 = CARTESIAN_POINT ( 'NONE',  ( 12.55312500061451786, 4.541064518000418104, -2.621784821874998173 ) ) ;
#39222 = CARTESIAN_POINT ( 'NONE',  ( 7.284375000614518036, 4.541064518000418104, 2.621784821874999949 ) ) ;
#39223 = CARTESIAN_POINT ( 'NONE',  ( 24.82500000122902861, -5.773502691896255534, -1.060575238724906372E-15 ) ) ;
#39224 = CARTESIAN_POINT ( 'NONE',  ( 15.60937500061451644, -4.541064518000417216, -2.621784821875001281 ) ) ;
#39225 = CARTESIAN_POINT ( 'NONE',  ( 29.05312500061451431, -4.541064518000417216, -2.621784821875001281 ) ) ;
#39226 = CARTESIAN_POINT ( 'NONE',  ( 26.84999999999999787, 0.000000000000000000, 4.999999999999998224 ) ) ;
#39227 = CARTESIAN_POINT ( 'NONE',  ( 27.27187500061451431, -6.054752690667223547, -1.112240025338166033E-15 ) ) ;
#39228 = CARTESIAN_POINT ( 'NONE',  ( 3.703125000614516882, 0.000000000000000000, 5.243569643749999010 ) ) ;
#39229 = CARTESIAN_POINT ( 'NONE',  ( 13.97812500061451679, 4.541064518000418104, 2.621784821874999949 ) ) ;
#39230 = ORIENTED_EDGE ( 'NONE', *, *, #57275, .F. ) ;
#39231 = CARTESIAN_POINT ( 'NONE',  ( 9.328125000614518214, 6.421520780324663323E-16, -5.243569643749999010 ) ) ;
#39232 = CARTESIAN_POINT ( 'NONE',  ( 5.578125000614518214, -4.541064518000419881, 2.621784821874995952 ) ) ;
#39233 = CARTESIAN_POINT ( 'NONE',  ( 19.84687500061451360, 5.492252693125287522, 3.363034840372157021E-16 ) ) ;
#39234 = CARTESIAN_POINT ( 'NONE',  ( -0.6945863667395647534, 9.663023495605401081, 26.06076786935074097 ) ) ;
#39235 = CARTESIAN_POINT ( 'NONE',  ( 15.48749999999999893, 5.773502691896255534, 3.535250795749688894E-16 ) ) ;
#39236 = CARTESIAN_POINT ( 'NONE',  ( 15.53437500061451715, -4.541064518000419881, 2.621784821874995952 ) ) ;
#39237 = CARTESIAN_POINT ( 'NONE',  ( 14.36250000122903359, 0.000000000000000000, 4.999999999999998224 ) ) ;
#39238 = CARTESIAN_POINT ( 'NONE',  ( 19.08750000000000213, 5.773502691896255534, 3.535250795749688894E-16 ) ) ;
#39239 = CARTESIAN_POINT ( 'NONE',  ( 21.75937500061451502, 0.000000000000000000, 5.243569643749999010 ) ) ;
#39240 = CARTESIAN_POINT ( 'NONE',  ( -3.000416591977282496E-16, 13.39062500061451644, -34.90005215228797653 ) ) ;
#39241 = CARTESIAN_POINT ( 'NONE',  ( 21.63749999999999929, -2.886751345948126435, -5.000000000000000000 ) ) ;
#39242 = CARTESIAN_POINT ( 'NONE',  ( 24.72187500061451360, 4.119189519843966529, 2.378215178124999607 ) ) ;
#39243 = CARTESIAN_POINT ( 'NONE',  ( 20.54999999999999716, 0.000000000000000000, 4.999999999999998224 ) ) ;
#39244 = CARTESIAN_POINT ( 'NONE',  ( 26.84062500061451573, -3.027376345333610441, -5.243569643749999898 ) ) ;
#39245 = CARTESIAN_POINT ( 'NONE',  ( 24.89999999999999858, 4.330127018922192761, -2.499999999999997780 ) ) ;
#39246 = LINE ( 'NONE', #50335, #51417 ) ;
#39247 = EDGE_CURVE ( 'NONE', #11634, #36225, #980, .T. ) ;
#39248 = CARTESIAN_POINT ( 'NONE',  ( 26.09999999999999787, -4.330127018922190985, -2.500000000000001332 ) ) ;
#39249 = CARTESIAN_POINT ( 'NONE',  ( 9.253125000614517148, -4.541064518000417216, -2.621784821875001281 ) ) ;
#39250 = AXIS2_PLACEMENT_3D ( 'NONE', #52529, #51806, #41803 ) ;
#39251 = CARTESIAN_POINT ( 'NONE',  ( 27.12187500061451573, -4.119189519843968306, 2.378215178124996054 ) ) ;
#39252 = CARTESIAN_POINT ( 'NONE',  ( 21.79687500061451644, -3.027376345333614438, 5.243569643749998122 ) ) ;
#39253 = CARTESIAN_POINT ( 'NONE',  ( 13.35937500061451644, 2.746126346562645981, -4.756430356249997438 ) ) ;
#39254 = CARTESIAN_POINT ( 'NONE',  ( 4.303125000614516971, -4.541064518000417216, -2.621784821875001281 ) ) ;
#39255 = CARTESIAN_POINT ( 'NONE',  ( 10.65937500061451715, -4.541064518000417216, -2.621784821875001281 ) ) ;
#39256 = ORIENTED_EDGE ( 'NONE', *, *, #35197, .F. ) ;
#39257 = CARTESIAN_POINT ( 'NONE',  ( 20.63437500061451857, 6.421520780324663323E-16, -5.243569643749999010 ) ) ;
#39258 = CYLINDRICAL_SURFACE ( 'NONE', #19389, 4.000000000000000000 ) ;
#39259 = CARTESIAN_POINT ( 'NONE',  ( 29.73750000000000071, -2.886751345948125991, -5.000000000000000000 ) ) ;
#39260 = CARTESIAN_POINT ( 'NONE',  ( 3.900000000000000799, 0.000000000000000000, 4.999999999999998224 ) ) ;
#39261 = CARTESIAN_POINT ( 'NONE',  ( 15.33750000122903323, -4.330127018922194537, 2.499999999999995559 ) ) ;
#39262 = CARTESIAN_POINT ( 'NONE',  ( 1.071796769724497445, 15.36740381056766758, -33.99999999999998579 ) ) ;
#39263 = CARTESIAN_POINT ( 'NONE',  ( -2.000000000000000000, 19.02499999999999858, -33.46410161513775705 ) ) ;
#39264 = EDGE_LOOP ( 'NONE', ( #66946, #9925, #62372, #9359 ) ) ;
#39265 = CARTESIAN_POINT ( 'NONE',  ( 13.98750000000000249, -2.886751345948125991, -5.000000000000000000 ) ) ;
#39266 = CARTESIAN_POINT ( 'NONE',  ( 25.97812500061451502, 6.421520780324663323E-16, -5.243569643749999010 ) ) ;
#39267 = CARTESIAN_POINT ( 'NONE',  ( 17.43750000000000355, -2.886751345948129988, 4.999999999999997335 ) ) ;
#39268 = CARTESIAN_POINT ( 'NONE',  ( 10.31250000122903288, 0.000000000000000000, 4.999999999999998224 ) ) ;
#39269 = CARTESIAN_POINT ( 'NONE',  ( 7.978125000614517681, 6.421520780324663323E-16, -5.243569643749999010 ) ) ;
#39270 = CARTESIAN_POINT ( 'NONE',  ( 8.025000000000000355, -4.330127018922194537, 2.499999999999995559 ) ) ;
#39271 = DIRECTION ( 'NONE',  ( -0.000000000000000000, -1.000000000000000000, -0.000000000000000000 ) ) ;
#39272 = CARTESIAN_POINT ( 'NONE',  ( -3.000416591977282496E-16, 15.69687500061451857, -34.90005215228797653 ) ) ;
#39273 = CARTESIAN_POINT ( 'NONE',  ( 27.15000000122902790, -2.886751345948125991, -5.000000000000000000 ) ) ;
#39274 = CARTESIAN_POINT ( 'NONE',  ( -1.878215178124999163, 15.94062499938548427, 26.74683588394047007 ) ) ;
#39275 = CARTESIAN_POINT ( 'NONE',  ( 7.875000000000000000, 4.330127018922191873, 2.499999999999999556 ) ) ;
#39276 = LINE ( 'NONE', #24348, #42067 ) ;
#39277 = ORIENTED_EDGE ( 'NONE', *, *, #703, .T. ) ;
#39278 = CARTESIAN_POINT ( 'NONE',  ( 25.45312500061451644, -4.541064518000417216, -2.621784821875001281 ) ) ;
#39279 = CARTESIAN_POINT ( 'NONE',  ( 28.94062500061452070, -3.027376345333614438, 5.243569643749998122 ) ) ;
#39280 = CARTESIAN_POINT ( 'NONE',  ( 19.01250000122903216, -4.330127018922190985, -2.500000000000001332 ) ) ;
#39281 = CARTESIAN_POINT ( 'NONE',  ( 21.15937500061451715, 4.541064518000418104, -2.621784821874998173 ) ) ;
#39282 = CARTESIAN_POINT ( 'NONE',  ( 17.42812500061451786, 6.421520780324663323E-16, -5.243569643749999010 ) ) ;
#39283 = CARTESIAN_POINT ( 'NONE',  ( 4.243569643749999010, 12.41562500061459495, -32.45002607614398471 ) ) ;
#39284 = CARTESIAN_POINT ( 'NONE',  ( 6.365625000614518747, 3.027376345333611329, 5.243569643749999010 ) ) ;
#39285 = CARTESIAN_POINT ( 'NONE',  ( 29.66250000122903074, 0.000000000000000000, 4.999999999999998224 ) ) ;
#39286 = CARTESIAN_POINT ( 'NONE',  ( 25.20937500061451431, 4.119189519843966529, -2.378215178124998275 ) ) ;
#39287 = CARTESIAN_POINT ( 'NONE',  ( 19.11562500061451431, -6.054752690667223547, -1.112240025338166033E-15 ) ) ;
#39288 = CARTESIAN_POINT ( 'NONE',  ( -5.810221930991193690E-16, 14.03750000000000142, 26.00000000000000355 ) ) ;
#39289 = CARTESIAN_POINT ( 'NONE',  ( -3.756430356250000102, 19.16562499938548214, 30.00000000000000000 ) ) ;
#39290 = CARTESIAN_POINT ( 'NONE',  ( 13.35937500061451821, -4.541064518000417216, -2.621784821875001281 ) ) ;
#39291 = CARTESIAN_POINT ( 'NONE',  ( 13.62187500061451750, 3.027376345333611329, 5.243569643749999010 ) ) ;
#39292 = CARTESIAN_POINT ( 'NONE',  ( 21.57187500061451502, 3.027376345333613106, -5.243569643749998122 ) ) ;
#39293 = EDGE_LOOP ( 'NONE', ( #40018, #32266, #72381, #2725 ) ) ;
#39294 = CARTESIAN_POINT ( 'NONE',  ( 3.440625000614518036, -3.027376345333610441, -5.243569643749999898 ) ) ;
#39295 = CARTESIAN_POINT ( 'NONE',  ( 25.67812500061451431, 4.541064518000418104, 2.621784821874999949 ) ) ;
#39296 = CARTESIAN_POINT ( 'NONE',  ( 26.31562500061451715, -6.054752690667223547, -1.112240025338166033E-15 ) ) ;
#39297 = CARTESIAN_POINT ( 'NONE',  ( 17.26875000122903003, 2.886751345948185055, -4.999999999999902300 ) ) ;
#39298 = CARTESIAN_POINT ( 'NONE',  ( -2.828200636599751609E-16, 15.83750000000000036, 25.38119784648299770 ) ) ;
#39299 = CARTESIAN_POINT ( 'NONE',  ( 4.209375000614516971, 0.000000000000000000, 5.243569643749999010 ) ) ;
#39300 = CONTEXT_DEPENDENT_SHAPE_REPRESENTATION ( #62997, #7156 ) ;
#39301 = CARTESIAN_POINT ( 'NONE',  ( 11.02500000122903501, 2.886751345948129099, -4.999999999999998224 ) ) ;
#39302 = B_SPLINE_CURVE_WITH_KNOTS ( 'NONE', 3,
 ( #56806, #6212, #22111, #17641, #40201, #34640, #29112, #51646, #1047, #68640 ),
 .UNSPECIFIED., .F., .F.,
 ( 4, 3, 3, 4 ),
 ( 0.000000000000000000, 2.812505145549477149E-05, 5.585677060009500101E-05, 8.358888089303753656E-05 ),
 .UNSPECIFIED. ) ;
#39303 = CARTESIAN_POINT ( 'NONE',  ( 6.037500001229035185, 6.123233995736764310E-16, -4.999999999999998224 ) ) ;
#39304 = CARTESIAN_POINT ( 'NONE',  ( 3.253125000614518036, 0.000000000000000000, 5.243569643749999010 ) ) ;
#39305 = CARTESIAN_POINT ( 'NONE',  ( 2.000000000000000444, 18.36874999877096570, 26.53589838486224650 ) ) ;
#39306 = CARTESIAN_POINT ( 'NONE',  ( 19.78125000122902932, -4.330127018922194537, 2.499999999999995559 ) ) ;
#39307 = CARTESIAN_POINT ( 'NONE',  ( 12.04687500061451821, -3.027376345333610441, -5.243569643749999898 ) ) ;
#39308 = CARTESIAN_POINT ( 'NONE',  ( 24.60000000000000142, 0.000000000000000000, 4.999999999999998224 ) ) ;
#39309 = VERTEX_POINT ( 'NONE', #50062 ) ;
#39310 = EDGE_CURVE ( 'NONE', #2356, #11533, #24029, .T. ) ;
#39311 = CARTESIAN_POINT ( 'NONE',  ( 19.45312500061451644, 0.000000000000000000, 5.243569643749999010 ) ) ;
#39312 = CARTESIAN_POINT ( 'NONE',  ( 14.44687500061451679, 6.054752690667223547, 3.707466751127219781E-16 ) ) ;
#39313 = CARTESIAN_POINT ( 'NONE',  ( 4.003125000614518925, 4.541064518000418104, -2.621784821874998173 ) ) ;
#39314 = CARTESIAN_POINT ( 'NONE',  ( 21.87187500061451573, -6.054752690667223547, -1.112240025338166033E-15 ) ) ;
#39315 = CARTESIAN_POINT ( 'NONE',  ( 10.02187500061451964, 3.027376345333611329, 5.243569643749999010 ) ) ;
#39316 = CARTESIAN_POINT ( 'NONE',  ( 4.115625000614516082, 3.027376345333611329, 5.243569643749999010 ) ) ;
#39317 = CARTESIAN_POINT ( 'NONE',  ( 5.924999999999999822, 6.123233995736764310E-16, -4.999999999999998224 ) ) ;
#39318 = CARTESIAN_POINT ( 'NONE',  ( 5.250000001229035540, 5.773502691896255534, 3.535250795749688894E-16 ) ) ;
#39319 = CARTESIAN_POINT ( 'NONE',  ( 19.22812500061451502, 6.421520780324663323E-16, -5.243569643749999010 ) ) ;
#39320 = CARTESIAN_POINT ( 'NONE',  ( 9.150000001229033231, -2.886751345948125991, -5.000000000000000000 ) ) ;
#39321 = CARTESIAN_POINT ( 'NONE',  ( 17.46562500061451217, 3.027376345333613106, -5.243569643749998122 ) ) ;
#39322 = CARTESIAN_POINT ( 'NONE',  ( 16.75312500061451715, 0.000000000000000000, 5.243569643749999010 ) ) ;
#39323 = CARTESIAN_POINT ( 'NONE',  ( 25.24687500061451573, 5.492252693125287522, 3.363034840372157021E-16 ) ) ;
#39324 = CARTESIAN_POINT ( 'NONE',  ( 14.77500000000000036, -4.330127018922194537, 2.499999999999995559 ) ) ;
#39325 = CARTESIAN_POINT ( 'NONE',  ( 8.325000001229033941, 2.886751345948129099, -4.999999999999998224 ) ) ;
#39326 = CARTESIAN_POINT ( 'NONE',  ( 5.540625000614515905, -3.027376345333614438, 5.243569643749998122 ) ) ;
#39327 = CARTESIAN_POINT ( 'NONE',  ( 20.02500000122903145, 2.886751345948129099, -4.999999999999998224 ) ) ;
#39328 = CARTESIAN_POINT ( 'NONE',  ( 27.93750000000000000, -2.886751345948125991, -5.000000000000000000 ) ) ;
#39329 = CARTESIAN_POINT ( 'NONE',  ( -2.121784821874996840, 12.28437500061451892, -26.32496088578401583 ) ) ;
#39330 = CARTESIAN_POINT ( 'NONE',  ( 4.602184248673647282, -1.954755528723157942, 4.813238914019062342 ) ) ;
#39331 = CARTESIAN_POINT ( 'NONE',  ( 23.96249999999999858, 2.886751345948095793, -5.000000000000055067 ) ) ;
#39332 = CARTESIAN_POINT ( 'NONE',  ( 5.034375000614519813, 4.541064518000418104, 2.621784821874999949 ) ) ;
#39333 = CARTESIAN_POINT ( 'NONE',  ( 21.45937500061451786, -4.541064518000417216, -2.621784821875001281 ) ) ;
#39334 = EDGE_CURVE ( 'NONE', #29028, #25827, #44293, .T. ) ;
#39335 = CARTESIAN_POINT ( 'NONE',  ( 5.000000000000000000, 6.123233995736766282E-16, 50.00000000000000000 ) ) ;
#39336 = CARTESIAN_POINT ( 'NONE',  ( 17.35312500061451502, -4.541064518000417216, -2.621784821875001281 ) ) ;
#39337 = CARTESIAN_POINT ( 'NONE',  ( 12.39375000122903181, 5.773502691896255534, 3.535250795749688894E-16 ) ) ;
#39338 = CARTESIAN_POINT ( 'NONE',  ( 13.12500000000000178, 6.123233995736764310E-16, -4.999999999999998224 ) ) ;
#39339 = CARTESIAN_POINT ( 'NONE',  ( 13.89375000122902648, -2.886751345948019409, 5.000000000000189182 ) ) ;
#39340 = CARTESIAN_POINT ( 'NONE',  ( 28.58437500061451786, -4.541064518000419881, 2.621784821874995952 ) ) ;
#39341 = CARTESIAN_POINT ( 'NONE',  ( 21.42187500061451644, 5.824947211148865298E-16, -4.756430356249998326 ) ) ;
#39342 = CARTESIAN_POINT ( 'NONE',  ( 13.37812500061451715, 6.421520780324663323E-16, -5.243569643749999010 ) ) ;
#39343 = CARTESIAN_POINT ( 'NONE',  ( 10.50937500061451679, 0.000000000000000000, 5.243569643749999010 ) ) ;
#39344 = ORIENTED_EDGE ( 'NONE', *, *, #65317, .F. ) ;
#39345 = CARTESIAN_POINT ( 'NONE',  ( 29.61562500061451431, 3.027376345333613106, -5.243569643749998122 ) ) ;
#39346 = CARTESIAN_POINT ( 'NONE',  ( 23.12812500061451360, -4.541064518000419881, 2.621784821874995952 ) ) ;
#39347 = DIRECTION ( 'NONE',  ( 1.000000000000000000, 0.000000000000000000, 0.000000000000000000 ) ) ;
#39348 = CARTESIAN_POINT ( 'NONE',  ( 1.626862140677534273E-15, 13.02500000122903323, 34.00000000000000000 ) ) ;
#39349 = CARTESIAN_POINT ( 'NONE',  ( 12.63749999999999929, -2.886751345948125991, -5.000000000000000000 ) ) ;
#39350 = CARTESIAN_POINT ( 'NONE',  ( 21.22500000122903074, -5.773502691896255534, -1.060575238724906372E-15 ) ) ;
#39351 = CARTESIAN_POINT ( 'NONE',  ( 16.94062500061451715, -3.027376345333610441, -5.243569643749999898 ) ) ;
#39352 = CARTESIAN_POINT ( 'NONE',  ( 13.35937500061451644, 2.746126346562645981, -4.756430356249997438 ) ) ;
#39353 = ORIENTED_EDGE ( 'NONE', *, *, #72743, .T. ) ;
#39354 = CARTESIAN_POINT ( 'NONE',  ( 19.83750000000000213, -2.886751345948125991, -5.000000000000000000 ) ) ;
#39355 = CARTESIAN_POINT ( 'NONE',  ( 24.63749999999999574, -2.886751345948129988, 4.999999999999997335 ) ) ;
#39356 = CARTESIAN_POINT ( 'NONE',  ( 22.32187500061451502, -6.054752690667223547, -1.112240025338166033E-15 ) ) ;
#39357 = CARTESIAN_POINT ( 'NONE',  ( 24.85312500061451502, 0.000000000000000000, 5.243569643749999010 ) ) ;
#39358 = VERTEX_POINT ( 'NONE', #912 ) ;
#39359 = DIRECTION ( 'NONE',  ( -1.000000000000000000, -0.000000000000000000, -0.000000000000000000 ) ) ;
#39360 = CARTESIAN_POINT ( 'NONE',  ( 8.278125000614515727, -4.541064518000419881, 2.621784821874995952 ) ) ;
#39361 = CARTESIAN_POINT ( 'NONE',  ( 11.10000000000000142, 0.000000000000000000, 4.999999999999998224 ) ) ;
#39362 = CARTESIAN_POINT ( 'NONE',  ( 14.24999999999999822, 0.000000000000000000, 4.999999999999998224 ) ) ;
#39363 = CARTESIAN_POINT ( 'NONE',  ( 7.800000001229035362, -2.886751345948126435, -5.000000000000000000 ) ) ;
#39364 = CARTESIAN_POINT ( 'NONE',  ( 5.221875000614519813, -6.054752690667223547, -1.112240025338166033E-15 ) ) ;
#39365 = CARTESIAN_POINT ( 'NONE',  ( 28.54687500061451644, -3.027376345333614438, 5.243569643749998122 ) ) ;
#39366 = ORIENTED_EDGE ( 'NONE', *, *, #67227, .T. ) ;
#39367 = CARTESIAN_POINT ( 'NONE',  ( 23.35312500061451857, 4.541064518000418104, -2.621784821874998173 ) ) ;
#39368 = CARTESIAN_POINT ( 'NONE',  ( 25.13437500061451502, 6.421520780324663323E-16, -5.243569643749999010 ) ) ;
#39369 = CARTESIAN_POINT ( 'NONE',  ( -4.243569643749998122, 18.04062500061459318, -27.54997392385601174 ) ) ;
#39370 = CARTESIAN_POINT ( 'NONE',  ( 11.40000000000000036, 4.330127018922192761, -2.499999999999997780 ) ) ;
#39371 = CARTESIAN_POINT ( 'NONE',  ( 9.628125000614517148, -4.541064518000419881, 2.621784821874995952 ) ) ;
#39372 = CARTESIAN_POINT ( 'NONE',  ( 3.735381814749570761, 3.323750120342865433, 3.996720557861077161 ) ) ;
#39373 = CARTESIAN_POINT ( 'NONE',  ( 26.65312500061451573, 0.000000000000000000, 5.243569643749999010 ) ) ;
#39374 = CARTESIAN_POINT ( 'NONE',  ( 13.62187500061451750, 2.746126346562643317, 4.756430356249998326 ) ) ;
#39375 = CARTESIAN_POINT ( 'NONE',  ( 3.253125000614518036, 0.000000000000000000, 5.243569643749999010 ) ) ;
#39376 = CARTESIAN_POINT ( 'NONE',  ( 19.77187500061451786, 3.027376345333613106, -5.243569643749998122 ) ) ;
#39377 = CARTESIAN_POINT ( 'NONE',  ( 4.243569643749999898, 15.58437500061451786, 30.00000000000000000 ) ) ;
#39378 = CARTESIAN_POINT ( 'NONE',  ( 21.34687500061451715, -3.027376345333614438, 5.243569643749998122 ) ) ;
#39379 = CARTESIAN_POINT ( 'NONE',  ( 3.825000000000001954, 4.330127018922191873, 2.499999999999999556 ) ) ;
#39380 = CARTESIAN_POINT ( 'NONE',  ( 2.121784821874999061, 18.80937500061451928, 26.32496088578401583 ) ) ;
#39381 = CARTESIAN_POINT ( 'NONE',  ( 9.778125000614517504, 6.421520780324663323E-16, -5.243569643749999010 ) ) ;
#39382 = CARTESIAN_POINT ( 'NONE',  ( 2.737500001229034474, -4.330127018922194537, 2.499999999999995559 ) ) ;
#39383 = CARTESIAN_POINT ( 'NONE',  ( 6.009375000614519458, 0.000000000000000000, 5.243569643749999010 ) ) ;
#39384 = CYLINDRICAL_SURFACE ( 'NONE', #22984, 4.999999999999998224 ) ;
#39385 = CARTESIAN_POINT ( 'NONE',  ( 6.665625000614515905, 3.027376345333613106, -5.243569643749998122 ) ) ;
#39386 = CARTESIAN_POINT ( 'NONE',  ( 11.74687500061451573, 6.054752690667223547, 3.707466751127219781E-16 ) ) ;
#39387 = FILL_AREA_STYLE_COLOUR ( '', #34382 ) ;
#39388 = CARTESIAN_POINT ( 'NONE',  ( 19.72500000122903074, 2.886751345948126879, 4.999999999999999112 ) ) ;
#39389 = CARTESIAN_POINT ( 'NONE',  ( 8.709375000614517859, 0.000000000000000000, 5.243569643749999010 ) ) ;
#39390 = CARTESIAN_POINT ( 'NONE',  ( 9.290625000614515017, -3.027376345333610441, -5.243569643749999898 ) ) ;
#39391 = CARTESIAN_POINT ( 'NONE',  ( 4.903125000614516615, 4.541064518000418104, -2.621784821874998173 ) ) ;
#39392 = CARTESIAN_POINT ( 'NONE',  ( 26.68125000122903145, 6.123233995736764310E-16, -4.999999999999998224 ) ) ;
#39393 = CARTESIAN_POINT ( 'NONE',  ( 18.60937500061451644, 0.000000000000000000, 5.243569643749999010 ) ) ;
#39394 = CARTESIAN_POINT ( 'NONE',  ( 1.626862140677534273E-15, 11.67500000122903181, 34.00000000000000000 ) ) ;
#39395 = CARTESIAN_POINT ( 'NONE',  ( 28.15312500061451573, -4.541064518000417216, -2.621784821875001281 ) ) ;
#39396 = CARTESIAN_POINT ( 'NONE',  ( 10.97812500061451679, -4.541064518000419881, 2.621784821874995952 ) ) ;
#39397 = CARTESIAN_POINT ( 'NONE',  ( 2.867942972713479755, -4.095717654485441450, 3.274159358307528134 ) ) ;
#39398 = CARTESIAN_POINT ( 'NONE',  ( -2.121784821874996840, 11.83437500061451786, -26.32496088578401583 ) ) ;
#39399 = CARTESIAN_POINT ( 'NONE',  ( 12.00000000122903465, 5.773502691896255534, 3.535250795749688894E-16 ) ) ;
#39400 = EDGE_CURVE ( 'NONE', #3790, #2494, #709, .T. ) ;
#39401 =( BOUNDED_CURVE ( )  B_SPLINE_CURVE ( 2, ( #30696, #31804, #64311, #53228, #42886, #20333, #36604 ),
 .UNSPECIFIED., .F., .F. ) 
 B_SPLINE_CURVE_WITH_KNOTS ( ( 3, 2, 2, 3 ),
 ( 0.5666666666666667629, 0.5694444444444445308, 0.5722222222222221877, 0.5749999999999999556 ),
 .UNSPECIFIED. ) 
 CURVE ( )  GEOMETRIC_REPRESENTATION_ITEM ( )  RATIONAL_B_SPLINE_CURVE ( ( 0.9999999999999946709, 0.8660254037844440367, 1.000000000000000000, 0.8660254037844387076, 1.000000000000000000, 0.8660254037844387076, 1.000000000000000000 ) ) 
 REPRESENTATION_ITEM ( '' )  );
#39402 = CARTESIAN_POINT ( 'NONE',  ( 27.14062500061451644, -3.027376345333614438, 5.243569643749998122 ) ) ;
#39403 = CARTESIAN_POINT ( 'NONE',  ( -4.243569643749997233, 14.89062500061451644, -27.54997392385601174 ) ) ;
#39404 = CARTESIAN_POINT ( 'NONE',  ( 14.06250000122903288, -4.330127018922190985, -2.500000000000001332 ) ) ;
#39405 = CARTESIAN_POINT ( 'NONE',  ( 14.47499999999999964, 6.123233995736764310E-16, -4.999999999999998224 ) ) ;
#39406 = LINE ( 'NONE', #44225, #72762 ) ;
#39407 = CARTESIAN_POINT ( 'NONE',  ( 22.37812500061451360, 6.421520780324663323E-16, -5.243569643749999010 ) ) ;
#39408 = CARTESIAN_POINT ( 'NONE',  ( 6.571875000614517681, -6.054752690667223547, -1.112240025338166033E-15 ) ) ;
#39409 = CARTESIAN_POINT ( 'NONE',  ( 8.550000001229031810, -2.886751345948129988, 4.999999999999997335 ) ) ;
#39410 = CARTESIAN_POINT ( 'NONE',  ( 16.31250000122903288, -4.330127018922190985, -2.500000000000001332 ) ) ;
#39411 = CARTESIAN_POINT ( 'NONE',  ( 12.96562500061451750, 3.027376345333613106, -5.243569643749998122 ) ) ;
#39412 = CARTESIAN_POINT ( 'NONE',  ( 17.24062500061451786, -3.027376345333614438, 5.243569643749998122 ) ) ;
#39413 = CARTESIAN_POINT ( 'NONE',  ( 27.63750000122903216, 6.123233995736764310E-16, -4.999999999999998224 ) ) ;
#39414 = CARTESIAN_POINT ( 'NONE',  ( 22.87500000000000000, -4.330127018922194537, 2.499999999999995559 ) ) ;
#39415 = CARTESIAN_POINT ( 'NONE',  ( 24.57187500061451502, -6.054752690667223547, -1.112240025338166033E-15 ) ) ;
#39416 = CARTESIAN_POINT ( 'NONE',  ( 25.76250000122903216, -4.330127018922190985, -2.500000000000001332 ) ) ;
#39417 = CARTESIAN_POINT ( 'NONE',  ( 10.57500000122903572, 2.886751345948129099, -4.999999999999998224 ) ) ;
#39418 = CARTESIAN_POINT ( 'NONE',  ( 28.32187500061451502, 3.027376345333613106, -5.243569643749998122 ) ) ;
#39419 = ADVANCED_FACE ( 'NONE', ( #23058 ), #46696, .T. ) ;
#39420 = CARTESIAN_POINT ( 'NONE',  ( 5.184375000614516615, -4.541064518000419881, 2.621784821874995952 ) ) ;
#39421 = CARTESIAN_POINT ( 'NONE',  ( 22.52812500061451573, 4.541064518000418104, 2.621784821874999949 ) ) ;
#39422 = CARTESIAN_POINT ( 'NONE',  ( -1.878215178125001827, 15.75312499938548427, 33.25316411605952283 ) ) ;
#39423 = CARTESIAN_POINT ( 'NONE',  ( 0.000000000000000000, 20.00000000000000000, -33.99999999999999289 ) ) ;
#39424 = CARTESIAN_POINT ( 'NONE',  ( 10.05937500061451750, 0.000000000000000000, 5.243569643749999010 ) ) ;
#39425 = CARTESIAN_POINT ( 'NONE',  ( 3.999999999999999112, 12.57500000000000107, 30.00000000000000000 ) ) ;
#39426 = CARTESIAN_POINT ( 'NONE',  ( 3.271875000614519635, 3.027376345333611329, 5.243569643749999010 ) ) ;
#39427 = CARTESIAN_POINT ( 'NONE',  ( 6.684375000614518392, 6.421520780324663323E-16, -5.243569643749999010 ) ) ;
#39428 = DIRECTION ( 'NONE',  ( 0.000000000000000000, 0.000000000000000000, -1.000000000000000000 ) ) ;
#39429 = CARTESIAN_POINT ( 'NONE',  ( 27.45937500061451786, 4.541064518000418104, -2.621784821874998173 ) ) ;
#39430 = CARTESIAN_POINT ( 'NONE',  ( 19.79999999999999716, -4.330127018922190985, -2.500000000000001332 ) ) ;
#39431 = VERTEX_POINT ( 'NONE', #45286 ) ;
#39433 = EDGE_CURVE ( 'NONE', #1784, #28145, #11306, .T. ) ;
#39432 = CARTESIAN_POINT ( 'NONE',  ( 26.06250000000000000, -5.773502691896255534, -1.060575238724906372E-15 ) ) ;
#39434 = CARTESIAN_POINT ( 'NONE',  ( 29.74687500061451217, 6.054752690667223547, 3.707466751127219781E-16 ) ) ;
#39435 = ORIENTED_EDGE ( 'NONE', *, *, #71019, .T. ) ;
#39436 = CARTESIAN_POINT ( 'NONE',  ( 15.55312500061451608, -4.541064518000417216, -2.621784821875001281 ) ) ;
#39437 = CARTESIAN_POINT ( 'NONE',  ( 7.153125000614518392, 4.541064518000418104, -2.621784821874998173 ) ) ;
#39438 = CARTESIAN_POINT ( 'NONE',  ( 18.19687500061451502, -4.119189519843965641, -2.378215178125001383 ) ) ;
#39439 = CARTESIAN_POINT ( 'NONE',  ( 4.996875000614516615, 6.054752690667223547, 3.707466751127219781E-16 ) ) ;
#39440 = CARTESIAN_POINT ( 'NONE',  ( 18.18750000122903288, 6.123233995736764310E-16, -4.999999999999998224 ) ) ;
#39441 = CARTESIAN_POINT ( 'NONE',  ( 23.21250000000000213, 2.886751345948126879, 4.999999999999999112 ) ) ;
#39442 = CARTESIAN_POINT ( 'NONE',  ( 24.03750000122903430, 6.123233995736764310E-16, -4.999999999999998224 ) ) ;
#39443 = CARTESIAN_POINT ( 'NONE',  ( 7.284375000614518036, 4.541064518000418104, 2.621784821874999949 ) ) ;
#39444 = CARTESIAN_POINT ( 'NONE',  ( 12.19687500061451679, 6.054752690667223547, 3.707466751127219781E-16 ) ) ;
#39445 = CARTESIAN_POINT ( 'NONE',  ( 21.53437500061451715, 6.421520780324663323E-16, -5.243569643749999010 ) ) ;
#39446 = DIRECTION ( 'NONE',  ( 1.000000000000000000, 0.000000000000000000, 0.000000000000000000 ) ) ;
#39447 = ORIENTED_EDGE ( 'NONE', *, *, #20329, .F. ) ;
#39448 = CARTESIAN_POINT ( 'NONE',  ( 4.134375000614517681, 4.541064518000418104, 2.621784821874999949 ) ) ;
#39449 = CARTESIAN_POINT ( 'NONE',  ( 6.046875000614519102, -3.027376345333614438, 5.243569643749998122 ) ) ;
#39450 = CARTESIAN_POINT ( 'NONE',  ( 18.14999999999999858, 4.330127018922192761, -2.499999999999997780 ) ) ;
#39451 = CARTESIAN_POINT ( 'NONE',  ( 15.92812500061451608, -4.541064518000419881, 2.621784821874995952 ) ) ;
#39452 = CARTESIAN_POINT ( 'NONE',  ( 3.999999999999998668, 18.31250000000000000, 32.30940107675850470 ) ) ;
#39453 = CARTESIAN_POINT ( 'NONE',  ( 4.289383384044220371, 2.569665102604888673, 4.334061492837330221 ) ) ;
#39454 = CARTESIAN_POINT ( 'NONE',  ( 21.72187500061451715, 2.746126346562643317, 4.756430356249998326 ) ) ;
#39455 = CARTESIAN_POINT ( 'NONE',  ( 10.00312500061451715, 0.000000000000000000, 5.243569643749999010 ) ) ;
#39456 = CARTESIAN_POINT ( 'NONE',  ( 27.38437500061451857, 6.421520780324663323E-16, -5.243569643749999010 ) ) ;
#39457 = FACE_OUTER_BOUND ( 'NONE', #71731, .T. ) ;
#39458 = CARTESIAN_POINT ( 'NONE',  ( 29.67187500061451644, 3.027376345333613106, -5.243569643749998122 ) ) ;
#39459 = CARTESIAN_POINT ( 'NONE',  ( 9.000000000000001776, -4.330127018922190985, -2.500000000000001332 ) ) ;
#39460 = CARTESIAN_POINT ( 'NONE',  ( -3.999999999999999112, 14.71250000122903501, 30.00000000000000000 ) ) ;
#39461 = CARTESIAN_POINT ( 'NONE',  ( 10.20000000122903572, 5.773502691896255534, 3.535250795749688894E-16 ) ) ;
#39462 = CARTESIAN_POINT ( 'NONE',  ( 19.84687500061451360, 6.054752690667223547, 3.707466751127219781E-16 ) ) ;
#39463 = CARTESIAN_POINT ( 'NONE',  ( 13.99687500061451928, 6.054752690667223547, 3.707466751127219781E-16 ) ) ;
#39464 = CARTESIAN_POINT ( 'NONE',  ( 17.84999999999999787, 0.000000000000000000, 4.999999999999998224 ) ) ;
#39465 = VERTEX_POINT ( 'NONE', #56370 ) ;
#39466 = CARTESIAN_POINT ( 'NONE',  ( 15.74062500061451608, 6.054752690667223547, 3.707466751127219781E-16 ) ) ;
#39467 = CARTESIAN_POINT ( 'NONE',  ( 27.33750000122903145, 4.330127018922191873, 2.499999999999999556 ) ) ;
#39468 = CARTESIAN_POINT ( 'NONE',  ( 15.00937500061451679, 0.000000000000000000, 5.243569643749999010 ) ) ;
#39469 = CARTESIAN_POINT ( 'NONE',  ( 3.365625000614516082, -6.054752690667223547, -1.112240025338166033E-15 ) ) ;
#39470 = CARTESIAN_POINT ( 'NONE',  ( 16.45312500061451289, -4.541064518000417216, -2.621784821875001281 ) ) ;
#39471 = CARTESIAN_POINT ( 'NONE',  ( 18.30000000000000071, 0.000000000000000000, 4.999999999999998224 ) ) ;
#39472 = CARTESIAN_POINT ( 'NONE',  ( 26.70937500061451431, 0.000000000000000000, 5.243569643749999010 ) ) ;
#39473 = CARTESIAN_POINT ( 'NONE',  ( -4.243569643749999898, 11.21562500061451750, 27.54997392385601529 ) ) ;
#39474 = CARTESIAN_POINT ( 'NONE',  ( 15.27187500061451786, 3.027376345333613106, -5.243569643749998122 ) ) ;
#39475 = CARTESIAN_POINT ( 'NONE',  ( 14.81250000122903288, 0.000000000000000000, 4.999999999999998224 ) ) ;
#39476 = LINE ( 'NONE', #46105, #10334 ) ;
#39477 = CARTESIAN_POINT ( 'NONE',  ( 3.342464638718772196, -3.718602191040201621, 3.696902112923342365 ) ) ;
#39478 = CARTESIAN_POINT ( 'NONE',  ( 18.34687500061451715, -3.027376345333610441, -5.243569643749999898 ) ) ;
#39479 = CARTESIAN_POINT ( 'NONE',  ( 21.18750000122903288, -4.330127018922194537, 2.499999999999995559 ) ) ;
#39480 = VECTOR ( 'NONE', #34886, 1000.000000000000000 ) ;
#39481 = CARTESIAN_POINT ( 'NONE',  ( 14.33437500061451786, 6.421520780324663323E-16, -5.243569643749999010 ) ) ;
#39482 = CARTESIAN_POINT ( 'NONE',  ( 2.121784821874999061, 13.40937500061451892, 26.32496088578401583 ) ) ;
#39483 = CARTESIAN_POINT ( 'NONE',  ( 21.60000000122903430, -2.886751345948129988, 4.999999999999997335 ) ) ;
#39484 = CARTESIAN_POINT ( 'NONE',  ( 15.25312500061451715, 4.541064518000418104, -2.621784821874998173 ) ) ;
#39485 = ORIENTED_EDGE ( 'NONE', *, *, #35222, .T. ) ;
#39486 = VERTEX_POINT ( 'NONE', #10209 ) ;
#39487 = VECTOR ( 'NONE', #30956, 1000.000000000000000 ) ;
#39488 = CARTESIAN_POINT ( 'NONE',  ( 20.77500000000000213, 6.123233995736764310E-16, -4.999999999999998224 ) ) ;
#39489 = CARTESIAN_POINT ( 'NONE',  ( -1.071796769724492338, 17.95490381179670081, 34.00000000000000000 ) ) ;
#39490 = CARTESIAN_POINT ( 'NONE',  ( 21.14062500061451289, 6.054752690667223547, 3.707466751127219781E-16 ) ) ;
#39491 = CARTESIAN_POINT ( 'NONE',  ( 3.942105046096219478, 3.076001935233271922, 29.30868670468199255 ) ) ;
#39492 = CARTESIAN_POINT ( 'NONE',  ( 13.91250000122903252, 0.000000000000000000, 4.999999999999998224 ) ) ;
#39493 = CARTESIAN_POINT ( 'NONE',  ( 19.00312500061451715, 0.000000000000000000, 5.243569643749999010 ) ) ;
#39494 = CARTESIAN_POINT ( 'NONE',  ( 24.32812500061451289, 4.541064518000418104, 2.621784821874999949 ) ) ;
#39495 = CARTESIAN_POINT ( 'NONE',  ( 5.578125000614518214, -4.541064518000419881, 2.621784821874995952 ) ) ;
#39496 = ORIENTED_EDGE ( 'NONE', *, *, #69860, .T. ) ;
#39497 = CARTESIAN_POINT ( 'NONE',  ( 29.39999999999999858, 4.330127018922192761, -2.499999999999997780 ) ) ;
#39498 = CARTESIAN_POINT ( 'NONE',  ( 17.39999999999999858, 0.000000000000000000, 4.999999999999998224 ) ) ;
#39499 = CARTESIAN_POINT ( 'NONE',  ( 9.046875000614518214, 5.492252693125287522, 3.363034840372157021E-16 ) ) ;
#39500 = DIRECTION ( 'NONE',  ( 0.000000000000000000, 0.000000000000000000, 1.000000000000000000 ) ) ;
#39501 = CARTESIAN_POINT ( 'NONE',  ( 8.484601909799253346E-16, 11.67500000122903359, -25.38119784648299770 ) ) ;
#39502 = CARTESIAN_POINT ( 'NONE',  ( 4.243569643749999010, 17.42187500061451999, -32.45002607614398471 ) ) ;
#39503 = CARTESIAN_POINT ( 'NONE',  ( 6.862500001229034474, -4.330127018922190985, -2.500000000000001332 ) ) ;
#39504 = CARTESIAN_POINT ( 'NONE',  ( 7.200000000000001954, -4.330127018922190985, -2.500000000000001332 ) ) ;
#39505 = ADVANCED_FACE ( 'NONE', ( #6117 ), #27572, .F. ) ;
#39506 = CARTESIAN_POINT ( 'NONE',  ( 3.712500001229034563, -4.330127018922190985, -2.500000000000001332 ) ) ;
#39507 = CARTESIAN_POINT ( 'NONE',  ( 11.37187500061451750, 3.027376345333611329, 5.243569643749999010 ) ) ;
#39508 = DIRECTION ( 'NONE',  ( -1.000000000000000000, -0.000000000000000000, -0.000000000000000000 ) ) ;
#39509 = CARTESIAN_POINT ( 'NONE',  ( 3.684375000614518836, 4.541064518000418104, 2.621784821874999949 ) ) ;
#39510 = CYLINDRICAL_SURFACE ( 'NONE', #9030, 3.999999999999996447 ) ;
#39511 = CARTESIAN_POINT ( 'NONE',  ( 12.50625000122903430, 0.000000000000000000, 4.999999999999998224 ) ) ;
#39512 = CARTESIAN_POINT ( 'NONE',  ( 10.43437500061451750, 4.541064518000418104, 2.621784821874999949 ) ) ;
#39513 = CARTESIAN_POINT ( 'NONE',  ( -3.999999999999997335, 18.68750000000000000, -27.69059892324149530 ) ) ;
#39514 = CARTESIAN_POINT ( 'NONE',  ( 3.999999999999998668, 14.41250000000000142, 27.69059892324149530 ) ) ;
#39515 = CIRCLE ( 'NONE', #31289, 9.000000000000000000 ) ;
#39516 = CARTESIAN_POINT ( 'NONE',  ( 4.243569643749999010, 16.91562500061459673, 27.54997392385601174 ) ) ;
#39517 = CARTESIAN_POINT ( 'NONE',  ( 22.24687500061451217, -3.027376345333614438, 5.243569643749998122 ) ) ;
#39518 =( NAMED_UNIT ( * ) SI_UNIT ( $, .STERADIAN. ) SOLID_ANGLE_UNIT ( ) );
#39519 = CARTESIAN_POINT ( 'NONE',  ( 29.10000000122903074, 5.773502691896255534, 3.535250795749688894E-16 ) ) ;
#39520 = VECTOR ( 'NONE', #51480, 1000.000000000000000 ) ;
#39521 = CARTESIAN_POINT ( 'NONE',  ( 18.75937500061451857, 2.746126346562645981, -4.756430356249997438 ) ) ;
#39522 = CARTESIAN_POINT ( 'NONE',  ( 22.60312500061451857, 0.000000000000000000, 5.243569643749999010 ) ) ;
#39523 = CARTESIAN_POINT ( 'NONE',  ( 16.19062500061451715, 6.054752690667223547, 3.707466751127219781E-16 ) ) ;
#39524 = CARTESIAN_POINT ( 'NONE',  ( 15.28125000122903288, -4.330127018922194537, 2.499999999999995559 ) ) ;
#39525 = CARTESIAN_POINT ( 'NONE',  ( 10.69687500061451679, -3.027376345333610441, -5.243569643749999898 ) ) ;
#39526 = CARTESIAN_POINT ( 'NONE',  ( 29.25000000000000000, -4.330127018922190985, -2.500000000000001332 ) ) ;
#39527 = CARTESIAN_POINT ( 'NONE',  ( 25.76250000122903216, -4.330127018922190985, -2.500000000000001332 ) ) ;
#39528 = CARTESIAN_POINT ( 'NONE',  ( 4.059375000614519280, 4.541064518000418104, -2.621784821874998173 ) ) ;
#39529 = AXIS2_PLACEMENT_3D ( 'NONE', #16105, #61535, #33827 ) ;
#39530 = CARTESIAN_POINT ( 'NONE',  ( 13.80937500061451750, -4.541064518000417216, -2.621784821875001281 ) ) ;
#39531 = CARTESIAN_POINT ( 'NONE',  ( 28.99687500061451573, -3.027376345333614438, 5.243569643749998122 ) ) ;
#39532 = FACE_OUTER_BOUND ( 'NONE', #7172, .T. ) ;
#39533 = CARTESIAN_POINT ( 'NONE',  ( 18.41249999999999787, -5.773502691896255534, -1.060575238724906372E-15 ) ) ;
#39534 = CARTESIAN_POINT ( 'NONE',  ( 22.99687500061451573, 6.054752690667223547, 3.707466751127219781E-16 ) ) ;
#39535 = CARTESIAN_POINT ( 'NONE',  ( 14.78437500061451715, 6.421520780324663323E-16, -5.243569643749999010 ) ) ;
#39536 = CARTESIAN_POINT ( 'NONE',  ( -7.967954043666661671E-16, 17.14062499938548356, 34.33755215474603517 ) ) ;
#39537 = CARTESIAN_POINT ( 'NONE',  ( 28.76249999999999929, -5.773502691896255534, -1.060575238724906372E-15 ) ) ;
#39538 = CARTESIAN_POINT ( 'NONE',  ( 4.425000001229032698, 2.886751345948126879, 4.999999999999999112 ) ) ;
#39539 = CARTESIAN_POINT ( 'NONE',  ( 29.22187500061451715, 2.746126346562645981, -4.756430356249997438 ) ) ;
#39540 = CARTESIAN_POINT ( 'NONE',  ( 16.60312500061451857, 4.541064518000418104, -2.621784821874998173 ) ) ;
#39541 = CARTESIAN_POINT ( 'NONE',  ( 7.237500000000000711, -2.886751345948125991, -5.000000000000000000 ) ) ;
#39542 =( BOUNDED_CURVE ( )  B_SPLINE_CURVE ( 2, ( #61182, #55284, #60805, #5400, #50470, #44575, #71545 ),
 .UNSPECIFIED., .F., .F. ) 
 B_SPLINE_CURVE_WITH_KNOTS ( ( 3, 2, 2, 3 ),
 ( 0.8166666666666666519, 0.8194444444444444198, 0.8222222222222222987, 0.8250000000000000666 ),
 .UNSPECIFIED. ) 
 CURVE ( )  GEOMETRIC_REPRESENTATION_ITEM ( )  RATIONAL_B_SPLINE_CURVE ( ( 1.000000000000000000, 0.8660254037844387076, 1.000000000000000000, 0.8660254037844387076, 1.000000000000000000, 0.8660254037844333785, 1.000000000000005329 ) ) 
 REPRESENTATION_ITEM ( '' )  );
#39543 = CARTESIAN_POINT ( 'NONE',  ( 17.17500000000000071, 6.123233995736764310E-16, -4.999999999999998224 ) ) ;
#39544 = CARTESIAN_POINT ( 'NONE',  ( 18.30000000000000071, 0.000000000000000000, 4.999999999999998224 ) ) ;
#39545 = CARTESIAN_POINT ( 'NONE',  ( 2.121784821874999061, 12.00312500061451715, 26.32496088578401583 ) ) ;
#39546 = CARTESIAN_POINT ( 'NONE',  ( 24.80625000122903145, -4.330127018922190985, -2.500000000000001332 ) ) ;
#39547 = CARTESIAN_POINT ( 'NONE',  ( 20.51250000122903216, 4.330127018922192761, -2.499999999999997780 ) ) ;
#39548 = CARTESIAN_POINT ( 'NONE',  ( -3.999999999999999112, 13.32500000122903216, 27.69059892324149885 ) ) ;
#39549 = CARTESIAN_POINT ( 'NONE',  ( 27.04687500061451644, 6.054752690667223547, 3.707466751127219781E-16 ) ) ;
#39550 = VERTEX_POINT ( 'NONE', #5761 ) ;
#39551 = CARTESIAN_POINT ( 'NONE',  ( 21.66562500061451502, 3.027376345333611329, 5.243569643749999010 ) ) ;
#39552 = CARTESIAN_POINT ( 'NONE',  ( 22.32187500061451502, -6.054752690667223547, -1.112240025338166033E-15 ) ) ;
#39553 = CARTESIAN_POINT ( 'NONE',  ( 5.887500000000000178, -2.886751345948125991, -5.000000000000000000 ) ) ;
#39554 = CARTESIAN_POINT ( 'NONE',  ( 10.49062500061451431, -3.027376345333614438, 5.243569643749998122 ) ) ;
#39555 = CARTESIAN_POINT ( 'NONE',  ( 23.61562500061451431, -6.054752690667223547, -1.112240025338166033E-15 ) ) ;
#39556 = CARTESIAN_POINT ( 'NONE',  ( 14.18437500061451750, -4.541064518000419881, 2.621784821874995952 ) ) ;
#39557 = CARTESIAN_POINT ( 'NONE',  ( 17.10937500061451999, 4.541064518000418104, -2.621784821874998173 ) ) ;
#39558 = CARTESIAN_POINT ( 'NONE',  ( 4.442357930815816758, 2.294658147637304690, -4.714824131856698131 ) ) ;
#39559 = CARTESIAN_POINT ( 'NONE',  ( 9.001249775931846008E-16, 18.11562500061451786, 34.90005215228797653 ) ) ;
#39560 = CARTESIAN_POINT ( 'NONE',  ( 22.12500000122903288, -5.773502691896255534, -1.060575238724906372E-15 ) ) ;
#39561 = CARTESIAN_POINT ( 'NONE',  ( 15.15937500061451715, -4.119189519843965641, -2.378215178125001383 ) ) ;
#39562 = CARTESIAN_POINT ( 'NONE',  ( 12.92812500061451786, 6.421520780324663323E-16, -5.243569643749999010 ) ) ;
#39563 = CARTESIAN_POINT ( 'NONE',  ( 5.296875000614518214, -3.027376345333610441, -5.243569643749999898 ) ) ;
#39564 = CARTESIAN_POINT ( 'NONE',  ( 4.696875000614518569, -3.027376345333614438, 5.243569643749998122 ) ) ;
#39565 = ORIENTED_EDGE ( 'NONE', *, *, #65890, .F. ) ;
#39566 = CARTESIAN_POINT ( 'NONE',  ( 28.95937500061451431, 0.000000000000000000, 5.243569643749999010 ) ) ;
#39567 = CARTESIAN_POINT ( 'NONE',  ( 17.39062500061451644, -3.027376345333610441, -5.243569643749999898 ) ) ;
#39568 = CARTESIAN_POINT ( 'NONE',  ( 28.31250000122903288, 0.000000000000000000, 4.999999999999998224 ) ) ;
#39569 = ADVANCED_FACE ( 'NONE', ( #27206 ), #49741, .F. ) ;
#39570 = CARTESIAN_POINT ( 'NONE',  ( 28.22812500061451502, 6.421520780324663323E-16, -5.243569643749999010 ) ) ;
#39571 = CARTESIAN_POINT ( 'NONE',  ( 21.00937500061451857, -4.541064518000417216, -2.621784821875001281 ) ) ;
#39572 = CARTESIAN_POINT ( 'NONE',  ( 18.21562500061451573, -6.054752690667223547, -1.112240025338166033E-15 ) ) ;
#39573 = CARTESIAN_POINT ( 'NONE',  ( 2.121784821874999061, 19.25937500061451857, 26.32496088578401583 ) ) ;
#39574 = AXIS2_PLACEMENT_3D ( 'NONE', #64066, #8290, #64434 ) ;
#39575 = CARTESIAN_POINT ( 'NONE',  ( 23.87812500061451715, 4.541064518000418104, 2.621784821874999949 ) ) ;
#39576 = CARTESIAN_POINT ( 'NONE',  ( 4.012500001229033053, 0.000000000000000000, 4.999999999999998224 ) ) ;
#39577 = ORIENTED_EDGE ( 'NONE', *, *, #65470, .F. ) ;
#39578 = CARTESIAN_POINT ( 'NONE',  ( 27.78749999999999787, -2.886751345948129988, 4.999999999999997335 ) ) ;
#39579 = CARTESIAN_POINT ( 'NONE',  ( 4.000000000000000000, 13.43750000000000000, -27.69059892324149530 ) ) ;
#39580 = CARTESIAN_POINT ( 'NONE',  ( 1.878215178125000495, 16.87812499938548072, 26.74683588394047007 ) ) ;
#39581 = CARTESIAN_POINT ( 'NONE',  ( 4.096875000614518925, 6.054752690667223547, 3.707466751127219781E-16 ) ) ;
#39582 = CARTESIAN_POINT ( 'NONE',  ( 11.16562500061451679, 3.027376345333613106, -5.243569643749998122 ) ) ;
#39583 = CARTESIAN_POINT ( 'NONE',  ( 25.72500000122903074, -5.773502691896255534, -1.060575238724906372E-15 ) ) ;
#39584 = CARTESIAN_POINT ( 'NONE',  ( 12.75937500061451857, 0.000000000000000000, 5.243569643749999010 ) ) ;
#39585 = CARTESIAN_POINT ( 'NONE',  ( 29.09062500061451573, -3.027376345333610441, -5.243569643749999898 ) ) ;
#39586 = CARTESIAN_POINT ( 'NONE',  ( 28.83749999999999858, -2.886751345948125991, -5.000000000000000000 ) ) ;
#39587 = CARTESIAN_POINT ( 'NONE',  ( 14.77500000122903501, 2.886751345948126879, 4.999999999999998224 ) ) ;
#39588 = CARTESIAN_POINT ( 'NONE',  ( 12.47812500061451502, 6.421520780324663323E-16, -5.243569643749999010 ) ) ;
#39589 = ORIENTED_EDGE ( 'NONE', *, *, #7572, .F. ) ;
#39590 = VECTOR ( 'NONE', #1466, 1000.000000000000000 ) ;
#39591 = CARTESIAN_POINT ( 'NONE',  ( 10.30312500061451431, 4.541064518000418104, -2.621784821874998173 ) ) ;
#39592 = CARTESIAN_POINT ( 'NONE',  ( 7.153125000614518392, 4.541064518000418104, -2.621784821874998173 ) ) ;
#39593 = CARTESIAN_POINT ( 'NONE',  ( 19.05937500061451928, 0.000000000000000000, 4.756430356249998326 ) ) ;
#39594 = EDGE_CURVE ( 'NONE', #57985, #19407, #26414, .T. ) ;
#39595 = CARTESIAN_POINT ( 'NONE',  ( 14.06250000122903288, -4.330127018922190985, -2.500000000000001332 ) ) ;
#39596 =( BOUNDED_CURVE ( )  B_SPLINE_CURVE ( 2, ( #15231, #39241, #49959, #50331, #22237, #26701, #72855 ),
 .UNSPECIFIED., .F., .F. ) 
 B_SPLINE_CURVE_WITH_KNOTS ( ( 3, 2, 2, 3 ),
 ( 0.3699999999999999956, 0.3733333333333333504, 0.3766666666666666496, 0.3800000000000000044 ),
 .UNSPECIFIED. ) 
 CURVE ( )  GEOMETRIC_REPRESENTATION_ITEM ( )  RATIONAL_B_SPLINE_CURVE ( ( 1.000000000000000000, 0.8660254037844387076, 1.000000000000000000, 0.8660254037844387076, 1.000000000000000000, 0.8660254037844387076, 1.000000000000000000 ) ) 
 REPRESENTATION_ITEM ( '' )  );
#39597 = CARTESIAN_POINT ( 'NONE',  ( 16.72500000000000142, 6.123233995736764310E-16, -4.999999999999998224 ) ) ;
#39598 =( BOUNDED_CURVE ( )  B_SPLINE_CURVE ( 2, ( #28613, #550, #16790, #23061, #45616, #68149, #51516 ),
 .UNSPECIFIED., .F., .F. ) 
 B_SPLINE_CURVE_WITH_KNOTS ( ( 3, 2, 2, 3 ),
 ( 0.3333333333333333703, 0.3361111111111111382, 0.3388888888888889062, 0.3416666666666666186 ),
 .UNSPECIFIED. ) 
 CURVE ( )  GEOMETRIC_REPRESENTATION_ITEM ( )  RATIONAL_B_SPLINE_CURVE ( ( 0.9999999999999973355, 0.8660254037844413721, 1.000000000000000000, 0.8660254037844387076, 1.000000000000000000, 0.8660254037844413721, 0.9999999999999973355 ) ) 
 REPRESENTATION_ITEM ( '' )  );
#39599 = CARTESIAN_POINT ( 'NONE',  ( 16.39687500061451786, -3.027376345333614438, 5.243569643749998122 ) ) ;
#39600 = CARTESIAN_POINT ( 'NONE',  ( 12.15000000122903501, -2.886751345948129988, 4.999999999999997335 ) ) ;
#39601 = CARTESIAN_POINT ( 'NONE',  ( 19.02187500061451786, 3.027376345333611329, 5.243569643749999010 ) ) ;
#39602 = CARTESIAN_POINT ( 'NONE',  ( 18.78749999999999432, -2.886751345948129988, 4.999999999999997335 ) ) ;
#39603 = CARTESIAN_POINT ( 'NONE',  ( 20.97187500061451715, -6.054752690667223547, -1.112240025338166033E-15 ) ) ;
#39604 = CARTESIAN_POINT ( 'NONE',  ( -4.243569643749999898, 13.46562500061451928, -32.45002607614398471 ) ) ;
#39605 = CARTESIAN_POINT ( 'NONE',  ( -3.999999999999999112, 19.66250000122903430, 30.00000000000000000 ) ) ;
#39606 = CARTESIAN_POINT ( 'NONE',  ( 25.73437500061451644, -2.746126346562646425, 4.756430356249996549 ) ) ;
#39607 = FACE_OUTER_BOUND ( 'NONE', #28208, .T. ) ;
#39608 = CARTESIAN_POINT ( 'NONE',  ( 28.04062500061451502, -3.027376345333614438, 5.243569643749998122 ) ) ;
#39609 = CYLINDRICAL_SURFACE ( 'NONE', #18593, 9.000000000000000000 ) ;
#39610 = CARTESIAN_POINT ( 'NONE',  ( 17.51249999999999929, -5.773502691896255534, -1.060575238724906372E-15 ) ) ;
#39611 = EDGE_CURVE ( 'NONE', #65915, #50879, #27935, .T. ) ;
#39612 = CARTESIAN_POINT ( 'NONE',  ( 24.63749999999999574, -2.886751345948129988, 4.999999999999997335 ) ) ;
#39613 =( BOUNDED_CURVE ( )  B_SPLINE_CURVE ( 2, ( #37150, #9083, #48245, #3550, #42336, #31620, #3918 ),
 .UNSPECIFIED., .F., .F. ) 
 B_SPLINE_CURVE_WITH_KNOTS ( ( 3, 2, 2, 3 ),
 ( 0.8100000000000000533, 0.8133333333333333526, 0.8166666666666667629, 0.8200000000000000622 ),
 .UNSPECIFIED. ) 
 CURVE ( )  GEOMETRIC_REPRESENTATION_ITEM ( )  RATIONAL_B_SPLINE_CURVE ( ( 1.000000000000000000, 0.8660254037844387076, 1.000000000000000000, 0.8660254037844387076, 1.000000000000000000, 0.8660254037844342667, 1.000000000000004441 ) ) 
 REPRESENTATION_ITEM ( '' )  );
#39614 = CARTESIAN_POINT ( 'NONE',  ( 8.203125000614518214, 0.000000000000000000, 5.243569643749999010 ) ) ;
#39615 = CARTESIAN_POINT ( 'NONE',  ( 27.38437500061451502, 5.492252693125287522, 3.363034840372157021E-16 ) ) ;
#39616 = CARTESIAN_POINT ( 'NONE',  ( 20.10937500061451289, -4.541064518000417216, -2.621784821875001281 ) ) ;
#39617 = CARTESIAN_POINT ( 'NONE',  ( 10.62187500061451395, 5.824947211148865298E-16, -4.756430356249998326 ) ) ;
#39618 = VECTOR ( 'NONE', #10289, 1000.000000000000000 ) ;
#39619 = CARTESIAN_POINT ( 'NONE',  ( 6.365625000614518747, 3.027376345333611329, 5.243569643749999010 ) ) ;
#39620 = CARTESIAN_POINT ( 'NONE',  ( 9.871875000614517504, 3.027376345333613106, -5.243569643749998122 ) ) ;
#39621 = ORIENTED_EDGE ( 'NONE', *, *, #33444, .F. ) ;
#39622 = CARTESIAN_POINT ( 'NONE',  ( 20.48437500061451289, -4.541064518000419881, 2.621784821874995952 ) ) ;
#39623 = CARTESIAN_POINT ( 'NONE',  ( 16.50000000000000000, 0.000000000000000000, 4.999999999999998224 ) ) ;
#39624 = LINE ( 'NONE', #51061, #11325 ) ;
#39625 = CARTESIAN_POINT ( 'NONE',  ( 4.912499999999999645, -5.773502691896255534, -1.060575238724906372E-15 ) ) ;
#39626 = CARTESIAN_POINT ( 'NONE',  ( 15.15000000122903323, 5.773502691896255534, 3.535250795749688894E-16 ) ) ;
#39627 = DIRECTION ( 'NONE',  ( -1.000000000000000000, -0.000000000000000000, -0.000000000000000000 ) ) ;
#39628 = CARTESIAN_POINT ( 'NONE',  ( -3.999999999999999112, 19.09999999999999787, -30.00000000000000000 ) ) ;
#39629 = ORIENTED_EDGE ( 'NONE', *, *, #56668, .F. ) ;
#39630 = CARTESIAN_POINT ( 'NONE',  ( 12.56250000000000178, -5.773502691896255534, -1.060575238724906372E-15 ) ) ;
#39631 = CARTESIAN_POINT ( 'NONE',  ( 24.92812500061451431, -4.541064518000419881, 2.621784821874995952 ) ) ;
#39632 = CARTESIAN_POINT ( 'NONE',  ( 16.05000000000000071, 0.000000000000000000, 4.999999999999998224 ) ) ;
#39633 = CARTESIAN_POINT ( 'NONE',  ( 11.55000000122903181, 5.773502691896255534, 3.535250795749688894E-16 ) ) ;
#39634 = CARTESIAN_POINT ( 'NONE',  ( 8.653125000614515727, 0.000000000000000000, 5.243569643749999010 ) ) ;
#39635 = VECTOR ( 'NONE', #42100, 1000.000000000000000 ) ;
#39636 = CARTESIAN_POINT ( 'NONE',  ( 8.662499999999999645, 2.886751345948129099, -4.999999999999998224 ) ) ;
#39637 = DIRECTION ( 'NONE',  ( 0.000000000000000000, 0.000000000000000000, 1.000000000000000000 ) ) ;
#39638 = CARTESIAN_POINT ( 'NONE',  ( -2.121784821874999949, 13.93437500061451750, -33.67503911421598417 ) ) ;
#39639 = CARTESIAN_POINT ( 'NONE',  ( 26.88750000122903216, 4.330127018922191873, 2.499999999999999556 ) ) ;
#39640 = CARTESIAN_POINT ( 'NONE',  ( -1.878215178124999163, 14.14062499938548356, 26.74683588394047007 ) ) ;
#39641 = CARTESIAN_POINT ( 'NONE',  ( 6.899999999999999467, 4.330127018922192761, -2.499999999999997780 ) ) ;
#39642 = CARTESIAN_POINT ( 'NONE',  ( -1.071796769724475906, 13.15759618943233100, -34.00000000000000711 ) ) ;
#39643 = VERTEX_POINT ( 'NONE', #72268 ) ;
#39644 = CARTESIAN_POINT ( 'NONE',  ( 22.37812500061451360, 6.421520780324663323E-16, -5.243569643749999010 ) ) ;
#39645 = CARTESIAN_POINT ( 'NONE',  ( 12.90000000122903145, 5.773502691896255534, 3.535250795749688894E-16 ) ) ;
#39646 = CARTESIAN_POINT ( 'NONE',  ( 29.24062500061451431, 6.054752690667223547, 3.707466751127219781E-16 ) ) ;
#39647 = CARTESIAN_POINT ( 'NONE',  ( 28.80937500061451573, 4.541064518000418104, -2.621784821874998173 ) ) ;
#39648 = CARTESIAN_POINT ( 'NONE',  ( 18.60937500061451644, 0.000000000000000000, 5.243569643749999010 ) ) ;
#39649 = CARTESIAN_POINT ( 'NONE',  ( 16.86562500061451786, -6.054752690667223547, -1.112240025338166033E-15 ) ) ;
#39650 = CARTESIAN_POINT ( 'NONE',  ( -4.243569643749999898, 12.60312500061459318, -30.00000000000000000 ) ) ;
#39651 = CARTESIAN_POINT ( 'NONE',  ( 7.528125000614515727, 6.421520780324663323E-16, -5.243569643749999010 ) ) ;
#39652 = CARTESIAN_POINT ( 'NONE',  ( 27.75000000122903288, 5.773502691896255534, 3.535250795749688894E-16 ) ) ;
#39653 = CARTESIAN_POINT ( 'NONE',  ( 21.68437500061451573, 4.119189519843966529, 2.378215178124999607 ) ) ;
#39654 = CARTESIAN_POINT ( 'NONE',  ( 19.97812500061451502, -4.541064518000419881, 2.621784821874995952 ) ) ;
#39655 = DIRECTION ( 'NONE',  ( 0.000000000000000000, 0.000000000000000000, -1.000000000000000000 ) ) ;
#39656 = CARTESIAN_POINT ( 'NONE',  ( 3.450000001229036162, 5.773502691896255534, 3.535250795749688894E-16 ) ) ;
#39657 = CARTESIAN_POINT ( 'NONE',  ( 12.90937500061451537, -4.541064518000417216, -2.621784821875001281 ) ) ;
#39658 = CARTESIAN_POINT ( 'NONE',  ( 11.59687500061451892, -3.027376345333610441, -5.243569643749999898 ) ) ;
#39659 = CARTESIAN_POINT ( 'NONE',  ( 21.04687500061451644, -3.027376345333610441, -5.243569643749999898 ) ) ;
#39660 = ORIENTED_EDGE ( 'NONE', *, *, #5302, .T. ) ;
#39661 = FACE_OUTER_BOUND ( 'NONE', #4134, .T. ) ;
#39662 = CARTESIAN_POINT ( 'NONE',  ( 26.91562500061451146, 3.027376345333613106, -5.243569643749998122 ) ) ;
#39663 = CARTESIAN_POINT ( 'NONE',  ( 23.95312500061451289, 0.000000000000000000, 5.243569643749999010 ) ) ;
#39664 = CARTESIAN_POINT ( 'NONE',  ( -1.999999999999999112, 17.09374999877096712, 26.53589838486224650 ) ) ;
#39665 = CARTESIAN_POINT ( 'NONE',  ( 4.000000000000000000, 17.93750000000000355, 32.30940107675849049 ) ) ;
#39666 = CARTESIAN_POINT ( 'NONE',  ( 3.796875000614517326, -3.027376345333614438, 5.243569643749998122 ) ) ;
#39667 = CARTESIAN_POINT ( 'NONE',  ( 12.97500000122903252, 2.886751345948126879, 4.999999999999999112 ) ) ;
#39668 = CARTESIAN_POINT ( 'NONE',  ( 7.650000001229034119, -2.886751345948129988, 4.999999999999997335 ) ) ;
#39669 = CARTESIAN_POINT ( 'NONE',  ( 21.60000000122903074, -2.886751345948130876, 4.999999999999996447 ) ) ;
#39670 = CARTESIAN_POINT ( 'NONE',  ( 26.32500000122903216, 2.886751345948129099, -4.999999999999998224 ) ) ;
#39671 = CARTESIAN_POINT ( 'NONE',  ( 4.000000000000000000, 17.39374999877096428, 30.00000000000000000 ) ) ;
#39672 = CARTESIAN_POINT ( 'NONE',  ( 15.54375000122903394, 5.773502691896255534, 3.535250795749688894E-16 ) ) ;
#39673 = CARTESIAN_POINT ( 'NONE',  ( 10.88437500061451679, 4.541064518000418104, 2.621784821874999949 ) ) ;
#39674 = CYLINDRICAL_SURFACE ( 'NONE', #8971, 4.000000000000000000 ) ;
#39675 = CARTESIAN_POINT ( 'NONE',  ( 16.60312500061451857, 4.541064518000418104, -2.621784821874998173 ) ) ;
#39676 = CARTESIAN_POINT ( 'NONE',  ( 14.52187500061451608, 3.027376345333611329, 5.243569643749999010 ) ) ;
#39677 = CARTESIAN_POINT ( 'NONE',  ( 4.565625000614516260, 3.027376345333611329, 5.243569643749999010 ) ) ;
#39678 = CARTESIAN_POINT ( 'NONE',  ( 22.02187500061451786, 3.027376345333612662, -5.243569643749998122 ) ) ;
#39679 = CARTESIAN_POINT ( 'NONE',  ( 9.796875000614519990, -3.027376345333610441, -5.243569643749999898 ) ) ;
#39680 = CARTESIAN_POINT ( 'NONE',  ( 4.865625000614517859, 3.027376345333613106, -5.243569643749998122 ) ) ;
#39681 = CARTESIAN_POINT ( 'NONE',  ( 45.00000000000000000, 0.000000000000000000, 4.999999999999998224 ) ) ;
#39683 = EDGE_CURVE ( 'NONE', #34387, #17794, #33956, .T. ) ;
#39682 = CARTESIAN_POINT ( 'NONE',  ( 5.812500001229035540, 0.000000000000000000, 4.999999999999998224 ) ) ;
#39684 = CARTESIAN_POINT ( 'NONE',  ( 20.05312500061451431, -4.541064518000417216, -2.621784821875001281 ) ) ;
#39685 = CARTESIAN_POINT ( 'NONE',  ( 7.050000001229036251, 5.773502691896255534, 3.535250795749688894E-16 ) ) ;
#39686 = CARTESIAN_POINT ( 'NONE',  ( 17.87812500061451715, 6.421520780324663323E-16, -5.243569643749999010 ) ) ;
#39687 = AXIS2_PLACEMENT_3D ( 'NONE', #26142, #66774, #49413 ) ;
#39688 = CARTESIAN_POINT ( 'NONE',  ( 12.47812500061451502, 6.421520780324663323E-16, -5.243569643749999010 ) ) ;
#39689 = CARTESIAN_POINT ( 'NONE',  ( 26.78437500061451360, -4.119189519843968306, 2.378215178124996054 ) ) ;
#39690 = CARTESIAN_POINT ( 'NONE',  ( 14.10000000000000142, 4.330127018922192761, -2.499999999999997780 ) ) ;
#39691 = CARTESIAN_POINT ( 'NONE',  ( 9.150000001229033231, -2.886751345948125991, -5.000000000000000000 ) ) ;
#39692 = CARTESIAN_POINT ( 'NONE',  ( 5.015625000614518214, 3.027376345333611329, 5.243569643749999010 ) ) ;
#39693 = CARTESIAN_POINT ( 'NONE',  ( 18.30000000122903359, 5.773502691896255534, 3.535250795749688894E-16 ) ) ;
#39694 = CARTESIAN_POINT ( 'NONE',  ( 26.09999999999999787, -4.330127018922190985, -2.500000000000001332 ) ) ;
#39695 = CARTESIAN_POINT ( 'NONE',  ( -2.121784821874996840, 10.48437500061451821, -26.32496088578401583 ) ) ;
#39696 = DIRECTION ( 'NONE',  ( 0.000000000000000000, 0.000000000000000000, 1.000000000000000000 ) ) ;
#39697 = CARTESIAN_POINT ( 'NONE',  ( 24.14999999999999858, 0.000000000000000000, 4.999999999999998224 ) ) ;
#39698 = EDGE_CURVE ( 'NONE', #48564, #29785, #49083, .T. ) ;
#39699 = DIRECTION ( 'NONE',  ( -1.000000000000000000, 0.000000000000000000, 0.000000000000000000 ) ) ;
#39700 = CARTESIAN_POINT ( 'NONE',  ( 20.25937500061451857, 4.541064518000418104, -2.621784821874998173 ) ) ;
#39701 = CARTESIAN_POINT ( 'NONE',  ( 10.57500000122903039, 2.886751345948062486, -5.000000000000113687 ) ) ;
#39702 = CARTESIAN_POINT ( 'NONE',  ( 16.22812500061451857, 4.541064518000418104, 2.621784821874999949 ) ) ;
#39703 = CARTESIAN_POINT ( 'NONE',  ( 12.13125000122903430, -4.330127018922194537, 2.499999999999995559 ) ) ;
#39704 = CARTESIAN_POINT ( 'NONE',  ( -1.999999999999997113, 14.78750000122903252, 33.46410161513775705 ) ) ;
#39705 = CARTESIAN_POINT ( 'NONE',  ( 10.42500000000000071, 6.123233995736764310E-16, -4.999999999999998224 ) ) ;
#39706 = CARTESIAN_POINT ( 'NONE',  ( 26.03437500061451715, 6.421520780324663323E-16, -5.243569643749999010 ) ) ;
#39707 = CARTESIAN_POINT ( 'NONE',  ( 19.17187500061451289, 5.824947211148865298E-16, -4.756430356249998326 ) ) ;
#39708 = CARTESIAN_POINT ( 'NONE',  ( 11.35312500061451679, 0.000000000000000000, 5.243569643749999010 ) ) ;
#39709 = CARTESIAN_POINT ( 'NONE',  ( 10.69687500061451679, -3.027376345333610441, -5.243569643749999898 ) ) ;
#39710 = ORIENTED_EDGE ( 'NONE', *, *, #1892, .T. ) ;
#39711 = CARTESIAN_POINT ( 'NONE',  ( 2.843225714139721028, -4.112946153745474120, -2.917534517181566756 ) ) ;
#39712 = CARTESIAN_POINT ( 'NONE',  ( 20.80312500061451431, 0.000000000000000000, 5.243569643749999010 ) ) ;
#39713 = DIRECTION ( 'NONE',  ( 0.000000000000000000, 0.000000000000000000, 1.000000000000000000 ) ) ;
#39714 = CARTESIAN_POINT ( 'NONE',  ( -2.000000000000000000, 12.83750000122903501, 26.53589838486224650 ) ) ;
#39715 = EDGE_CURVE ( 'NONE', #45665, #66820, #44929, .T. ) ;
#39716 = CARTESIAN_POINT ( 'NONE',  ( 11.17500000000000071, -4.330127018922194537, 2.499999999999995559 ) ) ;
#39717 = CARTESIAN_POINT ( 'NONE',  ( 21.71250000122903501, -4.330127018922190985, -2.500000000000001332 ) ) ;
#39718 = CARTESIAN_POINT ( 'NONE',  ( 15.66562500061451857, 3.027376345333613106, -5.243569643749998122 ) ) ;
#39719 = CARTESIAN_POINT ( 'NONE',  ( 13.65937500061451537, -5.492252693125287522, -1.008910452111647106E-15 ) ) ;
#39720 = ORIENTED_EDGE ( 'NONE', *, *, #61840, .T. ) ;
#39721 = CARTESIAN_POINT ( 'NONE',  ( 20.51249999999999929, 2.886751345948126879, 4.999999999999999112 ) ) ;
#39722 = CARTESIAN_POINT ( 'NONE',  ( 24.00000000000000000, 4.330127018922192761, -2.499999999999997780 ) ) ;
#39723 = CARTESIAN_POINT ( 'NONE',  ( 20.82187500061451857, 3.027376345333611329, 5.243569643749999010 ) ) ;
#39724 = CARTESIAN_POINT ( 'NONE',  ( 25.19062500061451715, 6.054752690667223547, 3.707466751127219781E-16 ) ) ;
#39725 = ORIENTED_EDGE ( 'NONE', *, *, #23556, .F. ) ;
#39726 = CARTESIAN_POINT ( 'NONE',  ( -5.810221930991193690E-16, 13.25000000122903465, -34.00000000000000000 ) ) ;
#39727 = CARTESIAN_POINT ( 'NONE',  ( 7.678125000614516082, 4.541064518000418104, 2.621784821874999949 ) ) ;
#39728 = CARTESIAN_POINT ( 'NONE',  ( 65.00000000000000000, 0.000000000000000000, 0.000000000000000000 ) ) ;
#39729 = CIRCLE ( 'NONE', #16082, 5.000000000000000000 ) ;
#39730 = CARTESIAN_POINT ( 'NONE',  ( 15.15000000000000036, 0.000000000000000000, 4.999999999999998224 ) ) ;
#39731 = CARTESIAN_POINT ( 'NONE',  ( 9.001249775931846008E-16, 17.66562500061451502, 34.90005215228797653 ) ) ;
#39732 = CARTESIAN_POINT ( 'NONE',  ( 5.634375000614519458, -4.541064518000419881, 2.621784821874995952 ) ) ;
#39733 = CARTESIAN_POINT ( 'NONE',  ( 26.89687500061451431, -3.027376345333610441, -5.243569643749999898 ) ) ;
#39734 = ORIENTED_EDGE ( 'NONE', *, *, #52008, .T. ) ;
#39735 = CARTESIAN_POINT ( 'NONE',  ( 23.46562500061451573, 3.027376345333611329, 5.243569643749999010 ) ) ;
#39736 = CARTESIAN_POINT ( 'NONE',  ( 24.53437500061451715, -4.541064518000419881, 2.621784821874995952 ) ) ;
#39737 = CARTESIAN_POINT ( 'NONE',  ( 4.243569643749999898, 18.64062500061459104, -27.54997392385601529 ) ) ;
#39738 = CARTESIAN_POINT ( 'NONE',  ( 10.91250000000000320, 2.886751345948129099, -4.999999999999998224 ) ) ;
#39739 = CARTESIAN_POINT ( 'NONE',  ( 8.278125000614515727, -4.541064518000419881, 2.621784821874995952 ) ) ;
#39740 = FACE_OUTER_BOUND ( 'NONE', #19566, .T. ) ;
#39741 = CARTESIAN_POINT ( 'NONE',  ( 1.071796769724491893, 11.13259618943233420, 33.99999999999999289 ) ) ;
#39742 = CARTESIAN_POINT ( 'NONE',  ( 26.46562500061451573, 3.027376345333612662, -5.243569643749998122 ) ) ;
#39744 = EDGE_CURVE ( 'NONE', #65546, #50439, #56623, .T. ) ;
#39743 = CARTESIAN_POINT ( 'NONE',  ( 29.59687500061451360, 4.119189519843966529, -2.378215178124998275 ) ) ;
#39745 = CARTESIAN_POINT ( 'NONE',  ( 13.02187500061451608, 2.746126346562645981, -4.756430356249997438 ) ) ;
#39746 = CARTESIAN_POINT ( 'NONE',  ( 3.215625000614518836, 3.027376345333611329, 5.243569643749999010 ) ) ;
#39747 = CARTESIAN_POINT ( 'NONE',  ( 18.72187500061451360, -6.054752690667223547, -1.112240025338166033E-15 ) ) ;
#39748 = CARTESIAN_POINT ( 'NONE',  ( -2.121784821874996840, 14.08437500061451786, 33.67503911421598417 ) ) ;
#39749 = CARTESIAN_POINT ( 'NONE',  ( 19.84687500061451360, 6.054752690667223547, 3.707466751127219781E-16 ) ) ;
#39750 = CARTESIAN_POINT ( 'NONE',  ( 29.25937500061451502, 4.541064518000418104, -2.621784821874998173 ) ) ;
#39751 = CARTESIAN_POINT ( 'NONE',  ( -2.121784821874996840, 19.03437500061451715, 33.67503911421598417 ) ) ;
#39752 = CARTESIAN_POINT ( 'NONE',  ( 10.15312500061451750, -4.541064518000417216, -2.621784821875001281 ) ) ;
#39753 = CARTESIAN_POINT ( 'NONE',  ( 3.999999999999998668, 17.22500000122903430, 27.69059892324149530 ) ) ;
#39754 = CARTESIAN_POINT ( 'NONE',  ( 7.734375000614517326, 4.541064518000418104, 2.621784821874999949 ) ) ;
#39755 = DIRECTION ( 'NONE',  ( -1.000000000000000000, -0.000000000000000000, -0.000000000000000000 ) ) ;
#39756 = CARTESIAN_POINT ( 'NONE',  ( 8.690625000614515372, -3.027376345333614438, 5.243569643749998122 ) ) ;
#39757 = CARTESIAN_POINT ( 'NONE',  ( 11.97187500061451892, -6.054752690667223547, -1.112240025338166033E-15 ) ) ;
#39758 =( NAMED_UNIT ( * ) PLANE_ANGLE_UNIT ( ) SI_UNIT ( $, .RADIAN. ) );
#39759 = CARTESIAN_POINT ( 'NONE',  ( 18.78750000122903430, 4.330127018922191873, 2.499999999999999556 ) ) ;
#39760 = CARTESIAN_POINT ( 'NONE',  ( 6.759375000614516793, 4.541064518000418104, -2.621784821874998173 ) ) ;
#39761 = CARTESIAN_POINT ( 'NONE',  ( 8.765625000614518214, -6.054752690667223547, -1.112240025338166033E-15 ) ) ;
#39762 = CARTESIAN_POINT ( 'NONE',  ( 16.05000000000000071, 0.000000000000000000, 4.999999999999998224 ) ) ;
#39763 = CARTESIAN_POINT ( 'NONE',  ( 24.16875000122903216, 2.886751345948126879, 4.999999999999999112 ) ) ;
#39764 = CARTESIAN_POINT ( 'NONE',  ( 18.87187500061451573, 3.027376345333613106, -5.243569643749998122 ) ) ;
#39765 = CARTESIAN_POINT ( 'NONE',  ( -5.810221930991193690E-16, 14.48749999999999893, 26.00000000000000355 ) ) ;
#39766 = ORIENTED_EDGE ( 'NONE', *, *, #43656, .F. ) ;
#39767 = CARTESIAN_POINT ( 'NONE',  ( 26.12812500061451360, 4.541064518000418104, 2.621784821874999949 ) ) ;
#39768 = CARTESIAN_POINT ( 'NONE',  ( 13.04062500061451502, 6.054752690667223547, 3.707466751127219781E-16 ) ) ;
#39769 = EDGE_CURVE ( 'NONE', #36659, #4004, #71750, .T. ) ;
#39770 = CARTESIAN_POINT ( 'NONE',  ( 2.878125000614517592, -4.541064518000419881, 2.621784821874995952 ) ) ;
#39771 = CARTESIAN_POINT ( 'NONE',  ( 12.44062500061451537, -3.027376345333610441, -5.243569643749999898 ) ) ;
#39772 = CARTESIAN_POINT ( 'NONE',  ( -4.243569643749999898, 10.40937500061451892, -30.00000000000000000 ) ) ;
#39773 = CARTESIAN_POINT ( 'NONE',  ( 13.91250000122903252, 0.000000000000000000, 4.999999999999998224 ) ) ;
#39774 = CARTESIAN_POINT ( 'NONE',  ( 27.70312500061451289, -4.541064518000417216, -2.621784821875001281 ) ) ;
#39775 = CARTESIAN_POINT ( 'NONE',  ( 2.121784821875001281, 15.00312500061451715, -26.32496088578401938 ) ) ;
#39776 = CARTESIAN_POINT ( 'NONE',  ( 15.56250000122903465, 4.330127018922192761, -2.499999999999997780 ) ) ;
#39777 = CARTESIAN_POINT ( 'NONE',  ( 12.71250000000000036, 2.886751345948129099, -4.999999999999998224 ) ) ;
#39778 = CARTESIAN_POINT ( 'NONE',  ( 19.94062500061451715, -3.027376345333614438, 5.243569643749998122 ) ) ;
#39779 = CARTESIAN_POINT ( 'NONE',  ( 6.871875000614517504, 3.027376345333611329, 5.243569643749999010 ) ) ;
#39780 = CARTESIAN_POINT ( 'NONE',  ( 7.612500001229035362, 0.000000000000000000, 4.999999999999998224 ) ) ;
#39781 = CARTESIAN_POINT ( 'NONE',  ( 16.46250000122903501, 4.330127018922192761, -2.499999999999997780 ) ) ;
#39782 = CARTESIAN_POINT ( 'NONE',  ( 11.95312500061451644, -4.541064518000417216, -2.621784821875001281 ) ) ;
#39783 = CARTESIAN_POINT ( 'NONE',  ( 14.95312500061451644, 0.000000000000000000, 5.243569643749999010 ) ) ;
#39784 = CARTESIAN_POINT ( 'NONE',  ( 27.45000000122903572, -2.886751345948129988, 4.999999999999997335 ) ) ;
#39785 = CARTESIAN_POINT ( 'NONE',  ( 22.34999999999999787, 0.000000000000000000, 4.999999999999998224 ) ) ;
#39786 = CARTESIAN_POINT ( 'NONE',  ( 23.55937500061451573, 0.000000000000000000, 5.243569643749999010 ) ) ;
#39787 = FACE_OUTER_BOUND ( 'NONE', #12848, .T. ) ;
#39788 = CARTESIAN_POINT ( 'NONE',  ( 9.637500001229033941, 6.123233995736764310E-16, -4.999999999999998224 ) ) ;
#39789 = CARTESIAN_POINT ( 'NONE',  ( 27.83437500061451786, 6.421520780324663323E-16, -5.243569643749999010 ) ) ;
#39790 = CARTESIAN_POINT ( 'NONE',  ( 6.234375000614519102, 6.421520780324663323E-16, -5.243569643749999010 ) ) ;
#39791 = CARTESIAN_POINT ( 'NONE',  ( 23.87812500061451715, 4.541064518000418104, 2.621784821874999949 ) ) ;
#39792 = CARTESIAN_POINT ( 'NONE',  ( 3.756430356250000546, 14.59062499938548463, 27.83122392262697886 ) ) ;
#39793 = CARTESIAN_POINT ( 'NONE',  ( 4.898587196589411843E-16, 20.00000000000000000, -26.00000000000000000 ) ) ;
#39794 = CARTESIAN_POINT ( 'NONE',  ( 11.44687500061451857, -3.027376345333614438, 5.243569643749998122 ) ) ;
#39795 = B_SPLINE_CURVE_WITH_KNOTS ( 'NONE', 3,
 ( #28240, #61125, #530, #32689, #72941, #16773 ),
 .UNSPECIFIED., .F., .F.,
 ( 4, 2, 4 ),
 ( 2.013653876781666499E-16, 0.0005272855844084262241, 0.001054571168816651220 ),
 .UNSPECIFIED. ) ;
#39796 = CARTESIAN_POINT ( 'NONE',  ( 4.575260086717169550, 2.016679235498957112, 4.840250765194281435 ) ) ;
#39797 = CARTESIAN_POINT ( 'NONE',  ( 3.646875000614520079, 6.054752690667223547, 3.707466751127219781E-16 ) ) ;
#39798 = CARTESIAN_POINT ( 'NONE',  ( 6.271875000614517859, 3.027376345333613106, -5.243569643749998122 ) ) ;
#39799 = CARTESIAN_POINT ( 'NONE',  ( 6.637500000000001066, -2.886751345948130876, 4.999999999999996447 ) ) ;
#39800 = CARTESIAN_POINT ( 'NONE',  ( 26.78437500061451360, -4.541064518000419881, 2.621784821874995952 ) ) ;
#39801 = CARTESIAN_POINT ( 'NONE',  ( 4.243569643749999898, 10.54062500061459495, 32.45002607614398471 ) ) ;
#39802 = CARTESIAN_POINT ( 'NONE',  ( 18.37500000000000355, -4.330127018922194537, 2.499999999999995559 ) ) ;
#39803 = ORIENTED_EDGE ( 'NONE', *, *, #55282, .F. ) ;
#39804 = CARTESIAN_POINT ( 'NONE',  ( 27.26249999999999929, 2.886751345948126879, 4.999999999999999112 ) ) ;
#39805 = CARTESIAN_POINT ( 'NONE',  ( 29.14687500061451075, -3.027376345333610441, -5.243569643749999898 ) ) ;
#39806 = VERTEX_POINT ( 'NONE', #45652 ) ;
#39807 = CARTESIAN_POINT ( 'NONE',  ( 16.60312500061451857, 4.541064518000418104, -2.621784821874998173 ) ) ;
#39808 = CARTESIAN_POINT ( 'NONE',  ( 9.178125000614517859, -4.541064518000419881, 2.621784821874995952 ) ) ;
#39809 = CARTESIAN_POINT ( 'NONE',  ( 18.38437500061451502, 5.492252693125287522, 3.363034840372157021E-16 ) ) ;
#39810 = CARTESIAN_POINT ( 'NONE',  ( 5.109375000614518214, 0.000000000000000000, 5.243569643749999010 ) ) ;
#39811 = CARTESIAN_POINT ( 'NONE',  ( 17.96250000122903501, 0.000000000000000000, 4.999999999999998224 ) ) ;
#39812 = CARTESIAN_POINT ( 'NONE',  ( 22.42500000000000071, -4.330127018922194537, 2.499999999999995559 ) ) ;
#39813 = CARTESIAN_POINT ( 'NONE',  ( 3.999999999999998668, 13.96250000000000036, -32.30940107675850470 ) ) ;
#39814 = CARTESIAN_POINT ( 'NONE',  ( 3.984375000614517326, 6.421520780324663323E-16, -5.243569643749999010 ) ) ;
#39815 = CARTESIAN_POINT ( 'NONE',  ( 11.85937500061451644, 0.000000000000000000, 5.243569643749999010 ) ) ;
#39816 = CARTESIAN_POINT ( 'NONE',  ( 21.08437500061451786, 6.421520780324663323E-16, -5.243569643749999010 ) ) ;
#39817 = CARTESIAN_POINT ( 'NONE',  ( 4.898587196589412829E-16, 27.50000000000000000, 34.00000000000000000 ) ) ;
#39818 = ORIENTED_EDGE ( 'NONE', *, *, #44518, .F. ) ;
#39819 = EDGE_CURVE ( 'NONE', #29389, #22784, #8504, .T. ) ;
#39820 = CARTESIAN_POINT ( 'NONE',  ( 3.946875000614517681, -3.027376345333610441, -5.243569643749999898 ) ) ;
#39821 = CARTESIAN_POINT ( 'NONE',  ( 7.096875000614517148, -3.027376345333610441, -5.243569643749999898 ) ) ;
#39822 = AXIS2_PLACEMENT_3D ( 'NONE', #55907, #5299, #20446 ) ;
#39823 = CARTESIAN_POINT ( 'NONE',  ( 18.52499999999999858, 6.123233995736764310E-16, -4.999999999999998224 ) ) ;
#39824 = CARTESIAN_POINT ( 'NONE',  ( 14.91562500061451679, 3.027376345333611329, 5.243569643749999010 ) ) ;
#39825 = CARTESIAN_POINT ( 'NONE',  ( -4.000000000000000888, 17.71249999999999858, 32.30940107675850470 ) ) ;
#39826 = CYLINDRICAL_SURFACE ( 'NONE', #50483, 4.999999999999998224 ) ;
#39827 = CARTESIAN_POINT ( 'NONE',  ( 19.65937500061451360, -4.119189519843965641, -2.378215178125001383 ) ) ;
#39828 = CARTESIAN_POINT ( 'NONE',  ( 10.52812500061451750, -4.541064518000419881, 2.621784821874995952 ) ) ;
#39829 = CARTESIAN_POINT ( 'NONE',  ( 27.57187500061451857, 3.027376345333611329, 5.243569643749999010 ) ) ;
#39830 = CARTESIAN_POINT ( 'NONE',  ( 27.98437500061451289, 4.541064518000418104, 2.621784821874999949 ) ) ;
#39831 = CARTESIAN_POINT ( 'NONE',  ( 8.849999999999999645, 0.000000000000000000, 4.999999999999998224 ) ) ;
#39832 = CARTESIAN_POINT ( 'NONE',  ( 1.999999999999998668, 15.01250000122903394, 26.53589838486224650 ) ) ;
#39834 =( BOUNDED_CURVE ( )  B_SPLINE_CURVE ( 2, ( #37700, #8905, #25521, #58758, #70960, #13701, #53976 ),
 .UNSPECIFIED., .F., .F. ) 
 B_SPLINE_CURVE_WITH_KNOTS ( ( 3, 2, 2, 3 ),
 ( 0.8833333333333333037, 0.8861111111111110716, 0.8888888888888888395, 0.8916666666666667185 ),
 .UNSPECIFIED. ) 
 CURVE ( )  GEOMETRIC_REPRESENTATION_ITEM ( )  RATIONAL_B_SPLINE_CURVE ( ( 1.000000000000000000, 0.8660254037844387076, 1.000000000000000000, 0.8660254037844387076, 1.000000000000000000, 0.8660254037844387076, 1.000000000000000000 ) ) 
 REPRESENTATION_ITEM ( '' )  );
#39833 = CARTESIAN_POINT ( 'NONE',  ( 9.450000001229033941, -2.886751345948129988, 4.999999999999997335 ) ) ;
#39835 = CARTESIAN_POINT ( 'NONE',  ( 20.33437500061451786, 4.541064518000418104, 2.621784821874999949 ) ) ;
#39836 = CARTESIAN_POINT ( 'NONE',  ( 13.77187500061451786, -6.054752690667223547, -1.112240025338166033E-15 ) ) ;
#39837 = CARTESIAN_POINT ( 'NONE',  ( 4.898587196589411843E-16, 20.00000000000000000, -26.00000000000000000 ) ) ;
#39838 = ORIENTED_EDGE ( 'NONE', *, *, #2252, .T. ) ;
#39839 = CARTESIAN_POINT ( 'NONE',  ( 14.31562500061451537, 3.027376345333613106, -5.243569643749998122 ) ) ;
#39840 = CARTESIAN_POINT ( 'NONE',  ( 26.43750000122903288, 4.330127018922191873, 2.499999999999999556 ) ) ;
#39841 = CARTESIAN_POINT ( 'NONE',  ( 14.22187500061451537, -6.054752690667223547, -1.112240025338166033E-15 ) ) ;
#39842 = LINE ( 'NONE', #17998, #66570 ) ;
#39843 = CARTESIAN_POINT ( 'NONE',  ( 17.80312500061451786, -4.541064518000417216, -2.621784821875001281 ) ) ;
#39844 = CARTESIAN_POINT ( 'NONE',  ( 18.15000000122903501, -2.886751345948126435, -5.000000000000000000 ) ) ;
#39845 = CARTESIAN_POINT ( 'NONE',  ( 27.19687500061451857, -3.027376345333614438, 5.243569643749998122 ) ) ;
#39846 = CARTESIAN_POINT ( 'NONE',  ( 4.243569643749999010, 11.51562500061451644, 27.54997392385601174 ) ) ;
#39847 = ADVANCED_FACE ( 'NONE', ( #29015 ), #35270, .F. ) ;
#39848 = CARTESIAN_POINT ( 'NONE',  ( 15.83437500061451608, 4.541064518000418104, 2.621784821874999949 ) ) ;
#39849 = CARTESIAN_POINT ( 'NONE',  ( 14.10000000122903252, -2.886751345948125991, -5.000000000000000000 ) ) ;
#39850 = CARTESIAN_POINT ( 'NONE',  ( 8.109375000614518214, 4.119189519843966529, -2.378215178124998275 ) ) ;
#39851 = CARTESIAN_POINT ( 'NONE',  ( 9.001249775931846008E-16, 15.92187500061451821, -25.09994784771203058 ) ) ;
#39852 = CARTESIAN_POINT ( 'NONE',  ( 18.42187500061451644, 3.027376345333613106, -5.243569643749998122 ) ) ;
#39853 = CARTESIAN_POINT ( 'NONE',  ( 19.95000000122903572, -2.886751345948125991, -5.000000000000000000 ) ) ;
#39854 = EDGE_CURVE ( 'NONE', #61742, #4282, #57439, .T. ) ;
#39855 = CARTESIAN_POINT ( 'NONE',  ( 14.25937500061451679, -4.541064518000417216, -2.621784821875001281 ) ) ;
#39856 = CARTESIAN_POINT ( 'NONE',  ( -3.000416591977282496E-16, 11.19687500061451679, 25.09994784771203058 ) ) ;
#39857 = CARTESIAN_POINT ( 'NONE',  ( 23.17500000122903359, 2.886751345948129099, -4.999999999999998224 ) ) ;
#39858 = CARTESIAN_POINT ( 'NONE',  ( 15.59062500061451573, -3.027376345333610441, -5.243569643749999898 ) ) ;
#39859 = DIRECTION ( 'NONE',  ( 0.000000000000000000, 0.000000000000000000, -1.000000000000000000 ) ) ;
#39860 = ORIENTED_EDGE ( 'NONE', *, *, #27502, .T. ) ;
#39861 = VERTEX_POINT ( 'NONE', #17549 ) ;
#39862 = CARTESIAN_POINT ( 'NONE',  ( 20.36249999999999716, 2.886751345948129099, -4.999999999999998224 ) ) ;
#39863 = CARTESIAN_POINT ( 'NONE',  ( 15.03750000122903252, 6.123233995736764310E-16, -4.999999999999998224 ) ) ;
#39864 = CARTESIAN_POINT ( 'NONE',  ( 0.1378111602261695712, 5.000000000000000000, 33.99999999999998579 ) ) ;
#39865 = CARTESIAN_POINT ( 'NONE',  ( 15.45000000122903216, -2.886751345948125991, -5.000000000000000000 ) ) ;
#39866 = CARTESIAN_POINT ( 'NONE',  ( 18.85312500061451502, 4.541064518000418104, -2.621784821874998173 ) ) ;
#39867 = CARTESIAN_POINT ( 'NONE',  ( 23.95312500061451289, 0.000000000000000000, 5.243569643749999010 ) ) ;
#39868 = CARTESIAN_POINT ( 'NONE',  ( 5.690625000614516260, -3.027376345333610441, -5.243569643749999898 ) ) ;
#39869 = CARTESIAN_POINT ( 'NONE',  ( -1.999999999999999112, 20.24374999877096570, 26.53589838486224650 ) ) ;
#39870 = CARTESIAN_POINT ( 'NONE',  ( 17.90625000122903288, 0.000000000000000000, 4.999999999999998224 ) ) ;
#39871 = CARTESIAN_POINT ( 'NONE',  ( 10.35937500061451644, 4.119189519843966529, -2.378215178124998275 ) ) ;
#39872 = CARTESIAN_POINT ( 'NONE',  ( 29.82187500061451502, 3.027376345333611329, 5.243569643749999010 ) ) ;
#39873 = CARTESIAN_POINT ( 'NONE',  ( -3.999999999999999556, 11.07500000122903394, -32.30940107675850470 ) ) ;
#39874 = CARTESIAN_POINT ( 'NONE',  ( 4.243569643749999898, 18.73437500061451644, -30.00000000000000000 ) ) ;
#39875 = CARTESIAN_POINT ( 'NONE',  ( 6.637500001229035718, 4.330127018922191873, 2.499999999999999556 ) ) ;
#39876 = VECTOR ( 'NONE', #29024, 1000.000000000000000 ) ;
#39877 = CARTESIAN_POINT ( 'NONE',  ( 9.299999999999998934, 0.000000000000000000, 4.999999999999998224 ) ) ;
#39878 = CARTESIAN_POINT ( 'NONE',  ( 4.575000001229033941, -5.773502691896255534, -1.060575238724906372E-15 ) ) ;
#39879 = CARTESIAN_POINT ( 'NONE',  ( 12.75937500061451857, 0.000000000000000000, 5.243569643749999010 ) ) ;
#39880 = CARTESIAN_POINT ( 'NONE',  ( 29.76562500061451644, 3.027376345333611329, 5.243569643749999010 ) ) ;
#39881 = CARTESIAN_POINT ( 'NONE',  ( 4.509375000614518569, 4.541064518000418104, -2.621784821874998173 ) ) ;
#39882 = CARTESIAN_POINT ( 'NONE',  ( 3.486133158594716510E-16, 19.55000000122903359, 26.00000000000000355 ) ) ;
#39883 = CARTESIAN_POINT ( 'NONE',  ( 9.459375000614517859, 4.541064518000418104, -2.621784821874998173 ) ) ;
#39884 = CARTESIAN_POINT ( 'NONE',  ( 14.37187500061451928, 3.027376345333613106, -5.243569643749998122 ) ) ;
#39885 = CARTESIAN_POINT ( 'NONE',  ( 1.071796769724491893, 13.94509619066136707, -26.00000000000000355 ) ) ;
#39886 = CARTESIAN_POINT ( 'NONE',  ( 6.000000000000001776, 4.330127018922192761, -2.499999999999997780 ) ) ;
#39887 = CARTESIAN_POINT ( 'NONE',  ( -4.243569643749998122, 16.24062500061459247, 32.45002607614398471 ) ) ;
#39888 = CARTESIAN_POINT ( 'NONE',  ( 21.08437500061451786, 6.421520780324663323E-16, -5.243569643749999010 ) ) ;
#39889 = CARTESIAN_POINT ( 'NONE',  ( 9.674999999999998934, 4.330127018922191873, 2.499999999999999556 ) ) ;
#39890 = CARTESIAN_POINT ( 'NONE',  ( 27.37500000122903288, 2.886751345948126879, 4.999999999999999112 ) ) ;
#39891 = CARTESIAN_POINT ( 'NONE',  ( 18.04687500061451644, 0.000000000000000000, 4.756430356249998326 ) ) ;
#39892 = CARTESIAN_POINT ( 'NONE',  ( 22.26562500061451644, -6.054752690667223547, -1.112240025338166033E-15 ) ) ;
#39893 = CARTESIAN_POINT ( 'NONE',  ( 14.91562500061451679, 3.027376345333611329, 5.243569643749999010 ) ) ;
#39894 = CARTESIAN_POINT ( 'NONE',  ( 26.40937500061451360, 2.746126346562645981, -4.756430356249997438 ) ) ;
#39895 = CARTESIAN_POINT ( 'NONE',  ( 11.59687500061451892, -3.027376345333610441, -5.243569643749999898 ) ) ;
#39896 = CARTESIAN_POINT ( 'NONE',  ( 27.67499999999999716, 4.330127018922191873, 2.499999999999999556 ) ) ;
#39897 = CARTESIAN_POINT ( 'NONE',  ( 24.48750000122903359, 6.123233995736764310E-16, -4.999999999999998224 ) ) ;
#39898 = CARTESIAN_POINT ( 'NONE',  ( 3.309375000614518836, 0.000000000000000000, 5.243569643749999010 ) ) ;
#39899 = CARTESIAN_POINT ( 'NONE',  ( 13.54687500061451999, 6.054752690667223547, 3.707466751127219781E-16 ) ) ;
#39900 = CARTESIAN_POINT ( 'NONE',  ( 21.03749999999999787, -2.886751345948102898, 5.000000000000044409 ) ) ;
#39901 = CARTESIAN_POINT ( 'NONE',  ( 21.67500000000000071, 6.123233995736764310E-16, -4.999999999999998224 ) ) ;
#39902 = CYLINDRICAL_SURFACE ( 'NONE', #36026, 4.999999999999998224 ) ;
#39903 = CARTESIAN_POINT ( 'NONE',  ( 23.18437500061451573, -4.541064518000419881, 2.621784821874995952 ) ) ;
#39904 = CARTESIAN_POINT ( 'NONE',  ( 13.50937500061451679, 4.541064518000418104, -2.621784821874998173 ) ) ;
#39905 = CARTESIAN_POINT ( 'NONE',  ( -1.878215178124999163, 16.05312499938548143, 26.74683588394047007 ) ) ;
#39906 = CARTESIAN_POINT ( 'NONE',  ( 25.01249999999999929, 2.886751345948126879, 4.999999999999999112 ) ) ;
#39907 = CARTESIAN_POINT ( 'NONE',  ( 3.487500001229035362, 4.330127018922191873, 2.499999999999999556 ) ) ;
#39908 = CARTESIAN_POINT ( 'NONE',  ( 27.98437500061451289, 4.119189519843966529, 2.378215178124999607 ) ) ;
#39909 = CARTESIAN_POINT ( 'NONE',  ( 17.61562500061451786, 3.027376345333611329, 5.243569643749999010 ) ) ;
#39910 = CARTESIAN_POINT ( 'NONE',  ( 7.837499999999999467, 5.773502691896255534, 3.535250795749688894E-16 ) ) ;
#39911 = CARTESIAN_POINT ( 'NONE',  ( -1.071796769724491005, 14.05759618943233669, 26.00000000000000355 ) ) ;
#39912 = CARTESIAN_POINT ( 'NONE',  ( 17.92500000000000071, -4.330127018922194537, 2.499999999999995559 ) ) ;
#39913 = CARTESIAN_POINT ( 'NONE',  ( 4.243569643749999010, 13.76562500061451644, 27.54997392385601174 ) ) ;
#39914 = CARTESIAN_POINT ( 'NONE',  ( 45.00000000000000000, 6.123233995736764310E-16, -4.999999999999998224 ) ) ;
#39915 = CARTESIAN_POINT ( 'NONE',  ( 20.73750000122903359, -4.330127018922194537, 2.499999999999995559 ) ) ;
#39916 = CARTESIAN_POINT ( 'NONE',  ( 27.98437500061451289, 4.541064518000418104, 2.621784821874999949 ) ) ;
#39917 = ORIENTED_EDGE ( 'NONE', *, *, #48306, .T. ) ;
#39918 = CARTESIAN_POINT ( 'NONE',  ( 21.02812500061451573, 6.421520780324663323E-16, -5.243569643749999010 ) ) ;
#39919 = CARTESIAN_POINT ( 'NONE',  ( 22.80937500061451573, -4.541064518000417216, -2.621784821875001281 ) ) ;
#39920 = CARTESIAN_POINT ( 'NONE',  ( 3.225000000000002309, 6.123233995736764310E-16, -4.999999999999998224 ) ) ;
#39921 = CARTESIAN_POINT ( 'NONE',  ( 9.553125000614517859, 0.000000000000000000, 5.243569643749999010 ) ) ;
#39922 = CARTESIAN_POINT ( 'NONE',  ( 23.42812500061451786, 4.541064518000418104, 2.621784821874999949 ) ) ;
#39923 = CARTESIAN_POINT ( 'NONE',  ( 13.02187500061451608, 3.027376345333613106, -5.243569643749998122 ) ) ;
#39924 = CARTESIAN_POINT ( 'NONE',  ( 16.02187500061451786, -6.054752690667223547, -1.112240025338166033E-15 ) ) ;
#39925 = CARTESIAN_POINT ( 'NONE',  ( 4.243569643749999010, 17.36562500061451786, 27.54997392385601174 ) ) ;
#39926 = CARTESIAN_POINT ( 'NONE',  ( 20.21250000122903145, 0.000000000000000000, 4.999999999999998224 ) ) ;
#39927 = CARTESIAN_POINT ( 'NONE',  ( 15.23437500061451644, 5.824947211148865298E-16, -4.756430356249998326 ) ) ;
#39928 = CARTESIAN_POINT ( 'NONE',  ( 13.07812500061451821, 4.541064518000418104, 2.621784821874999949 ) ) ;
#39929 = CARTESIAN_POINT ( 'NONE',  ( 4.809375000614516615, -4.541064518000417216, -2.621784821875001281 ) ) ;
#39930 = CARTESIAN_POINT ( 'NONE',  ( 5.109375000614518214, 0.000000000000000000, 5.243569643749999010 ) ) ;
#39931 = EDGE_LOOP ( 'NONE', ( #46237, #64871, #65591, #55972 ) ) ;
#39932 = CARTESIAN_POINT ( 'NONE',  ( 26.07187500061451857, 3.027376345333613106, -5.243569643749998122 ) ) ;
#39933 = CARTESIAN_POINT ( 'NONE',  ( 16.34062500061451573, -3.027376345333614438, 5.243569643749998122 ) ) ;
#39934 = CARTESIAN_POINT ( 'NONE',  ( 27.33750000122903145, 4.330127018922191873, 2.499999999999999556 ) ) ;
#39935 = ADVANCED_FACE ( 'NONE', ( #51186 ), #46368, .T. ) ;
#39936 = CARTESIAN_POINT ( 'NONE',  ( 28.26562500061451289, 3.027376345333613106, -5.243569643749998122 ) ) ;
#39937 = CARTESIAN_POINT ( 'NONE',  ( 22.50937500061451857, 4.541064518000418104, -2.621784821874998173 ) ) ;
#39938 = CARTESIAN_POINT ( 'NONE',  ( 16.49062500061451786, -3.027376345333610441, -5.243569643749999898 ) ) ;
#39939 = CARTESIAN_POINT ( 'NONE',  ( -2.121784821874996840, 19.03437500061451715, 33.67503911421598417 ) ) ;
#39940 = CARTESIAN_POINT ( 'NONE',  ( 23.05312500061451431, 0.000000000000000000, 5.243569643749999010 ) ) ;
#39941 = CARTESIAN_POINT ( 'NONE',  ( 3.750000001229034652, -2.886751345948125991, -5.000000000000000000 ) ) ;
#39942 = ORIENTED_EDGE ( 'NONE', *, *, #32530, .F. ) ;
#39943 = CARTESIAN_POINT ( 'NONE',  ( 27.44999999999999929, -4.330127018922190985, -2.500000000000001332 ) ) ;
#39944 = CARTESIAN_POINT ( 'NONE',  ( -2.000000000000000000, 12.27500000000000036, -33.46410161513775705 ) ) ;
#39945 = CARTESIAN_POINT ( 'NONE',  ( 2.655984681222220721E-16, 17.81562499938548427, 25.66244784525396483 ) ) ;
#39946 = CARTESIAN_POINT ( 'NONE',  ( 3.084375000614519191, 6.421520780324663323E-16, -5.243569643749999010 ) ) ;
#39947 = CARTESIAN_POINT ( 'NONE',  ( 10.15312500061451750, -4.541064518000417216, -2.621784821875001281 ) ) ;
#39948 = CARTESIAN_POINT ( 'NONE',  ( 22.91250000122903430, 0.000000000000000000, 4.999999999999998224 ) ) ;
#39949 = CARTESIAN_POINT ( 'NONE',  ( 12.57187500061452035, 3.027376345333612662, -5.243569643749998122 ) ) ;
#39950 = CARTESIAN_POINT ( 'NONE',  ( 26.05312500061451431, 4.541064518000418104, -2.621784821874998173 ) ) ;
#39951 = CARTESIAN_POINT ( 'NONE',  ( 27.07499999999999929, 6.123233995736764310E-16, -4.999999999999998224 ) ) ;
#39952 = CARTESIAN_POINT ( 'NONE',  ( 1.999999999999998668, 18.61250000122903359, -33.46410161513775705 ) ) ;
#39953 = CARTESIAN_POINT ( 'NONE',  ( 4.115625000614516082, 3.027376345333611329, 5.243569643749999010 ) ) ;
#39954 = CARTESIAN_POINT ( 'NONE',  ( 11.91562500061451857, -6.054752690667223547, -1.112240025338166033E-15 ) ) ;
#39955 = ORIENTED_EDGE ( 'NONE', *, *, #23306, .T. ) ;
#39956 = CARTESIAN_POINT ( 'NONE',  ( 8.240625000614516082, -3.027376345333614438, 5.243569643749998122 ) ) ;
#39957 = CARTESIAN_POINT ( 'NONE',  ( 6.215625000614517504, 3.027376345333613106, -5.243569643749998122 ) ) ;
#39958 = CARTESIAN_POINT ( 'NONE',  ( 16.02187500061451786, -5.492252693125287522, -1.008910452111647106E-15 ) ) ;
#39959 = FACE_OUTER_BOUND ( 'NONE', #19285, .T. ) ;
#39960 = CARTESIAN_POINT ( 'NONE',  ( 15.11249999999999893, 2.886751345948126879, 4.999999999999999112 ) ) ;
#39961 = CARTESIAN_POINT ( 'NONE',  ( 17.25937500061451502, 0.000000000000000000, 5.243569643749999010 ) ) ;
#39962 = CARTESIAN_POINT ( 'NONE',  ( 10.46250000122903323, -4.330127018922190985, -2.500000000000001332 ) ) ;
#39963 = CARTESIAN_POINT ( 'NONE',  ( 19.88437500061451857, 4.541064518000418104, 2.621784821874999949 ) ) ;
#39964 = CARTESIAN_POINT ( 'NONE',  ( 18.97499999999999787, 6.123233995736764310E-16, -4.999999999999998224 ) ) ;
#39965 = CARTESIAN_POINT ( 'NONE',  ( 21.27187500061451786, 3.027376345333611329, 5.243569643749999010 ) ) ;
#39966 = CARTESIAN_POINT ( 'NONE',  ( -2.121784821874996840, 14.47812500061451679, -26.32496088578401583 ) ) ;
#39967 = DIRECTION ( 'NONE',  ( 0.000000000000000000, 6.195440985631456550E-17, 1.000000000000000000 ) ) ;
#39968 = CARTESIAN_POINT ( 'NONE',  ( 24.53437500061451715, -2.746126346562641984, -4.756430356249999214 ) ) ;
#39969 = CARTESIAN_POINT ( 'NONE',  ( -5.810221930991193690E-16, 11.78749999999999964, -34.00000000000000000 ) ) ;
#39970 = CARTESIAN_POINT ( 'NONE',  ( 27.10312500061451502, 0.000000000000000000, 5.243569643749999010 ) ) ;
#39971 = CARTESIAN_POINT ( 'NONE',  ( 17.13750000122903216, -4.330127018922194537, 2.499999999999995559 ) ) ;
#39972 = CARTESIAN_POINT ( 'NONE',  ( 28.50937500061451502, 0.000000000000000000, 5.243569643749999010 ) ) ;
#39973 =( BOUNDED_CURVE ( )  B_SPLINE_CURVE ( 2, ( #37732, #58791, #48828, #71358, #20732, #2660, #15193, #60251, #19995 ),
 .UNSPECIFIED., .F., .F. ) 
 B_SPLINE_CURVE_WITH_KNOTS ( ( 3, 2, 2, 2, 3 ),
 ( 0.6195652173913043237, 0.6231884057971014412, 0.6304347826086956763, 0.6376811594202898004, 0.6413043478260869179 ),
 .UNSPECIFIED. ) 
 CURVE ( )  GEOMETRIC_REPRESENTATION_ITEM ( )  RATIONAL_B_SPLINE_CURVE ( ( 0.9330127018922194093, 0.9330127018922194093, 1.000000000000000000, 0.8660254037844387076, 1.000000000000000000, 0.8660254037844387076, 1.000000000000000000, 0.9330127018922194093, 0.9330127018922194093 ) ) 
 REPRESENTATION_ITEM ( '' )  );
#39974 = CARTESIAN_POINT ( 'NONE',  ( 24.07499999999999929, 4.330127018922191873, 2.499999999999999556 ) ) ;
#39975 = EDGE_CURVE ( 'NONE', #51457, #27655, #23597, .T. ) ;
#39976 = CARTESIAN_POINT ( 'NONE',  ( 6.815625000614517148, 3.027376345333611329, 5.243569643749999010 ) ) ;
#39977 = CARTESIAN_POINT ( 'NONE',  ( 24.00937500061451502, -5.492252693125287522, -1.008910452111647106E-15 ) ) ;
#39978 = CARTESIAN_POINT ( 'NONE',  ( 19.43437500061451928, 4.541064518000418104, 2.621784821874999949 ) ) ;
#39979 = CARTESIAN_POINT ( 'NONE',  ( 10.39687500061451608, 0.000000000000000000, 4.756430356249998326 ) ) ;
#39980 = CARTESIAN_POINT ( 'NONE',  ( 5.690625000614516260, -3.027376345333610441, -5.243569643749999898 ) ) ;
#39981 = CARTESIAN_POINT ( 'NONE',  ( 11.18437500061451928, 6.421520780324663323E-16, -5.243569643749999010 ) ) ;
#39982 = ORIENTED_EDGE ( 'NONE', *, *, #33073, .F. ) ;
#39983 = CARTESIAN_POINT ( 'NONE',  ( 21.19687500061451502, 6.054752690667223547, 3.707466751127219781E-16 ) ) ;
#39984 = CARTESIAN_POINT ( 'NONE',  ( 8.081250001229031810, -4.330127018922194537, 2.499999999999995559 ) ) ;
#39985 = CARTESIAN_POINT ( 'NONE',  ( 28.16249999999999787, 2.886751345948126879, 4.999999999999999112 ) ) ;
#39986 = CARTESIAN_POINT ( 'NONE',  ( 29.25937500061451502, 4.541064518000418104, -2.621784821874998173 ) ) ;
#39987 = DIRECTION ( 'NONE',  ( -0.000000000000000000, -1.000000000000000000, -0.000000000000000000 ) ) ;
#39988 = ORIENTED_EDGE ( 'NONE', *, *, #14507, .T. ) ;
#39989 = CARTESIAN_POINT ( 'NONE',  ( 10.61250000000000071, 2.886751345948126879, 4.999999999999999112 ) ) ;
#39990 = CARTESIAN_POINT ( 'NONE',  ( 15.34687500061451537, 0.000000000000000000, 4.756430356249998326 ) ) ;
#39991 = CARTESIAN_POINT ( 'NONE',  ( 25.04062500061451502, -3.027376345333610441, -5.243569643749999898 ) ) ;
#39992 = CARTESIAN_POINT ( 'NONE',  ( 14.17500000000000071, 4.330127018922191873, 2.499999999999999556 ) ) ;
#39993 = CARTESIAN_POINT ( 'NONE',  ( 11.02500000122903501, 2.886751345948129099, -4.999999999999998224 ) ) ;
#39994 = CARTESIAN_POINT ( 'NONE',  ( 10.04062500061451502, -3.027376345333614438, 5.243569643749998122 ) ) ;
#39995 = CARTESIAN_POINT ( 'NONE',  ( 9.449999999999999289, -4.330127018922190985, -2.500000000000001332 ) ) ;
#39996 = DIRECTION ( 'NONE',  ( -1.000000000000000000, -0.000000000000000000, -0.000000000000000000 ) ) ;
#39997 = CARTESIAN_POINT ( 'NONE',  ( 28.57500000122903572, 2.886751345948129099, -4.999999999999998224 ) ) ;
#39998 = CARTESIAN_POINT ( 'NONE',  ( -3.756430356250000990, 16.05312499938548143, 32.16877607737301048 ) ) ;
#39999 = CARTESIAN_POINT ( 'NONE',  ( 7.575000000000001954, -4.330127018922194537, 2.499999999999995559 ) ) ;
#40000 = CARTESIAN_POINT ( 'NONE',  ( 18.75000000000000000, 0.000000000000000000, 4.999999999999998224 ) ) ;
#40001 = ORIENTED_EDGE ( 'NONE', *, *, #30947, .T. ) ;
#40002 = CARTESIAN_POINT ( 'NONE',  ( 21.59062500061451928, 6.054752690667223547, 3.707466751127219781E-16 ) ) ;
#40003 = CARTESIAN_POINT ( 'NONE',  ( 29.01562500061451644, -6.054752690667223547, -1.112240025338166033E-15 ) ) ;
#40004 = CARTESIAN_POINT ( 'NONE',  ( 29.22187500061451715, 3.027376345333613106, -5.243569643749998122 ) ) ;
#40005 = CARTESIAN_POINT ( 'NONE',  ( 19.09687500061451360, -3.027376345333614438, 5.243569643749998122 ) ) ;
#40006 = ADVANCED_FACE ( 'NONE', ( #590 ), #52629, .F. ) ;
#40007 = CARTESIAN_POINT ( 'NONE',  ( 16.15312500061451573, 4.541064518000418104, -2.621784821874998173 ) ) ;
#40008 = CARTESIAN_POINT ( 'NONE',  ( 4.243569643749999898, 10.57812500061459637, -30.00000000000000000 ) ) ;
#40009 = CARTESIAN_POINT ( 'NONE',  ( 3.028125000614518392, 6.421520780324663323E-16, -5.243569643749999010 ) ) ;
#40010 = CARTESIAN_POINT ( 'NONE',  ( 27.71250000122903145, 4.330127018922192761, -2.499999999999997780 ) ) ;
#40011 = CARTESIAN_POINT ( 'NONE',  ( 22.39687500061451075, -2.746126346562641984, -4.756430356249999214 ) ) ;
#40012 = CARTESIAN_POINT ( 'NONE',  ( 19.86562500061451786, 3.027376345333611329, 5.243569643749999010 ) ) ;
#40013 = CARTESIAN_POINT ( 'NONE',  ( 65.00000000000000000, 0.000000000000000000, 0.000000000000000000 ) ) ;
#40014 = CARTESIAN_POINT ( 'NONE',  ( 2.850000001229036073, -2.886751345948125991, -5.000000000000000000 ) ) ;
#40015 = CARTESIAN_POINT ( 'NONE',  ( 13.05937500061451750, 4.541064518000418104, -2.621784821874998173 ) ) ;
#40016 = CARTESIAN_POINT ( 'NONE',  ( 10.95937500061451964, 0.000000000000000000, 5.243569643749999010 ) ) ;
#40017 = CARTESIAN_POINT ( 'NONE',  ( 20.22187500061451715, 3.027376345333613106, -5.243569643749998122 ) ) ;
#40018 = ORIENTED_EDGE ( 'NONE', *, *, #33576, .F. ) ;
#40019 = CARTESIAN_POINT ( 'NONE',  ( 2.164655401860464234, 4.642258459466365395, 2.164655401860464234 ) ) ;
#40020 = CARTESIAN_POINT ( 'NONE',  ( 24.74062500061451786, 6.054752690667223547, 3.707466751127219781E-16 ) ) ;
#40021 = CARTESIAN_POINT ( 'NONE',  ( 19.80937500061451573, 4.541064518000418104, -2.621784821874998173 ) ) ;
#40022 = CARTESIAN_POINT ( 'NONE',  ( 24.77812500061451217, 4.541064518000418104, 2.621784821874999949 ) ) ;
#40023 = DIRECTION ( 'NONE',  ( -1.000000000000000000, -0.000000000000000000, -0.000000000000000000 ) ) ;
#40024 = CARTESIAN_POINT ( 'NONE',  ( -2.000000000000000000, 17.67500000000000071, 26.53589838486224650 ) ) ;
#40025 = CARTESIAN_POINT ( 'NONE',  ( 28.56562500061451715, -6.054752690667223547, -1.112240025338166033E-15 ) ) ;
#40026 = CONTEXT_DEPENDENT_SHAPE_REPRESENTATION ( #4000, #25489 ) ;
#40027 = CARTESIAN_POINT ( 'NONE',  ( 11.62500000122903465, 2.886751345948126879, 4.999999999999999112 ) ) ;
#40028 = CARTESIAN_POINT ( 'NONE',  ( 7.950000001229033053, 5.773502691896255534, 3.535250795749688894E-16 ) ) ;
#40029 = CARTESIAN_POINT ( 'NONE',  ( 8.484601909799253346E-16, 19.21250000000000213, -25.38119784648299770 ) ) ;
#40030 = CARTESIAN_POINT ( 'NONE',  ( 27.15000000122902790, -2.886751345948125991, -5.000000000000000000 ) ) ;
#40031 = CARTESIAN_POINT ( 'NONE',  ( 1.999999999999997335, 17.31874999877096499, 33.46410161513775705 ) ) ;
#40032 = CARTESIAN_POINT ( 'NONE',  ( 16.51875000122903359, 2.886751345948126879, 4.999999999999999112 ) ) ;
#40033 = CARTESIAN_POINT ( 'NONE',  ( 9.234375000614518214, -4.541064518000419881, 2.621784821874995952 ) ) ;
#40034 = DIRECTION ( 'NONE',  ( -1.000000000000000000, -0.000000000000000000, -0.000000000000000000 ) ) ;
#40035 = CARTESIAN_POINT ( 'NONE',  ( 16.30312500061451786, 0.000000000000000000, 5.243569643749999010 ) ) ;
#40036 = CARTESIAN_POINT ( 'NONE',  ( 13.17187500061451999, 3.027376345333611329, 5.243569643749999010 ) ) ;
#40037 = CARTESIAN_POINT ( 'NONE',  ( 28.65000000122903145, 5.773502691896255534, 3.535250795749688894E-16 ) ) ;
#40038 = CARTESIAN_POINT ( 'NONE',  ( 20.14687500061451786, -3.027376345333610441, -5.243569643749999898 ) ) ;
#40039 = CARTESIAN_POINT ( 'NONE',  ( 6.346875000614517148, 6.054752690667223547, 3.707466751127219781E-16 ) ) ;
#40040 = CARTESIAN_POINT ( 'NONE',  ( 3.665625000614517681, 3.027376345333611329, 5.243569643749999010 ) ) ;
#40041 = CYLINDRICAL_SURFACE ( 'NONE', #16769, 4.000000000000000000 ) ;
#40042 = CARTESIAN_POINT ( 'NONE',  ( 10.19062500061451892, -3.027376345333610441, -5.243569643749999898 ) ) ;
#40043 =( BOUNDED_CURVE ( )  B_SPLINE_CURVE ( 2, ( #26246, #15146, #71681, #37683, #43606, #3358, #38796 ),
 .UNSPECIFIED., .F., .F. ) 
 B_SPLINE_CURVE_WITH_KNOTS ( ( 3, 2, 2, 3 ),
 ( 0.4200000000000000955, 0.4233333333333334503, 0.4266666666666668051, 0.4300000000000001044 ),
 .UNSPECIFIED. ) 
 CURVE ( )  GEOMETRIC_REPRESENTATION_ITEM ( )  RATIONAL_B_SPLINE_CURVE ( ( 0.9999999999999955591, 0.8660254037844431485, 1.000000000000000000, 0.8660254037844387076, 1.000000000000000000, 0.8660254037844342667, 1.000000000000004441 ) ) 
 REPRESENTATION_ITEM ( '' )  );
#40044 = CARTESIAN_POINT ( 'NONE',  ( 19.60312500061451502, -4.541064518000417216, -2.621784821875001281 ) ) ;
#40045 = ORIENTED_EDGE ( 'NONE', *, *, #19955, .F. ) ;
#40046 = B_SPLINE_CURVE_WITH_KNOTS ( 'NONE', 3,
 ( #26127, #15397, #66017, #65277, #49038, #37939, #15035, #26869, #60830, #10236 ),
 .UNSPECIFIED., .F., .F.,
 ( 4, 3, 3, 4 ),
 ( 0.000000000000000000, 5.625091169402055566E-05, 9.375822253212263134E-05, 0.0001312677523608356484 ),
 .UNSPECIFIED. ) ;
#40047 = CARTESIAN_POINT ( 'NONE',  ( 5.625000001229036428, 2.886751345948129099, -4.999999999999998224 ) ) ;
#40048 = CARTESIAN_POINT ( 'NONE',  ( 17.65312500061451573, 0.000000000000000000, 5.243569643749999010 ) ) ;
#40049 = CARTESIAN_POINT ( 'NONE',  ( 13.49062500061451608, 6.054752690667223547, 3.707466751127219781E-16 ) ) ;
#40050 = CARTESIAN_POINT ( 'NONE',  ( 24.23437500061451644, 5.824947211148865298E-16, -4.756430356249998326 ) ) ;
#40051 = CARTESIAN_POINT ( 'NONE',  ( 12.90000000000000213, 0.000000000000000000, 4.999999999999998224 ) ) ;
#40052 = CARTESIAN_POINT ( 'NONE',  ( 8.250000001229034652, -2.886751345948125991, -5.000000000000000000 ) ) ;
#40053 = CARTESIAN_POINT ( 'NONE',  ( 5.578125000614518214, -4.541064518000419881, 2.621784821874995952 ) ) ;
#40054 = CARTESIAN_POINT ( 'NONE',  ( 17.77500000122903145, 2.886751345948129099, -4.999999999999998224 ) ) ;
#40055 = CARTESIAN_POINT ( 'NONE',  ( 27.75000000000000000, 0.000000000000000000, 4.999999999999998224 ) ) ;
#40056 = CARTESIAN_POINT ( 'NONE',  ( -2.121784821874999949, 10.33437500061451786, -33.67503911421598417 ) ) ;
#40057 = CARTESIAN_POINT ( 'NONE',  ( 3.675000001229035362, -5.773502691896255534, -1.060575238724906372E-15 ) ) ;
#40058 = CARTESIAN_POINT ( 'NONE',  ( 5.000000000000000000, 39.99999999999999289, 30.00000000000000000 ) ) ;
#40059 = CARTESIAN_POINT ( 'NONE',  ( 19.58437500061451786, -4.541064518000419881, 2.621784821874995952 ) ) ;
#40060 = DIRECTION ( 'NONE',  ( -1.000000000000000000, -0.000000000000000000, -0.000000000000000000 ) ) ;
#40061 = EDGE_CURVE ( 'NONE', #6439, #66791, #23165, .T. ) ;
#40062 = CARTESIAN_POINT ( 'NONE',  ( 15.55312500061451608, -4.541064518000417216, -2.621784821875001281 ) ) ;
#40063 = CARTESIAN_POINT ( 'NONE',  ( 8.906250001229031099, 0.000000000000000000, 4.999999999999998224 ) ) ;
#40064 = CARTESIAN_POINT ( 'NONE',  ( 15.86250000122903181, -4.330127018922190985, -2.500000000000001332 ) ) ;
#40065 = CARTESIAN_POINT ( 'NONE',  ( 29.37187500061451928, 3.027376345333611329, 5.243569643749999010 ) ) ;
#40066 = CARTESIAN_POINT ( 'NONE',  ( 27.38437500061451857, 6.421520780324663323E-16, -5.243569643749999010 ) ) ;
#40067 = CARTESIAN_POINT ( 'NONE',  ( 19.58437500061451786, -2.746126346562641984, -4.756430356249999214 ) ) ;
#40068 = CARTESIAN_POINT ( 'NONE',  ( 12.29062500061451857, -3.027376345333614438, 5.243569643749998122 ) ) ;
#40069 = CARTESIAN_POINT ( 'NONE',  ( 10.39687500061451786, 6.054752690667223547, 3.707466751127219781E-16 ) ) ;
#40070 = ORIENTED_EDGE ( 'NONE', *, *, #2651, .F. ) ;
#40071 = CARTESIAN_POINT ( 'NONE',  ( 28.97812500061451502, -4.541064518000419881, 2.621784821874995952 ) ) ;
#40072 = CARTESIAN_POINT ( 'NONE',  ( 21.02812500061451573, 6.421520780324663323E-16, -5.243569643749999010 ) ) ;
#40073 = CARTESIAN_POINT ( 'NONE',  ( 3.999999999999998668, 13.17500000122903536, -32.30940107675850470 ) ) ;
#40074 = ADVANCED_FACE ( 'NONE', ( #31181 ), #35890, .T. ) ;
#40075 = CARTESIAN_POINT ( 'NONE',  ( 10.05000000000000071, 4.330127018922192761, -2.499999999999997780 ) ) ;
#40076 = CARTESIAN_POINT ( 'NONE',  ( 21.37500000122902932, 2.886751345948129099, -4.999999999999998224 ) ) ;
#40077 = CARTESIAN_POINT ( 'NONE',  ( 15.29062500061451679, 6.054752690667223547, 3.707466751127219781E-16 ) ) ;
#40078 = CARTESIAN_POINT ( 'NONE',  ( 13.28437500061451537, -2.746126346562642428, -4.756430356249999214 ) ) ;
#40079 = ORIENTED_EDGE ( 'NONE', *, *, #51734, .F. ) ;
#40080 = CARTESIAN_POINT ( 'NONE',  ( 19.12500000000000000, 4.330127018922191873, 2.499999999999999556 ) ) ;
#40081 = EDGE_CURVE ( 'NONE', #50521, #8942, #56628, .T. ) ;
#40082 = CARTESIAN_POINT ( 'NONE',  ( 21.93750000000000000, -2.886751345948129988, 4.999999999999997335 ) ) ;
#40083 = CARTESIAN_POINT ( 'NONE',  ( 20.59687500061451360, -3.027376345333610441, -5.243569643749999898 ) ) ;
#40084 = CARTESIAN_POINT ( 'NONE',  ( 25.41562500061451146, -6.054752690667223547, -1.112240025338166033E-15 ) ) ;
#40085 = ORIENTED_EDGE ( 'NONE', *, *, #67290, .F. ) ;
#40086 = CARTESIAN_POINT ( 'NONE',  ( 28.61250000000000071, 2.886751345948143754, 4.999999999999969802 ) ) ;
#40087 = CARTESIAN_POINT ( 'NONE',  ( 8.165625000614516793, 3.027376345333611329, 5.243569643749999010 ) ) ;
#40088 = CARTESIAN_POINT ( 'NONE',  ( 3.999999999999998668, 12.16250000000000320, 27.69059892324149530 ) ) ;
#40089 = CARTESIAN_POINT ( 'NONE',  ( 14.06250000000000000, 2.886751345948129099, -4.999999999999998224 ) ) ;
#40090 = CARTESIAN_POINT ( 'NONE',  ( -4.243569643749997233, 17.59062500061451928, 32.45002607614398471 ) ) ;
#40091 = CARTESIAN_POINT ( 'NONE',  ( 29.50312500061451360, -4.541064518000417216, -2.621784821875001281 ) ) ;
#40092 = CARTESIAN_POINT ( 'NONE',  ( 25.88437500061451502, -4.541064518000419881, 2.621784821874995952 ) ) ;
#40093 = ORIENTED_EDGE ( 'NONE', *, *, #19563, .T. ) ;
#40094 = CARTESIAN_POINT ( 'NONE',  ( 23.57812500061451289, -4.541064518000419881, 2.621784821874995952 ) ) ;
#40095 = CARTESIAN_POINT ( 'NONE',  ( 26.37187500061451217, -6.054752690667223547, -1.112240025338166033E-15 ) ) ;
#40096 = CARTESIAN_POINT ( 'NONE',  ( 4.243569643749999010, 18.26562500061459104, -32.45002607614398471 ) ) ;
#40097 = CARTESIAN_POINT ( 'NONE',  ( 11.06250000000000000, 2.886751345948126879, 4.999999999999999112 ) ) ;
#40098 = CARTESIAN_POINT ( 'NONE',  ( 9.065625000614517148, 3.027376345333611329, 5.243569643749999010 ) ) ;
#40099 = CARTESIAN_POINT ( 'NONE',  ( 28.24687500061451573, -2.746126346562641984, -4.756430356249999214 ) ) ;
#40100 = CARTESIAN_POINT ( 'NONE',  ( 29.54062500061451502, -3.027376345333610441, -5.243569643749999898 ) ) ;
#40101 = CARTESIAN_POINT ( 'NONE',  ( 27.21562500061451573, -6.054752690667223547, -1.112240025338166033E-15 ) ) ;
#40102 = CARTESIAN_POINT ( 'NONE',  ( 29.52187500061451431, 5.824947211148865298E-16, -4.756430356249998326 ) ) ;
#40103 = CARTESIAN_POINT ( 'NONE',  ( 13.73437500061451821, -4.119189519843968306, 2.378215178124996054 ) ) ;
#40104 = CARTESIAN_POINT ( 'NONE',  ( 19.69687500061451857, -3.027376345333610441, -5.243569643749999898 ) ) ;
#40105 = CARTESIAN_POINT ( 'NONE',  ( -4.243569643749997233, 15.39687500061451786, 32.45002607614398471 ) ) ;
#40106 = CARTESIAN_POINT ( 'NONE',  ( 20.22187500061451715, 3.027376345333613106, -5.243569643749998122 ) ) ;
#40107 = CARTESIAN_POINT ( 'NONE',  ( 27.08437500061451786, 4.541064518000418104, 2.621784821874999949 ) ) ;
#40108 = CARTESIAN_POINT ( 'NONE',  ( -4.243569643749999898, 16.25937500061451857, 30.00000000000000000 ) ) ;
#40109 = CARTESIAN_POINT ( 'NONE',  ( 9.403125000614517504, 4.541064518000418104, -2.621784821874998173 ) ) ;
#40110 = CARTESIAN_POINT ( 'NONE',  ( 16.61250000122903359, 0.000000000000000000, 4.999999999999998224 ) ) ;
#40111 = CARTESIAN_POINT ( 'NONE',  ( 5.784375000614517148, 6.421520780324663323E-16, -5.243569643749999010 ) ) ;
#40112 = CARTESIAN_POINT ( 'NONE',  ( 26.06250000122903288, 0.000000000000000000, 4.999999999999998224 ) ) ;
#40113 = CARTESIAN_POINT ( 'NONE',  ( 7.340625000614518392, -3.027376345333614438, 5.243569643749998122 ) ) ;
#40114 = CARTESIAN_POINT ( 'NONE',  ( 12.60937500061451821, 4.541064518000418104, -2.621784821874998173 ) ) ;
#40115 = CARTESIAN_POINT ( 'NONE',  ( 18.60000000122903430, -2.886751345948125991, -5.000000000000000000 ) ) ;
#40116 = CARTESIAN_POINT ( 'NONE',  ( 6.421875000614519102, 3.027376345333611329, 5.243569643749999010 ) ) ;
#40117 = CARTESIAN_POINT ( 'NONE',  ( 7.828125000614517326, -4.541064518000419881, 2.621784821874995952 ) ) ;
#40118 = CARTESIAN_POINT ( 'NONE',  ( 4.000000000000000000, 12.53749999999999964, 27.69059892324149885 ) ) ;
#40119 = CARTESIAN_POINT ( 'NONE',  ( 23.19375000122902719, 5.773502691896255534, 3.535250795749688894E-16 ) ) ;
#40120 = CARTESIAN_POINT ( 'NONE',  ( 18.57187500061451857, 3.027376345333611329, 5.243569643749999010 ) ) ;
#40121 = CARTESIAN_POINT ( 'NONE',  ( 45.00000000000000000, -6.363961030678960462, -6.363961030678893849 ) ) ;
#40122 = ORIENTED_EDGE ( 'NONE', *, *, #55670, .T. ) ;
#40123 = CARTESIAN_POINT ( 'NONE',  ( 25.45312500061451644, -4.541064518000417216, -2.621784821875001281 ) ) ;
#40124 = CARTESIAN_POINT ( 'NONE',  ( 13.30312500061451786, -4.541064518000417216, -2.621784821875001281 ) ) ;
#40125 = EDGE_CURVE ( 'NONE', #72689, #40370, #15186, .T. ) ;
#40126 = CARTESIAN_POINT ( 'NONE',  ( 27.75937500061451502, -4.541064518000417216, -2.621784821875001281 ) ) ;
#40127 = CARTESIAN_POINT ( 'NONE',  ( 10.11562500061451608, -6.054752690667223547, -1.112240025338166033E-15 ) ) ;
#40128 = CARTESIAN_POINT ( 'NONE',  ( 28.87499999999999645, 6.123233995736764310E-16, -4.999999999999998224 ) ) ;
#40129 = CARTESIAN_POINT ( 'NONE',  ( 13.83750000122903323, 4.330127018922191873, 2.499999999999999556 ) ) ;
#40130 = CARTESIAN_POINT ( 'NONE',  ( 26.50312500061451360, 4.541064518000418104, -2.621784821874998173 ) ) ;
#40131 = CARTESIAN_POINT ( 'NONE',  ( 2.121784821874999061, 12.45312500061451821, -33.67503911421598417 ) ) ;
#40132 = CARTESIAN_POINT ( 'NONE',  ( 14.32500000122903394, 2.886751345948126879, 4.999999999999999112 ) ) ;
#40133 = CARTESIAN_POINT ( 'NONE',  ( 11.96250000000000213, 2.886751345948126879, 4.999999999999999112 ) ) ;
#40134 = CARTESIAN_POINT ( 'NONE',  ( 20.50312500061451715, -4.541064518000417216, -2.621784821875001281 ) ) ;
#40135 = CARTESIAN_POINT ( 'NONE',  ( 7.434375000614519280, -4.541064518000419881, 2.621784821874995952 ) ) ;
#40136 = CARTESIAN_POINT ( 'NONE',  ( 8.587500001229035007, -4.330127018922194537, 2.499999999999995559 ) ) ;
#40137 = CARTESIAN_POINT ( 'NONE',  ( 16.05000000122903359, 5.773502691896255534, 3.535250795749688894E-16 ) ) ;
#40138 = CARTESIAN_POINT ( 'NONE',  ( 13.67812500061451786, -4.541064518000419881, 2.621784821874995952 ) ) ;
#40139 = CARTESIAN_POINT ( 'NONE',  ( 14.91562500061451679, 3.027376345333611329, 5.243569643749999010 ) ) ;
#40140 = CARTESIAN_POINT ( 'NONE',  ( 24.67500000122903359, 2.886751345948126879, 4.999999999999999112 ) ) ;
#40141 = CARTESIAN_POINT ( 'NONE',  ( 19.83750000000000213, -2.886751345948125991, -5.000000000000000000 ) ) ;
#40142 = CARTESIAN_POINT ( 'NONE',  ( 23.82187500061451502, 3.027376345333613106, -5.243569643749998122 ) ) ;
#40143 = LINE ( 'NONE', #44240, #30003 ) ;
#40144 = CARTESIAN_POINT ( 'NONE',  ( 9.187500001229034652, 6.123233995736764310E-16, -4.999999999999998224 ) ) ;
#40145 = CARTESIAN_POINT ( 'NONE',  ( 10.05937500061451750, 0.000000000000000000, 5.243569643749999010 ) ) ;
#40146 = CARTESIAN_POINT ( 'NONE',  ( 28.65937500061451715, -4.541064518000417216, -2.621784821875001281 ) ) ;
#40147 = CARTESIAN_POINT ( 'NONE',  ( 4.211141394161732165, -2.695746283285643141, -4.240727999807930360 ) ) ;
#40148 = CARTESIAN_POINT ( 'NONE',  ( 23.35312500061451857, 4.541064518000418104, -2.621784821874998173 ) ) ;
#40149 = CARTESIAN_POINT ( 'NONE',  ( 3.756430356249998770, 15.41562499938548392, 32.16877607737301759 ) ) ;
#40150 = CARTESIAN_POINT ( 'NONE',  ( 7.875000000000000000, 4.330127018922191873, 2.499999999999999556 ) ) ;
#40151 = CARTESIAN_POINT ( 'NONE',  ( 7.734375000614517326, 4.541064518000418104, 2.621784821874999949 ) ) ;
#40152 = DIRECTION ( 'NONE',  ( 1.000000000000000000, -0.000000000000000000, -0.000000000000000000 ) ) ;
#40153 = CARTESIAN_POINT ( 'NONE',  ( 26.39062500061451644, -3.027376345333610441, -5.243569643749999898 ) ) ;
#40154 = CARTESIAN_POINT ( 'NONE',  ( 6.571875000614517681, -6.054752690667223547, -1.112240025338166033E-15 ) ) ;
#40155 = CARTESIAN_POINT ( 'NONE',  ( -3.999999999999999112, 16.47500000122903430, -32.30940107675850470 ) ) ;
#40156 = CARTESIAN_POINT ( 'NONE',  ( 26.70937500061451431, 0.000000000000000000, 5.243569643749999010 ) ) ;
#40157 = CARTESIAN_POINT ( 'NONE',  ( 2.121784821875001281, 10.50312500061459353, 33.67503911421598417 ) ) ;
#40158 = CARTESIAN_POINT ( 'NONE',  ( 20.17499999999999716, -4.330127018922194537, 2.499999999999995559 ) ) ;
#40159 = ORIENTED_EDGE ( 'NONE', *, *, #6614, .F. ) ;
#40160 = CARTESIAN_POINT ( 'NONE',  ( 26.47499999999999787, -4.330127018922194537, 2.499999999999995559 ) ) ;
#40161 = ADVANCED_FACE ( 'NONE', ( #52533 ), #35470, .T. ) ;
#40162 = CARTESIAN_POINT ( 'NONE',  ( 27.49687500061451217, 6.054752690667223547, 3.707466751127219781E-16 ) ) ;
#40163 = ORIENTED_EDGE ( 'NONE', *, *, #38317, .F. ) ;
#40164 = CARTESIAN_POINT ( 'NONE',  ( 15.40312500061451573, 0.000000000000000000, 5.243569643749999010 ) ) ;
#40165 = CARTESIAN_POINT ( 'NONE',  ( 5.803125000614517859, 4.541064518000418104, -2.621784821874998173 ) ) ;
#40166 = CARTESIAN_POINT ( 'NONE',  ( 19.09687500061451360, -4.119189519843965641, -2.378215178125001383 ) ) ;
#40167 = CARTESIAN_POINT ( 'NONE',  ( 3.946875000614517681, -3.027376345333610441, -5.243569643749999898 ) ) ;
#40168 = CARTESIAN_POINT ( 'NONE',  ( 14.92500000122903181, -5.773502691896255534, -1.060575238724906372E-15 ) ) ;
#40169 = CARTESIAN_POINT ( 'NONE',  ( 21.89999999999999858, 0.000000000000000000, 4.999999999999998224 ) ) ;
#40170 = CARTESIAN_POINT ( 'NONE',  ( 28.91250000000000497, 2.886751345948129099, -4.999999999999998224 ) ) ;
#40171 = CARTESIAN_POINT ( 'NONE',  ( 3.459375000614519635, -4.541064518000417216, -2.621784821875001281 ) ) ;
#40172 = CARTESIAN_POINT ( 'NONE',  ( 8.371875000614515727, -6.054752690667223547, -1.112240025338166033E-15 ) ) ;
#40173 = CARTESIAN_POINT ( 'NONE',  ( 21.27187500061451786, 3.027376345333611329, 5.243569643749999010 ) ) ;
#40174 = CARTESIAN_POINT ( 'NONE',  ( -1.071796769724488563, 15.25490381179670152, -26.00000000000000000 ) ) ;
#40175 = ORIENTED_EDGE ( 'NONE', *, *, #4248, .F. ) ;
#40176 = CARTESIAN_POINT ( 'NONE',  ( 3.159375000614518036, 4.541064518000418104, -2.621784821874998173 ) ) ;
#40177 = CARTESIAN_POINT ( 'NONE',  ( 6.834375000614518747, 4.541064518000418104, 2.621784821874999949 ) ) ;
#40178 = CARTESIAN_POINT ( 'NONE',  ( 18.48750000000000071, -2.886751345948125991, -5.000000000000000000 ) ) ;
#40179 = CARTESIAN_POINT ( 'NONE',  ( 17.20312500061451644, 0.000000000000000000, 5.243569643749999010 ) ) ;
#40180 = CARTESIAN_POINT ( 'NONE',  ( 2.828200636599751609E-16, 19.36250000000000426, 25.38119784648299415 ) ) ;
#40181 = CARTESIAN_POINT ( 'NONE',  ( 24.71250000122903145, 0.000000000000000000, 4.999999999999998224 ) ) ;
#40182 = CARTESIAN_POINT ( 'NONE',  ( 18.90937500061451360, 4.119189519843966529, -2.378215178124998275 ) ) ;
#40183 = CARTESIAN_POINT ( 'NONE',  ( 10.07812500061451644, -4.541064518000419881, 2.621784821874995952 ) ) ;
#40184 = CARTESIAN_POINT ( 'NONE',  ( 26.78437500061451360, -4.541064518000419881, 2.621784821874995952 ) ) ;
#40185 = CARTESIAN_POINT ( 'NONE',  ( -5.810221930991193690E-16, 13.25000000122903465, 26.00000000000000355 ) ) ;
#40186 = CARTESIAN_POINT ( 'NONE',  ( 26.14687500061451431, 6.054752690667223547, 3.707466751127219781E-16 ) ) ;
#40187 = CARTESIAN_POINT ( 'NONE',  ( 6.899999999999999467, 4.330127018922192761, -2.499999999999997780 ) ) ;
#40188 = CARTESIAN_POINT ( 'NONE',  ( 4.000000000000000000, 13.10000000122903430, 32.30940107675849049 ) ) ;
#40189 = CARTESIAN_POINT ( 'NONE',  ( 5.587500001229033231, 6.123233995736764310E-16, -4.999999999999998224 ) ) ;
#40190 = CARTESIAN_POINT ( 'NONE',  ( 19.43437500061451928, 4.541064518000418104, 2.621784821874999949 ) ) ;
#40191 = CARTESIAN_POINT ( 'NONE',  ( 10.65937500061451715, -4.541064518000417216, -2.621784821875001281 ) ) ;
#40192 = CYLINDRICAL_SURFACE ( 'NONE', #59570, 4.999999999999998224 ) ;
#40193 = ORIENTED_EDGE ( 'NONE', *, *, #55155, .F. ) ;
#40194 = CARTESIAN_POINT ( 'NONE',  ( 15.10312500061451502, -4.541064518000417216, -2.621784821875001281 ) ) ;
#40195 = CARTESIAN_POINT ( 'NONE',  ( 26.96250000122903145, 0.000000000000000000, 4.999999999999998224 ) ) ;
#40196 = CARTESIAN_POINT ( 'NONE',  ( 13.13437500061451857, 4.541064518000418104, 2.621784821874999949 ) ) ;
#40197 = CARTESIAN_POINT ( 'NONE',  ( 0.4082266053725470134, 9.993705886960393414, -35.98952669105264590 ) ) ;
#40198 = CARTESIAN_POINT ( 'NONE',  ( 13.86562500061451431, 3.027376345333613106, -5.243569643749998122 ) ) ;
#40199 = CARTESIAN_POINT ( 'NONE',  ( 2.000000000000001332, 18.80000000000000071, -26.53589838486224650 ) ) ;
#40200 = CARTESIAN_POINT ( 'NONE',  ( 26.52187500061451431, 3.027376345333613106, -5.243569643749998122 ) ) ;
#40201 = CARTESIAN_POINT ( 'NONE',  ( 2.898640642222699348, -4.074056819411355335, 3.301080373617285790 ) ) ;
#40202 = CARTESIAN_POINT ( 'NONE',  ( 12.00000000122903465, 5.773502691896255534, 3.535250795749688894E-16 ) ) ;
#40203 = CARTESIAN_POINT ( 'NONE',  ( 30.00000000000000000, 0.000000000000000000, 0.000000000000000000 ) ) ;
#40204 = CARTESIAN_POINT ( 'NONE',  ( 9.001249775931846008E-16, 16.82187500061451857, -25.09994784771203058 ) ) ;
#40205 = CARTESIAN_POINT ( 'NONE',  ( 17.70937500061451431, 0.000000000000000000, 5.243569643749999010 ) ) ;
#40206 = CARTESIAN_POINT ( 'NONE',  ( 19.46250000122903145, -4.330127018922190985, -2.500000000000001332 ) ) ;
#40207 = CARTESIAN_POINT ( 'NONE',  ( 14.85937500061451644, 4.541064518000418104, -2.621784821874998173 ) ) ;
#40208 = CARTESIAN_POINT ( 'NONE',  ( -2.121784821874996840, 19.42812500061451786, -26.32496088578401583 ) ) ;
#40209 = CARTESIAN_POINT ( 'NONE',  ( 23.32500000122903572, 2.886751345948126879, 4.999999999999999112 ) ) ;
#40210 = CARTESIAN_POINT ( 'NONE',  ( 15.81562500061451537, 3.027376345333611329, 5.243569643749999010 ) ) ;
#40211 = CARTESIAN_POINT ( 'NONE',  ( 29.05312500061451431, -4.541064518000417216, -2.621784821875001281 ) ) ;
#40212 = ORIENTED_EDGE ( 'NONE', *, *, #40242, .T. ) ;
#40213 = VERTEX_POINT ( 'NONE', #49493 ) ;
#40214 = CARTESIAN_POINT ( 'NONE',  ( 17.73750000000000071, 5.773502691896255534, 3.535250795749688894E-16 ) ) ;
#40215 = CARTESIAN_POINT ( 'NONE',  ( -1.626862140677534273E-15, 18.18124999877096215, 34.00000000000000000 ) ) ;
#40216 = CARTESIAN_POINT ( 'NONE',  ( 3.202568429182106602, 3.863133281671068620, 32.44766922691853495 ) ) ;
#40217 = EDGE_CURVE ( 'NONE', #50573, #15973, #10880, .T. ) ;
#40218 = CARTESIAN_POINT ( 'NONE',  ( 15.07500000122903394, 2.886751345948129099, -4.999999999999998224 ) ) ;
#40219 = CARTESIAN_POINT ( 'NONE',  ( 19.79062500061451502, 6.054752690667223547, 3.707466751127219781E-16 ) ) ;
#40220 = CARTESIAN_POINT ( 'NONE',  ( 23.16562500061451502, -6.054752690667223547, -1.112240025338166033E-15 ) ) ;
#40221 = CARTESIAN_POINT ( 'NONE',  ( 4.453125000614517326, 4.541064518000418104, -2.621784821874998173 ) ) ;
#40222 = CARTESIAN_POINT ( 'NONE',  ( 27.71250000000000568, 2.886751345948126879, 4.999999999999999112 ) ) ;
#40223 = CARTESIAN_POINT ( 'NONE',  ( 1.071796769724489895, 11.87990381179669974, 26.00000000000000355 ) ) ;
#40224 = CARTESIAN_POINT ( 'NONE',  ( 8.334375000614516082, -4.119189519843968306, 2.378215178124996054 ) ) ;
#40225 = LINE ( 'NONE', #6965, #37068 ) ;
#40226 = CARTESIAN_POINT ( 'NONE',  ( -3.999999999999999556, 10.17500000122903359, -32.30940107675850470 ) ) ;
#40227 = CARTESIAN_POINT ( 'NONE',  ( 4.243569643749999010, 15.17187500061451644, -32.45002607614398471 ) ) ;
#40228 = CARTESIAN_POINT ( 'NONE',  ( 5.587500001229033231, 6.123233995736764310E-16, -4.999999999999998224 ) ) ;
#40229 = CARTESIAN_POINT ( 'NONE',  ( 7.462500000000001243, 2.886751345948126879, 4.999999999999999112 ) ) ;
#40230 = CARTESIAN_POINT ( 'NONE',  ( 4.875000001229034652, 2.886751345948126879, 4.999999999999999112 ) ) ;
#40231 = CARTESIAN_POINT ( 'NONE',  ( 10.20937500061451786, -4.541064518000417216, -2.621784821875001281 ) ) ;
#40232 = CARTESIAN_POINT ( 'NONE',  ( 23.73750000122903359, 4.330127018922191873, 2.499999999999999556 ) ) ;
#40233 = CARTESIAN_POINT ( 'NONE',  ( 1.626862140677534470E-15, 13.28750000000000142, 34.00000000000000000 ) ) ;
#40234 = CARTESIAN_POINT ( 'NONE',  ( 29.62500000122903288, 2.886751345948126879, 4.999999999999998224 ) ) ;
#40235 = CARTESIAN_POINT ( 'NONE',  ( 8.034375000614518925, 6.421520780324663323E-16, -5.243569643749999010 ) ) ;
#40236 = CARTESIAN_POINT ( 'NONE',  ( 13.88437500061451679, 6.421520780324663323E-16, -5.243569643749999010 ) ) ;
#40237 = EDGE_CURVE ( 'NONE', #29801, #8994, #43589, .T. ) ;
#40238 = CARTESIAN_POINT ( 'NONE',  ( 5.737499999999998934, -2.886751345948129988, 4.999999999999997335 ) ) ;
#40239 = CARTESIAN_POINT ( 'NONE',  ( -2.121784821874996840, 16.27812500061459744, 33.67503911421598417 ) ) ;
#40240 = CARTESIAN_POINT ( 'NONE',  ( 21.12187500061451573, 3.027376345333613106, -5.243569643749998122 ) ) ;
#40241 = AXIS2_PLACEMENT_3D ( 'NONE', #40252, #62773, #23968 ) ;
#40242 = EDGE_CURVE ( 'NONE', #31518, #44291, #43480, .T. ) ;
#40243 =( BOUNDED_CURVE ( )  B_SPLINE_CURVE ( 3, ( #3837, #27463, #26732, #60321 ),
 .UNSPECIFIED., .F., .F. ) 
 B_SPLINE_CURVE_WITH_KNOTS ( ( 4, 4 ),
 ( 0.6957555874851240052, 0.7294133852515908290 ),
 .UNSPECIFIED. ) 
 CURVE ( )  GEOMETRIC_REPRESENTATION_ITEM ( )  RATIONAL_B_SPLINE_CURVE ( ( 1.000000000000000000, 0.9999055982821311028, 0.9999055982821311028, 1.000000000000000000 ) ) 
 REPRESENTATION_ITEM ( '' )  );
#40244 = CARTESIAN_POINT ( 'NONE',  ( 26.47500000122903074, 2.886751345948126879, 4.999999999999999112 ) ) ;
#40245 = CARTESIAN_POINT ( 'NONE',  ( 17.10937500061451644, 2.746126346562643317, 4.756430356249998326 ) ) ;
#40246 = CARTESIAN_POINT ( 'NONE',  ( 22.04062500061451502, 6.054752690667223547, 3.707466751127219781E-16 ) ) ;
#40247 = CARTESIAN_POINT ( 'NONE',  ( 16.60312500061451857, 4.541064518000418104, -2.621784821874998173 ) ) ;
#40248 = CARTESIAN_POINT ( 'NONE',  ( 27.34687500061451360, 4.119189519843966529, -2.378215178124998275 ) ) ;
#40249 = CARTESIAN_POINT ( 'NONE',  ( 12.72187500061451537, 3.027376345333611329, 5.243569643749999010 ) ) ;
#40250 = CARTESIAN_POINT ( 'NONE',  ( 29.55000000000000071, 0.000000000000000000, 4.999999999999998224 ) ) ;
#40251 = CARTESIAN_POINT ( 'NONE',  ( 25.16250000122903074, 0.000000000000000000, 4.999999999999998224 ) ) ;
#40252 = CARTESIAN_POINT ( 'NONE',  ( 0.000000000000000000, 20.00000000000000000, 30.00000000000000000 ) ) ;
#40253 = CARTESIAN_POINT ( 'NONE',  ( 12.79687500061451821, -3.027376345333614438, 5.243569643749998122 ) ) ;
#40254 = CARTESIAN_POINT ( 'NONE',  ( 28.28437500061451715, 6.421520780324663323E-16, -5.243569643749999010 ) ) ;
#40255 = CARTESIAN_POINT ( 'NONE',  ( 4.898587196589411843E-16, 20.00000000000000000, 33.99999999999999289 ) ) ;
#40256 = CARTESIAN_POINT ( 'NONE',  ( 11.88750000122903216, 6.123233995736764310E-16, -4.999999999999998224 ) ) ;
#40257 = CARTESIAN_POINT ( 'NONE',  ( 21.53437500061451715, 6.421520780324663323E-16, -5.243569643749999010 ) ) ;
#40258 = CARTESIAN_POINT ( 'NONE',  ( 13.58437500061451786, 4.541064518000418104, 2.621784821874999949 ) ) ;
#40259 = CARTESIAN_POINT ( 'NONE',  ( -7.967954043666661671E-16, 17.59062499938548285, 34.33755215474603517 ) ) ;
#40260 = CARTESIAN_POINT ( 'NONE',  ( 26.81250000000000000, 2.886751345948126879, 4.999999999999999112 ) ) ;
#40261 = CARTESIAN_POINT ( 'NONE',  ( -4.000000000000000000, 13.17500000000000071, 30.00000000000000000 ) ) ;
#40262 = CARTESIAN_POINT ( 'NONE',  ( 26.07187500061451857, 2.746126346562645981, -4.756430356249997438 ) ) ;
#40263 = CARTESIAN_POINT ( 'NONE',  ( 16.97812500061451502, 6.421520780324663323E-16, -5.243569643749999010 ) ) ;
#40264 = CARTESIAN_POINT ( 'NONE',  ( 5.850000000000001421, -4.330127018922190985, -2.500000000000001332 ) ) ;
#40265 = CARTESIAN_POINT ( 'NONE',  ( 4.000000000000000000, 13.55000000122903359, 32.30940107675849760 ) ) ;
#40266 = CARTESIAN_POINT ( 'NONE',  ( 17.84999999999999787, 0.000000000000000000, 4.999999999999998224 ) ) ;
#40267 = CARTESIAN_POINT ( 'NONE',  ( 4.243569643749999898, 11.47812500061451679, 30.00000000000000000 ) ) ;
#40268 = CARTESIAN_POINT ( 'NONE',  ( 24.65625000122903288, 0.000000000000000000, 4.999999999999998224 ) ) ;
#40269 = CARTESIAN_POINT ( 'NONE',  ( 26.97187500061451360, 3.027376345333613106, -5.243569643749998122 ) ) ;
#40270 = ORIENTED_EDGE ( 'NONE', *, *, #45929, .T. ) ;
#40271 = CARTESIAN_POINT ( 'NONE',  ( 20.84062500061451573, -3.027376345333614438, 5.243569643749998122 ) ) ;
#40272 = CARTESIAN_POINT ( 'NONE',  ( 21.15937500061451715, 4.541064518000418104, -2.621784821874998173 ) ) ;
#40273 = CARTESIAN_POINT ( 'NONE',  ( 4.500000000000000888, -4.330127018922190985, -2.500000000000001332 ) ) ;
#40274 = CARTESIAN_POINT ( 'NONE',  ( 8.015625000614518214, 3.027376345333613106, -5.243569643749998122 ) ) ;
#40275 = CARTESIAN_POINT ( 'NONE',  ( 23.87812500061451715, 4.541064518000418104, 2.621784821874999949 ) ) ;
#40276 = CARTESIAN_POINT ( 'NONE',  ( 12.87187500061451750, -6.054752690667223547, -1.112240025338166033E-15 ) ) ;
#40277 = CARTESIAN_POINT ( 'NONE',  ( 17.48437500061451999, 6.421520780324663323E-16, -5.243569643749999010 ) ) ;
#40278 = CARTESIAN_POINT ( 'NONE',  ( -4.243569643749999898, 18.41562500061451857, 27.54997392385601529 ) ) ;
#40279 = CARTESIAN_POINT ( 'NONE',  ( 19.61250000122903359, 4.330127018922192761, -2.499999999999997780 ) ) ;
#40280 = CARTESIAN_POINT ( 'NONE',  ( 14.67187500061451821, -5.492252693125287522, -1.008910452111647106E-15 ) ) ;
#40281 = CARTESIAN_POINT ( 'NONE',  ( 9.253125000614517148, -4.541064518000417216, -2.621784821875001281 ) ) ;
#40282 = CARTESIAN_POINT ( 'NONE',  ( 5.371875000614516615, 3.027376345333613106, -5.243569643749998122 ) ) ;
#40283 = CARTESIAN_POINT ( 'NONE',  ( 4.621875000614516615, 3.027376345333611329, 5.243569643749999010 ) ) ;
#40284 = ORIENTED_EDGE ( 'NONE', *, *, #45137, .F. ) ;
#40285 = CARTESIAN_POINT ( 'NONE',  ( 24.19687500061451857, -3.027376345333610441, -5.243569643749999898 ) ) ;
#40286 = CARTESIAN_POINT ( 'NONE',  ( 15.74062500061451608, 6.054752690667223547, 3.707466751127219781E-16 ) ) ;
#40287 = CARTESIAN_POINT ( 'NONE',  ( 26.73750000122903003, 6.123233995736764310E-16, -4.999999999999998224 ) ) ;
#40288 = CARTESIAN_POINT ( 'NONE',  ( 27.40312500061451573, 4.541064518000418104, -2.621784821874998173 ) ) ;
#40289 = CARTESIAN_POINT ( 'NONE',  ( 22.09687500061451715, 6.054752690667223547, 3.707466751127219781E-16 ) ) ;
#40290 = CARTESIAN_POINT ( 'NONE',  ( 18.25312500061451715, -4.541064518000417216, -2.621784821875001281 ) ) ;
#40291 = CARTESIAN_POINT ( 'NONE',  ( -4.243569643749999898, 17.12187500061451573, 27.54997392385601529 ) ) ;
#40292 = CARTESIAN_POINT ( 'NONE',  ( 22.49062500061451431, 6.054752690667223547, 3.707466751127219781E-16 ) ) ;
#40293 = CARTESIAN_POINT ( 'NONE',  ( 3.037500001229032964, 4.330127018922191873, 2.499999999999999556 ) ) ;
#40294 = VERTEX_POINT ( 'NONE', #22136 ) ;
#40295 = CARTESIAN_POINT ( 'NONE',  ( 28.16249999999999787, 2.886751345948126879, 4.999999999999999112 ) ) ;
#40296 = CARTESIAN_POINT ( 'NONE',  ( -3.999999999999997335, 14.18750000000000000, -27.69059892324149175 ) ) ;
#40297 = CARTESIAN_POINT ( 'NONE',  ( 3.756430356249998770, 19.01562499938548356, 32.16877607737302469 ) ) ;
#40298 = CARTESIAN_POINT ( 'NONE',  ( 3.271875000614519635, 3.027376345333611329, 5.243569643749999010 ) ) ;
#40299 = CARTESIAN_POINT ( 'NONE',  ( 11.12812500061451715, 6.421520780324663323E-16, -5.243569643749999010 ) ) ;
#40300 = CARTESIAN_POINT ( 'NONE',  ( 22.46250000122903501, 0.000000000000000000, 4.999999999999998224 ) ) ;
#40301 = CARTESIAN_POINT ( 'NONE',  ( 26.91562500061451146, 3.027376345333613106, -5.243569643749998122 ) ) ;
#40302 = CARTESIAN_POINT ( 'NONE',  ( 27.48749999999999716, -2.886751345948125991, -5.000000000000000000 ) ) ;
#40303 = CARTESIAN_POINT ( 'NONE',  ( 8.484601909799253346E-16, 17.52500000122903501, -25.38119784648299770 ) ) ;
#40304 = CARTESIAN_POINT ( 'NONE',  ( -3.999999999999997335, 15.65000000122903501, -27.69059892324149530 ) ) ;
#40305 = CARTESIAN_POINT ( 'NONE',  ( 9.740625000614516082, -3.027376345333610441, -5.243569643749999898 ) ) ;
#40306 = ORIENTED_EDGE ( 'NONE', *, *, #34124, .T. ) ;
#40307 = CARTESIAN_POINT ( 'NONE',  ( 8.165625000614516793, 3.027376345333611329, 5.243569643749999010 ) ) ;
#40308 = CARTESIAN_POINT ( 'NONE',  ( 5.128125000614516260, -4.541064518000419881, 2.621784821874995952 ) ) ;
#40309 = CARTESIAN_POINT ( 'NONE',  ( 16.77187500061451786, 2.746126346562643317, 4.756430356249998326 ) ) ;
#40310 = CARTESIAN_POINT ( 'NONE',  ( 4.898587196589411843E-16, 20.00000000000000000, 33.99999999999999289 ) ) ;
#40311 = CARTESIAN_POINT ( 'NONE',  ( 14.58750000000000036, 5.773502691896255534, 3.535250795749688894E-16 ) ) ;
#40312 = CARTESIAN_POINT ( 'NONE',  ( 16.62187500061451573, 3.027376345333613106, -5.243569643749998122 ) ) ;
#40313 = CARTESIAN_POINT ( 'NONE',  ( 11.77500000122903501, -5.773502691896255534, -1.060575238724906372E-15 ) ) ;
#40314 = EDGE_CURVE ( 'NONE', #50439, #6778, #65671, .T. ) ;
#40315 = CARTESIAN_POINT ( 'NONE',  ( 19.09687500061451360, -3.027376345333614438, 5.243569643749998122 ) ) ;
#40316 = CARTESIAN_POINT ( 'NONE',  ( 16.31250000000000000, 2.886751345948129099, -4.999999999999998224 ) ) ;
#40317 = CARTESIAN_POINT ( 'NONE',  ( 20.48437500061451289, -4.541064518000419881, 2.621784821874995952 ) ) ;
#40318 = CARTESIAN_POINT ( 'NONE',  ( -4.243569643749997233, 14.44062500061451715, -27.54997392385601174 ) ) ;
#40319 = CARTESIAN_POINT ( 'NONE',  ( 29.80312500061451431, 0.000000000000000000, 4.999999999999998224 ) ) ;
#40320 = CARTESIAN_POINT ( 'NONE',  ( 26.22187500061451360, -4.119189519843968306, 2.378215178124996054 ) ) ;
#40321 = CARTESIAN_POINT ( 'NONE',  ( 4.148109664150280373, 2.791627878887652514, 4.438675071986421194 ) ) ;
#40322 = CARTESIAN_POINT ( 'NONE',  ( 26.87812500061451360, 6.421520780324663323E-16, -5.243569643749999010 ) ) ;
#40323 = CARTESIAN_POINT ( 'NONE',  ( 5.325000001229032165, 2.886751345948193936, 4.999999999999883649 ) ) ;
#40324 = CARTESIAN_POINT ( 'NONE',  ( 29.55937500061451573, -4.541064518000417216, -2.621784821875001281 ) ) ;
#40325 = CARTESIAN_POINT ( 'NONE',  ( 24.52499999999999858, 4.330127018922191873, 2.499999999999999556 ) ) ;
#40326 = EDGE_CURVE ( 'NONE', #8225, #9764, #68058, .T. ) ;
#40327 = CARTESIAN_POINT ( 'NONE',  ( 7.490625000614516082, -3.027376345333610441, -5.243569643749999898 ) ) ;
#40328 = CARTESIAN_POINT ( 'NONE',  ( 25.69687500061451502, 0.000000000000000000, 4.756430356249998326 ) ) ;
#40329 = CARTESIAN_POINT ( 'NONE',  ( 19.80937500061451573, 4.541064518000418104, -2.621784821874998173 ) ) ;
#40330 = CARTESIAN_POINT ( 'NONE',  ( 11.97187500061451537, 5.824947211148865298E-16, -4.756430356249998326 ) ) ;
#40331 = CARTESIAN_POINT ( 'NONE',  ( 4.753125000614515372, -4.541064518000417216, -2.621784821875001281 ) ) ;
#40332 = CARTESIAN_POINT ( 'NONE',  ( 8.709375000614517859, 0.000000000000000000, 5.243569643749999010 ) ) ;
#40333 = VERTEX_POINT ( 'NONE', #45767 ) ;
#40334 = CARTESIAN_POINT ( 'NONE',  ( 18.75937500061451857, -4.541064518000417216, -2.621784821875001281 ) ) ;
#40335 = CARTESIAN_POINT ( 'NONE',  ( 28.23750000000000426, -2.886751345948129988, 4.999999999999997335 ) ) ;
#40336 = CARTESIAN_POINT ( 'NONE',  ( 3.562500000000000444, -5.773502691896255534, -1.060575238724906372E-15 ) ) ;
#40337 = CARTESIAN_POINT ( 'NONE',  ( 2.000000000000001332, 10.25000000000000000, -26.53589838486224650 ) ) ;
#40338 = CARTESIAN_POINT ( 'NONE',  ( 16.01249999999999929, 2.886751345948126879, 4.999999999999998224 ) ) ;
#40339 = EDGE_LOOP ( 'NONE', ( #14388, #65305, #50159, #33786 ) ) ;
#40340 = CARTESIAN_POINT ( 'NONE',  ( 10.91250000000000320, 2.886751345948129099, -4.999999999999998224 ) ) ;
#40341 = CARTESIAN_POINT ( 'NONE',  ( 12.15937500061451360, 2.746126346562643317, 4.756430356249998326 ) ) ;
#40342 = CARTESIAN_POINT ( 'NONE',  ( 25.07812500061451644, 6.421520780324663323E-16, -5.243569643749999010 ) ) ;
#40343 = CARTESIAN_POINT ( 'NONE',  ( 13.83749999999999858, -2.886751345948129988, 4.999999999999997335 ) ) ;
#40344 = EDGE_CURVE ( 'NONE', #27030, #22784, #52390, .T. ) ;
#40345 = CARTESIAN_POINT ( 'NONE',  ( 10.01250000122903394, -4.330127018922190985, -2.500000000000001332 ) ) ;
#40346 = CARTESIAN_POINT ( 'NONE',  ( 9.290625000614515017, -3.027376345333610441, -5.243569643749999898 ) ) ;
#40347 = CARTESIAN_POINT ( 'NONE',  ( 24.03750000000000142, 5.773502691896255534, 3.535250795749688894E-16 ) ) ;
#40348 = CARTESIAN_POINT ( 'NONE',  ( 21.36562500061451431, -6.054752690667223547, -1.112240025338166033E-15 ) ) ;
#40349 = CARTESIAN_POINT ( 'NONE',  ( 0.000000000000000000, 20.00000000000000000, -30.00000000000000000 ) ) ;
#40350 = AXIS2_PLACEMENT_3D ( 'NONE', #41563, #47835, #20469 ) ;
#40351 = CARTESIAN_POINT ( 'NONE',  ( 28.16250000122903074, 4.330127018922192761, -2.499999999999997780 ) ) ;
#40352 = CARTESIAN_POINT ( 'NONE',  ( 3.756430356250000102, 17.14062499938548356, 30.00000000000000000 ) ) ;
#40353 = CARTESIAN_POINT ( 'NONE',  ( 6.600000000000001421, 0.000000000000000000, 4.999999999999998224 ) ) ;
#40354 = ORIENTED_EDGE ( 'NONE', *, *, #30402, .F. ) ;
#40355 = CARTESIAN_POINT ( 'NONE',  ( 21.06562500061451715, 3.027376345333613106, -5.243569643749998122 ) ) ;
#40356 = CARTESIAN_POINT ( 'NONE',  ( 29.05312500061451431, -4.541064518000417216, -2.621784821875001281 ) ) ;
#40357 = CYLINDRICAL_SURFACE ( 'NONE', #59647, 4.999999999999998224 ) ;
#40358 = CARTESIAN_POINT ( 'NONE',  ( 18.49687500061452283, 6.054752690667223547, 3.707466751127219781E-16 ) ) ;
#40359 = CARTESIAN_POINT ( 'NONE',  ( 13.37812500061451715, 6.421520780324663323E-16, -5.243569643749999010 ) ) ;
#40360 = CARTESIAN_POINT ( 'NONE',  ( 11.40000000000000036, 4.330127018922192761, -2.499999999999997780 ) ) ;
#40361 = CARTESIAN_POINT ( 'NONE',  ( 29.10000000122903074, 5.773502691896255534, 3.535250795749688894E-16 ) ) ;
#40362 = CARTESIAN_POINT ( 'NONE',  ( 22.95937500061451431, 4.119189519843966529, -2.378215178124998275 ) ) ;
#40363 = CARTESIAN_POINT ( 'NONE',  ( 17.09062500061451573, 6.054752690667223547, 3.707466751127219781E-16 ) ) ;
#40364 = CARTESIAN_POINT ( 'NONE',  ( 2.000000000000001332, 13.85000000000000142, 33.46410161513774995 ) ) ;
#40365 = CARTESIAN_POINT ( 'NONE',  ( 3.150000001229034119, -2.886751345948129988, 4.999999999999997335 ) ) ;
#40366 = AXIS2_PLACEMENT_3D ( 'NONE', #7424, #59111, #47673 ) ;
#40367 = CARTESIAN_POINT ( 'NONE',  ( 13.09687500061451892, 6.054752690667223547, 3.707466751127219781E-16 ) ) ;
#40368 = CARTESIAN_POINT ( 'NONE',  ( 12.53437500061451537, 6.421520780324663323E-16, -5.243569643749999010 ) ) ;
#40369 = CARTESIAN_POINT ( 'NONE',  ( 19.88437500061451857, 4.541064518000418104, 2.621784821874999949 ) ) ;
#40370 = VERTEX_POINT ( 'NONE', #68303 ) ;
#40371 = CARTESIAN_POINT ( 'NONE',  ( -5.948681673321857488, 8.038272906428572284, 29.19158024300208609 ) ) ;
#40372 = CARTESIAN_POINT ( 'NONE',  ( 24.14062500061451289, -3.027376345333610441, -5.243569643749999898 ) ) ;
#40373 = CARTESIAN_POINT ( 'NONE',  ( 19.77187500061451786, 3.027376345333613106, -5.243569643749998122 ) ) ;
#40374 = CARTESIAN_POINT ( 'NONE',  ( 24.70312500061451644, 4.541064518000418104, -2.621784821874998173 ) ) ;
#40375 = DIRECTION ( 'NONE',  ( -1.000000000000000000, -0.000000000000000000, -0.000000000000000000 ) ) ;
#40376 = CARTESIAN_POINT ( 'NONE',  ( -1.999999999999997113, 15.57500000000000284, 33.46410161513775705 ) ) ;
#40377 = CARTESIAN_POINT ( 'NONE',  ( 28.41562500061451502, 3.027376345333611329, 5.243569643749999010 ) ) ;
#40378 = CARTESIAN_POINT ( 'NONE',  ( 10.23750000122903359, 4.330127018922191873, 2.499999999999999556 ) ) ;
#40379 = CARTESIAN_POINT ( 'NONE',  ( 5.887500001229034829, -4.330127018922194537, 2.499999999999995559 ) ) ;
#40380 = CARTESIAN_POINT ( 'NONE',  ( 1.592000809091587073E-14, 17.18750000000000355, 26.00000000000000000 ) ) ;
#40381 = CARTESIAN_POINT ( 'NONE',  ( 26.58750000122903145, -4.330127018922194537, 2.499999999999995559 ) ) ;
#40382 = CARTESIAN_POINT ( 'NONE',  ( -1.999999999999999112, 17.99374999877096570, 26.53589838486224650 ) ) ;
#40383 = CARTESIAN_POINT ( 'NONE',  ( 16.70625000122903359, -4.330127018922190985, -2.500000000000001332 ) ) ;
#40384 = CARTESIAN_POINT ( 'NONE',  ( 8.596875000614518925, 6.054752690667223547, 3.707466751127219781E-16 ) ) ;
#40385 = CARTESIAN_POINT ( 'NONE',  ( -5.810221930991193690E-16, 10.10000000122903430, 26.00000000000000355 ) ) ;
#40386 = CARTESIAN_POINT ( 'NONE',  ( 18.32812500061451644, 6.421520780324663323E-16, -5.243569643749999010 ) ) ;
#40387 = CARTESIAN_POINT ( 'NONE',  ( 10.84687500061451892, 6.054752690667223547, 3.707466751127219781E-16 ) ) ;
#40388 = CARTESIAN_POINT ( 'NONE',  ( 28.53750000122903074, 6.123233995736764310E-16, -4.999999999999998224 ) ) ;
#40389 = CARTESIAN_POINT ( 'NONE',  ( 20.48437500061451289, -4.541064518000419881, 2.621784821874995952 ) ) ;
#40390 = CARTESIAN_POINT ( 'NONE',  ( 7.959375000614516971, -4.541064518000417216, -2.621784821875001281 ) ) ;
#40391 = CARTESIAN_POINT ( 'NONE',  ( 3.965625000614515727, 3.027376345333613106, -5.243569643749998122 ) ) ;
#40392 = CARTESIAN_POINT ( 'NONE',  ( 1.071796769724485232, 16.19240381056766509, 25.99999999999999645 ) ) ;
#40393 = CARTESIAN_POINT ( 'NONE',  ( 8.203125000614518214, 0.000000000000000000, 5.243569643749999010 ) ) ;
#40394 = CARTESIAN_POINT ( 'NONE',  ( 19.34062500061451573, 6.054752690667223547, 3.707466751127219781E-16 ) ) ;
#40395 = VERTEX_POINT ( 'NONE', #50942 ) ;
#40396 = CARTESIAN_POINT ( 'NONE',  ( 5.812500001229035540, 0.000000000000000000, 4.999999999999998224 ) ) ;
#40397 = CARTESIAN_POINT ( 'NONE',  ( 14.84062500061451750, 6.054752690667223547, 3.707466751127219781E-16 ) ) ;
#40398 = CARTESIAN_POINT ( 'NONE',  ( 12.92812500061451786, 6.421520780324663323E-16, -5.243569643749999010 ) ) ;
#40399 = CARTESIAN_POINT ( 'NONE',  ( 23.25937500061451857, -4.119189519843965641, -2.378215178125001383 ) ) ;
#40400 = CARTESIAN_POINT ( 'NONE',  ( 13.87500000000000178, -4.330127018922194537, 2.499999999999995559 ) ) ;
#40401 = CARTESIAN_POINT ( 'NONE',  ( 8.287500001229034297, 6.123233995736764310E-16, -4.999999999999998224 ) ) ;
#40402 = CARTESIAN_POINT ( 'NONE',  ( 4.978125000614518569, 4.541064518000418104, 2.621784821874999949 ) ) ;
#40403 =( BOUNDED_SURFACE ( )  B_SPLINE_SURFACE ( 1, 2, ( 
 ( #41813, #25925, #9666, #52902, #59157, #59895, #42916, #24815, #48465, #70989, #64343, #47719, #36277, #20365, #70258, #65439, #9301, #65811, #3766, #26291, #19630, #47361, #69893, #42186, #39566, #33647, #67291, #60996, #38845, #55465, #72819, #62091, #17009, #49199, #72447, #32927, #10395, #45107, #27391, #43654, #38097, #10029, #56191, #66922, #10757, #32199, #11118, #32564, #15553, #5585, #27031, #55102, #21466, #50297, #44756, #4502, #4857, #15922, #54733, #22560, #49923, #27756, #60619, #21832, #16290, #71732, #44396, #61360, #33289, #55827, #67643, #4135, #5215, #39205, #61719, #28122, #49562, #38472, #50650, #22202, #16649, #54, #72083, #26665, #21102, #44020, #66543, #66177, #22913, #68002, #45470, #63167, #28829, #57976, #68726, #29555, #1132, #62806, #6669, #12199, #12919, #39932, #34007, #23641, #62446, #40647, #11484, #57256, #69091, #51007, #17375, #52091, #24002, #46187, #34727, #29914, #56544, #1860, #7384, #11844, #18086, #7024, #12562, #29197, #51368, #1496, #63532, #5937, #46550, #35096, #57621, #35452, #18453, #68364, #41017, #770, #28471, #24367, #404, #51731, #52454, #56895, #23278, #45828, #6301, #46915, #69453, #18810, #41374, #34363, #17726, #40285, #59070, #25466, #25840, #54285, #2571, #25091, #42467, #19544, #37284, #20645, #48377, #7746, #3313, #14742, #70904, #31379, #48742, #47634, #8474, #65352, #59435, #41727, #48010, #31008, #53919, #20276, #24730, #2217, #70538, #53174, #47273, #42829, #2937, #42102, #59807, #19913, #64990, #14011, #71266, #14380, #70168, #30643, #64254, #30282, #36915, #53541, #36550, #9212, #13275, #8843, #52815, #31748, #69807, #3679, #63884, #35813, #64624, #26203, #58335, #19172, #13642, #36186, #58704, #8115, #54643, #49839, #4047, #4417, #44306, #11034, #61278, #66835, #66088, #50566, #22117, #5498, #73093, #44673, #5134, #72004, #72363, #66459, #10671, #43202, #28037, #60167, #10309, #43933, #21379, #56107, #38382, #26573, #49112, #21014, #67204, #4772, #21744, #65722, #16565, #43567, #71641, #39117, #38011, #15466, #32478, #33201, #55740, #60533, #15836, #26946, #15108, #33557, #60905, #38758, #9940, #32841, #37644, #49472, #9577, #55378, #55012, #27305, #16206, #27668, #32109, #50207, #72731, #61632, #52371, #17290, #22831, #51651, #7305, #28386, #34646, #50925, #22475, #18372, #40940, #63454, #12840, #322, #57897, #29836, #45383, #63086, #33922, #6945, #57174, #12120, #68284, #67919, #35014, #39852, #45025, #39478, #6587, #17645, #67560, #35374, #62365, #40566, #5855, #12487, #6218, #23194, #68645, #11762, #23921, #18008, #34279, #29117, #40205, #57543, #29476, #56464, #56811, #1052, #28746, #51285, #52013, #23562, #687, #1414, #46108, #46471, #45748, #16924, #69008, #62001, #11402, #62727, #64539, #42018, #13932, #38199, #1776, #36469, #8759, #31293, #53834, #7661, #8031, #48292, #70456, #19832, #25012, #41649, #60725, #8393, #2137, #47194, #24648, #13197, #58256, #35736, #53463, #19094, #70818, #58987, #42384, #30922, #53092, #70083, #2487, #3228, #30201, #24288, #2854, #52732, #25383, #46836, #47554, #59348, #41295, #69725, #64906, #14296, #47927, #19458, #20192, #69375, #66282, #43757, #64169, #36834, #25756, #15660, #10136, #13557, #32668, #18731, #63805, #36103, #58624, #30566, #6043, #39676, #38946, #39312, #44498, #55209, #68110, #72194, #27865, #61824, #27496, #67031, #72555, #50030, #33392, #44856, #155, #72922, #56297, #16031, #34109, #50397, #16754, #17117, #45578, #16390, #61464, #33752, #10859, #28577, #11946, #62196, #21573, #67745, #51114, #11592, #22661, #40036, #55928, #22304, #45211, #38579, #56648, #5324, #67392, #28222, #61103, #11229, #21943, #33029, #44127, #5687, #50752, #511, #23022, #4602, #17476, #66654, #62550, #10501, #27133, #49666, #55568, #4963, #69553, #24470, #34471, #35199, #18554, #23384, #29302, #45933, #41119, #68464, #68830, #35557, #2315, #52557, #58077, #57362, #41829, #13374, #69908, #64360, #35916, #18913, #63271, #63630, #57722, #1963, #56999, #19275, #51475, #1595, #7127, #12663, #47378, #29657, #17826, #40387, #12300, #58441, #69194, #13019, #6406, #7852, #34836, #62906, #30388, #51832, #6769, #23741, #47018, #41473, #1236, #52194, #18186, #28938, #24830, #24106, #30014, #46289, #46654, #877, #40756, #7485, #63993, #52917, #14481, #53648, #54386, #30745, #9317, #65455, #53277, #43671, #8580, #14111, #42931, #71748, #19646, #25940, #42202, #13750, #9681, #32214, #54748, #4150, #64726, #49215, #21118, #36650, #3781, #25192, #71374, #48480, #3420, #59539, #59172, #26306, #31109, #36292, #2676, #71004, #8949, #58806, #26682, #3041, #8216, #47736, #70275, #31483, #20380, #25572, #48112, #70635, #20010, #65090, #14848, #31850, #54025, #37387, #42563, #65827, #59911, #48844, #20749, #37015, #43307, #15209, #37749, #60267, #56207, #17024, #39222, #60635, #44771, #33663, #67306, #22217, #45123, #32942, #44411, #11135, #72834, #72100, #10772, #66937, #16664, #61734, #55119, #4518, #61375, #61012, #27047, #5600, #38860, #4872, #28137, #33305, #55843, #72463, #67658, #5231, #27772, #10047, #27408, #16306, #50312, #50665, #22575, #66194, #69, #15572, #38114, #32581, #10410, #49578, #21485, #44037, #66559, #15939, #38488, #55480, #49939, #21848, #50892, #16893, #1380, #46077, #29443, #23890, #68612, #29085, #22801, #657, #17259, #34612, #67171, #51981, #11003, #34247, #67887, #45353, #6913, #62335, #5465, #73062, #44992, #17973, #28715, #45719, #16532, #40534, #67530, #50534, #63050, #61969, #39448, #56434, #12091, #6552, #11371, #39820, #292, #39085, #57511, #11731, #62695, #22443, #56780, #61602, #6186, #33523, #51255, #33890, #56073, #23164, #28005, #5824, #28355, #12451, #68254, #17616, #40176, #34983, #57142, #51620, #1021, #23527, #24254, #35702, #64505 ),
 ( #24977, #63419, #3194, #41261, #46802, #2454, #31257, #52338, #58590, #1740, #46437, #42349, #64872, #14260, #36799, #69338, #8723, #53799, #18697, #13897, #57864, #30888, #7997, #36070, #19059, #63773, #58951, #13161, #68976, #12805, #30533, #41617, #18333, #59314, #58223, #36437, #29802, #8359, #30165, #47162, #19424, #7628, #52698, #2104, #24615, #35341, #53060, #13522, #64136, #53430, #40906, #47522, #7273, #41984, #69694, #70051, #2820, #25348, #47894, #70422, #19797, #25721, #26453, #9823, #14623, #20521, #37162, #32355, #59688, #60052, #43452, #60414, #54165, #9463, #48623, #33084, #4659, #61161, #55623, #27188, #60785, #54527, #54893, #48993, #66340, #48259, #10556, #42712, #65974, #71523, #3930, #3562, #31993, #71148, #70782, #49723, #20158, #65233, #72250, #10191, #20898, #4300, #15354, #15718, #9095, #31632, #26084, #37896, #26825, #49359, #38637, #71889, #43079, #65605, #14993, #21627, #21262, #43816, #37530, #44185, #38256, #32726, #66715, #55263, #16089, #67449, #23079, #17532, #55987, #28277, #61883, #34894, #68527, #33810, #574, #33442, #211, #72616, #11289, #12360, #50809, #5380, #5743, #44912, #45636, #21998, #68169, #56701, #44556, #5019, #72978, #27918, #34164, #62964, #10916, #17175, #50452, #27553, #936, #23444, #45990, #17888, #22360, #40448, #50085, #16811, #40094, #16446, #62608, #39735, #67802, #22716, #39367, #12004, #56353, #67087, #39003, #62252, #45269, #61518, #11649, #6101, #34527, #28632, #57057, #51170, #6464, #28999, #51536, #18615, #24166, #35257, #23802, #64052, #24533, #30078, #64420, #6827, #47077, #1292, #52977, #46353, #2022, #42261, #64784, #69253, #19338, #47436, #57423, #58138, #41533, #68887, #52254, #18244, #13432, #40817, #41180, #69612, #18973, #8276, #41893, #63689, #35982, #46718, #29361, #70332, #63333, #52616, #58501, #29716, #13079, #1657, #35618, #7544, #7910, #2373, #30448, #24891, #12721, #36352, #69967, #13813, #58866, #47803, #30806, #53339, #2737, #25254, #19709, #14175, #51894, #57778, #7188, #60695, #49273, #4211, #21543, #20440, #54445, #38171, #32272, #14539, #20811, #3844, #26739, #71806, #70694, #48170, #43366, #25999, #20069, #21175, #48904, #65521, #43728, #65889, #71435, #59968, #44098, #15270, #37809, #53710, #14907, #26365, #60329, #9738, #72163, #36709, #54805, #66252, #15630, #10108, #42625, #42989, #32638, #55178, #4574, #9376, #3481, #66624, #65149, #49636, #25632, #48538, #37075, #59599, #9011, #27104, #54083, #59231, #8639, #31168, #3103, #37448, #31909, #31543, #71065, #44470, #38550, #5661, #67000, #45184, #16001, #61794, #481, #55539, #21914, #34080, #28550, #28197, #39282, #34443, #61073, #6375, #11918, #72526, #22634, #11565, #50726, #33726, #33364, #56620, #68080, #10470, #6015, #39649, #67716, #17088, #33000, #11199, #22990, #4934, #16362, #51084, #45551, #129, #56272, #56971, #27469, #28907, #51445, #38916, #62168, #17449, #40007, #62521, #55901, #847, #23356, #50001, #45905, #61436, #10829, #5293, #27839, #72895, #50370, #22277, #44829, #67364, #16727, #41092, #1936, #40727, #57696, #12637, #63243, #46625, #58051, #13349, #12994, #69526, #29275, #47346, #63604, #29986, #30359, #58778, #7101, #29630, #46990, #24079, #41800, #25165, #52888, #12274, #7824, #19245, #2286, #35887, #53248, #52168, #35530, #69880, #63965, #46263, #52528, #7460, #58411, #24803, #51805, #6741, #24441, #1570, #1208, #64329, #18884, #69168, #13722, #41447, #36263, #18527, #2646, #8187, #30715, #34805, #68437, #17799, #40359, #62878, #57337, #23714, #68803, #18159, #35172, #54720, #53620, #53995, #21090, #43278, #65799, #70977, #14453, #32552, #31080, #60607, #36623, #36987, #59144, #3011, #8553, #26278, #65062, #43641, #31821, #15180, #37360, #25913, #42903, #48453, #49188, #25541, #70245, #59882, #48084, #14817, #4123, #26652, #71718, #70610, #3392, #66165, #37719, #60239, #20352, #59509, #55089, #19983, #10016, #42536, #8923, #31453, #65427, #9288, #48815, #54360, #15541, #3754, #9653, #71345, #20720, #32187, #38085, #4489, #47706, #19617, #42173, #64699, #14083, #27018, #72807, #11472, #66530, #32915, #45095, #39554, #16637, #50283, #45458, #49550, #17364, #22899, #10383, #33635, #22547, #61707, #44744, #44384, #67630, #5925, #21453, #16997, #50638, #56179, #50994, #33995, #10744, #11106, #16277, #72072, #39921, #44008, #22190, #5572, #72435, #38833, #66909, #21819, #5203, #39192, #62079, #67278, #28109, #60984, #28459, #42, #56532, #392, #62435, #61348, #33277, #67990, #55816, #11833, #56884, #34351, #15910, #38458, #55452, #4845, #27379, #49911, #27744, #23992, #7738, #1850, #57245, #63522, #46539, #46906, #41366, #40274, #17714, #12909, #68716, #62795, #63876, #18442, #35085, #13267, #35442, #41007, #29545, #13634, #57966, #7374, #23267, #57611, #69081, #29905, #52445, #41719, #6289, #6658, #18076, #24358, #18802, #29187, #52081, #63156, #36178, #69799, #7014, #69445, #34715, #1486, #759, #12551, #28818, #35805, #51721, #58327, #46177, #30273, #45817, #52806, #2207, #68353, #51356, #1122, #23631, #24722, #64246, #12188, #47265, #40637, #19165, #54632, #4039, #26563, #49103, #36541, #21005, #43557, #8466, #26193, #70159, #43193, #20268, #48369, #31371, #59061, #71256, #31001, #66079, #2563, #70895, #53912, #15457, #71632, #14002, #3670, #42094, #48733, #42458, #59427, #31738, #64616, #19906, #25459, #53534, #25083, #65343, #25832, #3305, #65713, #8106, #42820, #47626, #54276, #19536, #14733, #58695, #30634, #70531, #20636, #15099, #53166, #8835, #37275, #2930, #48003, #64981, #59797, #14372, #36907, #9203, #37635, #60158, #9568, #32100, #45374, #16914, #312, #67910, #39469, #73084, #66824, #44664, #61268, #5489, #38002, #22822, #55002, #5125, #38748, #16197, #50914, #33192, #49462, #43924 ) ),
 .UNSPECIFIED., .F., .F., .F. ) 
 B_SPLINE_SURFACE_WITH_KNOTS ( ( 2, 2 ),
 ( 3, 2, 2, 2, 2, 2, 2, 2, 2, 2, 2, 2, 2, 2, 2, 2, 2, 2, 2, 2, 2, 2, 2, 2, 2, 2, 2, 2, 2, 2, 2, 2, 2, 2, 2, 2, 2, 2, 2, 2, 2, 2, 2, 2, 2, 2, 2, 2, 2, 2, 2, 2, 2, 2, 2, 2, 2, 2, 2, 2, 2, 2, 2, 2, 2, 2, 2, 2, 2, 2, 2, 2, 2, 2, 2, 2, 2, 2, 2, 2, 2, 2, 2, 2, 2, 2, 2, 2, 2, 2, 2, 2, 2, 2, 2, 2, 2, 2, 2, 2, 2, 2, 2, 2, 2, 2, 2, 2, 2, 2, 2, 2, 2, 2, 2, 2, 2, 2, 2, 2, 2, 2, 2, 2, 2, 2, 2, 2, 2, 2, 2, 2, 2, 2, 2, 2, 2, 2, 2, 2, 2, 2, 2, 2, 2, 2, 2, 2, 2, 2, 2, 2, 2, 2, 2, 2, 2, 2, 2, 2, 2, 2, 2, 2, 2, 2, 2, 2, 2, 2, 2, 2, 2, 2, 2, 2, 2, 2, 2, 2, 2, 2, 2, 2, 2, 2, 2, 2, 2, 2, 2, 2, 2, 2, 2, 2, 2, 2, 2, 2, 2, 2, 2, 2, 2, 2, 2, 2, 2, 2, 2, 2, 2, 2, 2, 2, 2, 2, 2, 2, 2, 2, 2, 2, 2, 2, 2, 2, 2, 2, 2, 2, 2, 2, 2, 2, 2, 2, 2, 2, 2, 2, 2, 2, 2, 2, 2, 2, 2, 2, 2, 2, 2, 2, 2, 2, 2, 2, 2, 2, 2, 2, 2, 2, 2, 2, 2, 2, 2, 2, 2, 2, 2, 2, 2, 2, 2, 2, 2, 2, 2, 2, 2, 2, 2, 2, 2, 2, 2, 2, 2, 2, 2, 2, 2, 2, 2, 2, 2, 2, 2, 2, 2, 2, 2, 2, 2, 2, 2, 2, 2, 2, 2, 2, 2, 2, 2, 2, 2, 2, 2, 2, 2, 2, 2, 2, 2, 2, 2, 2, 2, 2, 2, 2, 2, 2, 2, 2, 2, 2, 2, 2, 2, 2, 2, 2, 2, 2, 2, 2, 2, 2, 2, 2, 2, 2, 2, 2, 2, 2, 3 ),
 ( 0.000000000000000000, 1.000000000000000000 ),
 ( 0.000000000000000000, 0.002777777777777777884, 0.005555555555555555768, 0.008333333333333333218, 0.01111111111111111154, 0.01388888888888888812, 0.01666666666666666644, 0.01944444444444444475, 0.02222222222222222307, 0.02500000000000000139, 0.02777777777777777624, 0.03055555555555555455, 0.03333333333333333287, 0.03611111111111110772, 0.03888888888888888951, 0.04166666666666666435, 0.04444444444444444614, 0.04722222222222222099, 0.05000000000000000278, 0.05277777777777777762, 0.05555555555555555247, 0.05833333333333333426, 0.06111111111111110911, 0.06388888888888888395, 0.06666666666666666574, 0.06944444444444444753, 0.07222222222222221544, 0.07499999999999999722, 0.07777777777777777901, 0.08055555555555556080, 0.08333333333333332871, 0.08611111111111111049, 0.08888888888888889228, 0.09166666666666666019, 0.09444444444444444198, 0.09722222222222222376, 0.1000000000000000056, 0.1027777777777777735, 0.1055555555555555552, 0.1083333333333333370, 0.1111111111111111049, 0.1138888888888888867, 0.1166666666666666685, 0.1194444444444444503, 0.1222222222222222182, 0.1250000000000000000, 0.1277777777777777679, 0.1305555555555555636, 0.1333333333333333315, 0.1361111111111110994, 0.1388888888888888951, 0.1416666666666666630, 0.1444444444444444309, 0.1472222222222222265, 0.1499999999999999944, 0.1527777777777777901, 0.1555555555555555580, 0.1583333333333333259, 0.1611111111111111216, 0.1638888888888888895, 0.1666666666666666574, 0.1694444444444444531, 0.1722222222222222210, 0.1749999999999999889, 0.1777777777777777846, 0.1805555555555555525, 0.1833333333333333204, 0.1861111111111111160, 0.1888888888888888840, 0.1916666666666666796, 0.1944444444444444475, 0.1972222222222222154, 0.2000000000000000111, 0.2027777777777777790, 0.2055555555555555469, 0.2083333333333333426, 0.2111111111111111105, 0.2138888888888888784, 0.2166666666666666741, 0.2194444444444444420, 0.2222222222222222099, 0.2250000000000000056, 0.2277777777777777735, 0.2305555555555555691, 0.2333333333333333370, 0.2361111111111111049, 0.2388888888888889006, 0.2416666666666666685, 0.2444444444444444364, 0.2472222222222222321, 0.2500000000000000000, 0.2527777777777777679, 0.2555555555555555358, 0.2583333333333333592, 0.2611111111111111271, 0.2638888888888888951, 0.2666666666666666630, 0.2694444444444444309, 0.2722222222222221988, 0.2750000000000000222, 0.2777777777777777901, 0.2805555555555555580, 0.2833333333333333259, 0.2861111111111110938, 0.2888888888888888618, 0.2916666666666666852, 0.2944444444444444531, 0.2972222222222222210, 0.2999999999999999889, 0.3027777777777777568, 0.3055555555555555802, 0.3083333333333333481, 0.3111111111111111160, 0.3138888888888888840, 0.3166666666666666519, 0.3194444444444444198, 0.3222222222222222432, 0.3250000000000000111, 0.3277777777777777790, 0.3305555555555555469, 0.3333333333333333148, 0.3361111111111111382, 0.3388888888888889062, 0.3416666666666666741, 0.3444444444444444420, 0.3472222222222222099, 0.3499999999999999778, 0.3527777777777778012, 0.3555555555555555691, 0.3583333333333333370, 0.3611111111111111049, 0.3638888888888888729, 0.3666666666666666408, 0.3694444444444444642, 0.3722222222222222321, 0.3750000000000000000, 0.3777777777777777679, 0.3805555555555555358, 0.3833333333333333592, 0.3861111111111111271, 0.3888888888888888951, 0.3916666666666666630, 0.3944444444444444309, 0.3972222222222221988, 0.4000000000000000222, 0.4027777777777777901, 0.4055555555555555580, 0.4083333333333333259, 0.4111111111111110938, 0.4138888888888888618, 0.4166666666666666852, 0.4194444444444444531, 0.4222222222222222210, 0.4249999999999999889, 0.4277777777777777568, 0.4305555555555555802, 0.4333333333333333481, 0.4361111111111111160, 0.4388888888888888840, 0.4416666666666666519, 0.4444444444444444198, 0.4472222222222222432, 0.4500000000000000111, 0.4527777777777777790, 0.4555555555555555469, 0.4583333333333333148, 0.4611111111111111382, 0.4638888888888889062, 0.4666666666666666741, 0.4694444444444444420, 0.4722222222222222099, 0.4749999999999999778, 0.4777777777777778012, 0.4805555555555555691, 0.4833333333333333370, 0.4861111111111111049, 0.4888888888888888729, 0.4916666666666666408, 0.4944444444444444642, 0.4972222222222222321, 0.5000000000000000000, 0.5027777777777777679, 0.5055555555555555358, 0.5083333333333333037, 0.5111111111111110716, 0.5138888888888888395, 0.5166666666666667185, 0.5194444444444444864, 0.5222222222222222543, 0.5250000000000000222, 0.5277777777777777901, 0.5305555555555555580, 0.5333333333333333259, 0.5361111111111110938, 0.5388888888888888618, 0.5416666666666666297, 0.5444444444444443976, 0.5472222222222222765, 0.5500000000000000444, 0.5527777777777778123, 0.5555555555555555802, 0.5583333333333333481, 0.5611111111111111160, 0.5638888888888888840, 0.5666666666666666519, 0.5694444444444444198, 0.5722222222222221877, 0.5749999999999999556, 0.5777777777777777235, 0.5805555555555556024, 0.5833333333333333703, 0.5861111111111111382, 0.5888888888888889062, 0.5916666666666666741, 0.5944444444444444420, 0.5972222222222222099, 0.5999999999999999778, 0.6027777777777777457, 0.6055555555555555136, 0.6083333333333332815, 0.6111111111111111605, 0.6138888888888889284, 0.6166666666666666963, 0.6194444444444444642, 0.6222222222222222321, 0.6250000000000000000, 0.6277777777777777679, 0.6305555555555555358, 0.6333333333333333037, 0.6361111111111110716, 0.6388888888888888395, 0.6416666666666667185, 0.6444444444444444864, 0.6472222222222222543, 0.6500000000000000222, 0.6527777777777777901, 0.6555555555555555580, 0.6583333333333333259, 0.6611111111111110938, 0.6638888888888888618, 0.6666666666666666297, 0.6694444444444443976, 0.6722222222222222765, 0.6750000000000000444, 0.6777777777777778123, 0.6805555555555555802, 0.6833333333333333481, 0.6861111111111111160, 0.6888888888888888840, 0.6916666666666666519, 0.6944444444444444198, 0.6972222222222221877, 0.6999999999999999556, 0.7027777777777777235, 0.7055555555555556024, 0.7083333333333333703, 0.7111111111111111382, 0.7138888888888889062, 0.7166666666666666741, 0.7194444444444444420, 0.7222222222222222099, 0.7249999999999999778, 0.7277777777777777457, 0.7305555555555555136, 0.7333333333333332815, 0.7361111111111111605, 0.7388888888888889284, 0.7416666666666666963, 0.7444444444444444642, 0.7472222222222222321, 0.7500000000000000000, 0.7527777777777777679, 0.7555555555555555358, 0.7583333333333333037, 0.7611111111111110716, 0.7638888888888888395, 0.7666666666666667185, 0.7694444444444444864, 0.7722222222222222543, 0.7750000000000000222, 0.7777777777777777901, 0.7805555555555555580, 0.7833333333333333259, 0.7861111111111110938, 0.7888888888888888618, 0.7916666666666666297, 0.7944444444444443976, 0.7972222222222222765, 0.8000000000000000444, 0.8027777777777778123, 0.8055555555555555802, 0.8083333333333333481, 0.8111111111111111160, 0.8138888888888888840, 0.8166666666666666519, 0.8194444444444444198, 0.8222222222222221877, 0.8249999999999999556, 0.8277777777777777235, 0.8305555555555556024, 0.8333333333333333703, 0.8361111111111111382, 0.8388888888888889062, 0.8416666666666666741, 0.8444444444444444420, 0.8472222222222222099, 0.8499999999999999778, 0.8527777777777777457, 0.8555555555555555136, 0.8583333333333332815, 0.8611111111111111605, 0.8638888888888889284, 0.8666666666666666963, 0.8694444444444444642, 0.8722222222222222321, 0.8750000000000000000, 0.8777777777777777679, 0.8805555555555555358, 0.8833333333333333037, 0.8861111111111110716, 0.8888888888888888395, 0.8916666666666667185, 0.8944444444444444864, 0.8972222222222222543, 0.9000000000000000222, 0.9027777777777777901, 0.9055555555555555580, 0.9083333333333333259, 0.9111111111111110938, 0.9138888888888888618, 0.9166666666666666297, 0.9194444444444443976, 0.9222222222222222765, 0.9250000000000000444, 0.9277777777777778123, 0.9305555555555555802, 0.9333333333333333481, 0.9361111111111111160, 0.9388888888888888840, 0.9416666666666666519, 0.9444444444444444198, 0.9472222222222221877, 0.9499999999999999556, 0.9527777777777777235, 0.9555555555555556024, 0.9583333333333333703, 0.9611111111111111382, 0.9638888888888889062, 0.9666666666666666741, 0.9694444444444444420, 0.9722222222222222099, 0.9749999999999999778, 0.9777777777777777457, 0.9805555555555555136, 0.9833333333333332815, 0.9861111111111111605, 0.9888888888888889284, 0.9916666666666666963, 0.9944444444444444642, 0.9972222222222222321, 1.000000000000000000 ),
 .UNSPECIFIED. ) 
 GEOMETRIC_REPRESENTATION_ITEM ( )  RATIONAL_B_SPLINE_SURFACE ( (
 ( 1.000000000000000000, 0.8660254037844387076, 1.000000000000000000, 0.8660254037844387076, 1.000000000000000000, 0.8660254037844387076, 1.000000000000000000, 0.8660254037844387076, 1.000000000000000000, 0.8660254037844387076, 1.000000000000000000, 0.8660254037844387076, 1.000000000000000000, 0.8660254037844387076, 1.000000000000000000, 0.8660254037844387076, 1.000000000000000000, 0.8660254037844387076, 1.000000000000000000, 0.8660254037844387076, 1.000000000000000000, 0.8660254037844387076, 1.000000000000000000, 0.8660254037844387076, 1.000000000000000000, 0.8660254037844387076, 1.000000000000000000, 0.8660254037844387076, 1.000000000000000000, 0.8660254037844387076, 1.000000000000000000, 0.8660254037844387076, 1.000000000000000000, 0.8660254037844387076, 1.000000000000000000, 0.8660254037844387076, 1.000000000000000000, 0.8660254037844387076, 1.000000000000000000, 0.8660254037844387076, 1.000000000000000000, 0.8660254037844387076, 1.000000000000000000, 0.8660254037844387076, 1.000000000000000000, 0.8660254037844387076, 1.000000000000000000, 0.8660254037844387076, 1.000000000000000000, 0.8660254037844387076, 1.000000000000000000, 0.8660254037844387076, 1.000000000000000000, 0.8660254037844387076, 1.000000000000000000, 0.8660254037844387076, 1.000000000000000000, 0.8660254037844387076, 1.000000000000000000, 0.8660254037844387076, 1.000000000000000000, 0.8660254037844387076, 1.000000000000000000, 0.8660254037844387076, 1.000000000000000000, 0.8660254037844387076, 1.000000000000000000, 0.8660254037844387076, 1.000000000000000000, 0.8660254037844387076, 1.000000000000000000, 0.8660254037844387076, 1.000000000000000000, 0.8660254037844387076, 1.000000000000000000, 0.8660254037844387076, 1.000000000000000000, 0.8660254037844387076, 1.000000000000000000, 0.8660254037844387076, 1.000000000000000000, 0.8660254037844387076, 1.000000000000000000, 0.8660254037844387076, 1.000000000000000000, 0.8660254037844387076, 1.000000000000000000, 0.8660254037844387076, 1.000000000000000000, 0.8660254037844387076, 1.000000000000000000, 0.8660254037844387076, 1.000000000000000000, 0.8660254037844387076, 1.000000000000000000, 0.8660254037844387076, 1.000000000000000000, 0.8660254037844387076, 1.000000000000000000, 0.8660254037844387076, 1.000000000000000000, 0.8660254037844387076, 1.000000000000000000, 0.8660254037844387076, 1.000000000000000000, 0.8660254037844387076, 1.000000000000000000, 0.8660254037844387076, 1.000000000000000000, 0.8660254037844387076, 1.000000000000000000, 0.8660254037844387076, 1.000000000000000000, 0.8660254037844387076, 1.000000000000000000, 0.8660254037844387076, 1.000000000000000000, 0.8660254037844387076, 1.000000000000000000, 0.8660254037844387076, 1.000000000000000000, 0.8660254037844387076, 1.000000000000000000, 0.8660254037844387076, 1.000000000000000000, 0.8660254037844387076, 1.000000000000000000, 0.8660254037844387076, 1.000000000000000000, 0.8660254037844387076, 1.000000000000000000, 0.8660254037844387076, 1.000000000000000000, 0.8660254037844387076, 1.000000000000000000, 0.8660254037844387076, 1.000000000000000000, 0.8660254037844387076, 1.000000000000000000, 0.8660254037844387076, 1.000000000000000000, 0.8660254037844387076, 1.000000000000000000, 0.8660254037844387076, 1.000000000000000000, 0.8660254037844387076, 1.000000000000000000, 0.8660254037844387076, 1.000000000000000000, 0.8660254037844387076, 1.000000000000000000, 0.8660254037844387076, 1.000000000000000000, 0.8660254037844387076, 1.000000000000000000, 0.8660254037844387076, 1.000000000000000000, 0.8660254037844387076, 1.000000000000000000, 0.8660254037844387076, 1.000000000000000000, 0.8660254037844387076, 1.000000000000000000, 0.8660254037844387076, 1.000000000000000000, 0.8660254037844387076, 1.000000000000000000, 0.8660254037844387076, 1.000000000000000000, 0.8660254037844387076, 1.000000000000000000, 0.8660254037844387076, 1.000000000000000000, 0.8660254037844387076, 1.000000000000000000, 0.8660254037844387076, 1.000000000000000000, 0.8660254037844387076, 1.000000000000000000, 0.8660254037844387076, 1.000000000000000000, 0.8660254037844387076, 1.000000000000000000, 0.8660254037844387076, 1.000000000000000000, 0.8660254037844387076, 1.000000000000000000, 0.8660254037844387076, 1.000000000000000000, 0.8660254037844387076, 1.000000000000000000, 0.8660254037844387076, 1.000000000000000000, 0.8660254037844387076, 1.000000000000000000, 0.8660254037844387076, 1.000000000000000000, 0.8660254037844387076, 1.000000000000000000, 0.8660254037844387076, 1.000000000000000000, 0.8660254037844387076, 1.000000000000000000, 0.8660254037844387076, 1.000000000000000000, 0.8660254037844387076, 1.000000000000000000, 0.8660254037844387076, 1.000000000000000000, 0.8660254037844387076, 1.000000000000000000, 0.8660254037844387076, 1.000000000000000000, 0.8660254037844387076, 1.000000000000000000, 0.8660254037844387076, 1.000000000000000000, 0.8660254037844387076, 1.000000000000000000, 0.8660254037844387076, 1.000000000000000000, 0.8660254037844387076, 1.000000000000000000, 0.8660254037844387076, 1.000000000000000000, 0.8660254037844387076, 1.000000000000000000, 0.8660254037844387076, 1.000000000000000000, 0.8660254037844387076, 1.000000000000000000, 0.8660254037844387076, 1.000000000000000000, 0.8660254037844387076, 1.000000000000000000, 0.8660254037844387076, 1.000000000000000000, 0.8660254037844387076, 1.000000000000000000, 0.8660254037844387076, 1.000000000000000000, 0.8660254037844387076, 1.000000000000000000, 0.8660254037844387076, 1.000000000000000000, 0.8660254037844387076, 1.000000000000000000, 0.8660254037844387076, 1.000000000000000000, 0.8660254037844387076, 1.000000000000000000, 0.8660254037844387076, 1.000000000000000000, 0.8660254037844387076, 1.000000000000000000, 0.8660254037844387076, 1.000000000000000000, 0.8660254037844387076, 1.000000000000000000, 0.8660254037844387076, 1.000000000000000000, 0.8660254037844387076, 1.000000000000000000, 0.8660254037844387076, 1.000000000000000000, 0.8660254037844387076, 1.000000000000000000, 0.8660254037844387076, 1.000000000000000000, 0.8660254037844387076, 1.000000000000000000, 0.8660254037844387076, 1.000000000000000000, 0.8660254037844387076, 1.000000000000000000, 0.8660254037844387076, 1.000000000000000000, 0.8660254037844387076, 1.000000000000000000, 0.8660254037844387076, 1.000000000000000000, 0.8660254037844387076, 1.000000000000000000, 0.8660254037844387076, 1.000000000000000000, 0.8660254037844387076, 1.000000000000000000, 0.8660254037844387076, 1.000000000000000000, 0.8660254037844387076, 1.000000000000000000, 0.8660254037844387076, 1.000000000000000000, 0.8660254037844387076, 1.000000000000000000, 0.8660254037844387076, 1.000000000000000000, 0.8660254037844387076, 1.000000000000000000, 0.8660254037844387076, 1.000000000000000000, 0.8660254037844387076, 1.000000000000000000, 0.8660254037844387076, 1.000000000000000000, 0.8660254037844387076, 1.000000000000000000, 0.8660254037844387076, 1.000000000000000000, 0.8660254037844387076, 1.000000000000000000, 0.8660254037844387076, 1.000000000000000000, 0.8660254037844387076, 1.000000000000000000, 0.8660254037844387076, 1.000000000000000000, 0.8660254037844387076, 1.000000000000000000, 0.8660254037844387076, 1.000000000000000000, 0.8660254037844387076, 1.000000000000000000, 0.8660254037844387076, 1.000000000000000000, 0.8660254037844387076, 1.000000000000000000, 0.8660254037844387076, 1.000000000000000000, 0.8660254037844387076, 1.000000000000000000, 0.8660254037844387076, 1.000000000000000000, 0.8660254037844387076, 1.000000000000000000, 0.8660254037844387076, 1.000000000000000000, 0.8660254037844387076, 1.000000000000000000, 0.8660254037844387076, 1.000000000000000000, 0.8660254037844387076, 1.000000000000000000, 0.8660254037844387076, 1.000000000000000000, 0.8660254037844387076, 1.000000000000000000, 0.8660254037844387076, 1.000000000000000000, 0.8660254037844387076, 1.000000000000000000, 0.8660254037844387076, 1.000000000000000000, 0.8660254037844387076, 1.000000000000000000, 0.8660254037844387076, 1.000000000000000000, 0.8660254037844387076, 1.000000000000000000, 0.8660254037844387076, 1.000000000000000000, 0.8660254037844387076, 1.000000000000000000, 0.8660254037844387076, 1.000000000000000000, 0.8660254037844387076, 1.000000000000000000, 0.8660254037844387076, 1.000000000000000000, 0.8660254037844387076, 1.000000000000000000, 0.8660254037844387076, 1.000000000000000000, 0.8660254037844387076, 1.000000000000000000, 0.8660254037844387076, 1.000000000000000000, 0.8660254037844387076, 1.000000000000000000, 0.8660254037844387076, 1.000000000000000000, 0.8660254037844387076, 1.000000000000000000, 0.8660254037844387076, 1.000000000000000000, 0.8660254037844387076, 1.000000000000000000, 0.8660254037844387076, 1.000000000000000000, 0.8660254037844387076, 1.000000000000000000, 0.8660254037844387076, 1.000000000000000000, 0.8660254037844387076, 1.000000000000000000, 0.8660254037844387076, 1.000000000000000000, 0.8660254037844387076, 1.000000000000000000, 0.8660254037844387076, 1.000000000000000000, 0.8660254037844387076, 1.000000000000000000, 0.8660254037844387076, 1.000000000000000000, 0.8660254037844387076, 1.000000000000000000, 0.8660254037844387076, 1.000000000000000000, 0.8660254037844387076, 1.000000000000000000, 0.8660254037844387076, 1.000000000000000000, 0.8660254037844387076, 1.000000000000000000, 0.8660254037844387076, 1.000000000000000000, 0.8660254037844387076, 1.000000000000000000, 0.8660254037844387076, 1.000000000000000000, 0.8660254037844387076, 1.000000000000000000, 0.8660254037844387076, 1.000000000000000000, 0.8660254037844387076, 1.000000000000000000, 0.8660254037844387076, 1.000000000000000000, 0.8660254037844387076, 1.000000000000000000, 0.8660254037844387076, 1.000000000000000000, 0.8660254037844387076, 1.000000000000000000, 0.8660254037844387076, 1.000000000000000000, 0.8660254037844387076, 1.000000000000000000, 0.8660254037844387076, 1.000000000000000000, 0.8660254037844387076, 1.000000000000000000, 0.8660254037844387076, 1.000000000000000000, 0.8660254037844387076, 1.000000000000000000, 0.8660254037844387076, 1.000000000000000000, 0.8660254037844387076, 1.000000000000000000, 0.8660254037844387076, 1.000000000000000000, 0.8660254037844387076, 1.000000000000000000, 0.8660254037844387076, 1.000000000000000000, 0.8660254037844387076, 1.000000000000000000, 0.8660254037844387076, 1.000000000000000000, 0.8660254037844387076, 1.000000000000000000, 0.8660254037844387076, 1.000000000000000000, 0.8660254037844387076, 1.000000000000000000, 0.8660254037844387076, 1.000000000000000000, 0.8660254037844387076, 1.000000000000000000, 0.8660254037844387076, 1.000000000000000000, 0.8660254037844387076, 1.000000000000000000, 0.8660254037844387076, 1.000000000000000000, 0.8660254037844387076, 1.000000000000000000, 0.8660254037844387076, 1.000000000000000000, 0.8660254037844387076, 1.000000000000000000, 0.8660254037844387076, 1.000000000000000000, 0.8660254037844387076, 1.000000000000000000, 0.8660254037844387076, 1.000000000000000000, 0.8660254037844387076, 1.000000000000000000, 0.8660254037844387076, 1.000000000000000000, 0.8660254037844387076, 1.000000000000000000, 0.8660254037844387076, 1.000000000000000000, 0.8660254037844387076, 1.000000000000000000, 0.8660254037844387076, 1.000000000000000000, 0.8660254037844387076, 1.000000000000000000, 0.8660254037844387076, 1.000000000000000000, 0.8660254037844387076, 1.000000000000000000, 0.8660254037844387076, 1.000000000000000000, 0.8660254037844387076, 1.000000000000000000, 0.8660254037844387076, 1.000000000000000000, 0.8660254037844387076, 1.000000000000000000, 0.8660254037844387076, 1.000000000000000000, 0.8660254037844387076, 1.000000000000000000, 0.8660254037844387076, 1.000000000000000000, 0.8660254037844387076, 1.000000000000000000, 0.8660254037844387076, 1.000000000000000000, 0.8660254037844387076, 1.000000000000000000, 0.8660254037844387076, 1.000000000000000000, 0.8660254037844387076, 1.000000000000000000, 0.8660254037844387076, 1.000000000000000000, 0.8660254037844387076, 1.000000000000000000, 0.8660254037844387076, 1.000000000000000000, 0.8660254037844387076, 1.000000000000000000, 0.8660254037844387076, 1.000000000000000000, 0.8660254037844387076, 1.000000000000000000, 0.8660254037844387076, 1.000000000000000000, 0.8660254037844387076, 1.000000000000000000, 0.8660254037844387076, 1.000000000000000000, 0.8660254037844387076, 1.000000000000000000, 0.8660254037844387076, 1.000000000000000000, 0.8660254037844387076, 1.000000000000000000, 0.8660254037844387076, 1.000000000000000000, 0.8660254037844387076, 1.000000000000000000, 0.8660254037844387076, 1.000000000000000000, 0.8660254037844387076, 1.000000000000000000, 0.8660254037844387076, 1.000000000000000000, 0.8660254037844387076, 1.000000000000000000, 0.8660254037844387076, 1.000000000000000000, 0.8660254037844387076, 1.000000000000000000, 0.8660254037844387076, 1.000000000000000000, 0.8660254037844387076, 1.000000000000000000, 0.8660254037844387076, 1.000000000000000000, 0.8660254037844387076, 1.000000000000000000, 0.8660254037844387076, 1.000000000000000000, 0.8660254037844387076, 1.000000000000000000, 0.8660254037844387076, 1.000000000000000000, 0.8660254037844387076, 1.000000000000000000, 0.8660254037844387076, 1.000000000000000000, 0.8660254037844387076, 1.000000000000000000, 0.8660254037844387076, 1.000000000000000000, 0.8660254037844387076, 1.000000000000000000, 0.8660254037844387076, 1.000000000000000000, 0.8660254037844387076, 1.000000000000000000, 0.8660254037844387076, 1.000000000000000000, 0.8660254037844387076, 1.000000000000000000, 0.8660254037844387076, 1.000000000000000000, 0.8660254037844387076, 1.000000000000000000, 0.8660254037844387076, 1.000000000000000000, 0.8660254037844387076, 1.000000000000000000, 0.8660254037844387076, 1.000000000000000000, 0.8660254037844387076, 1.000000000000000000, 0.8660254037844387076, 1.000000000000000000, 0.8660254037844387076, 1.000000000000000000, 0.8660254037844387076, 1.000000000000000000, 0.8660254037844387076, 1.000000000000000000, 0.8660254037844387076, 1.000000000000000000, 0.8660254037844387076, 1.000000000000000000, 0.8660254037844387076, 1.000000000000000000, 0.8660254037844387076, 1.000000000000000000, 0.8660254037844387076, 1.000000000000000000, 0.8660254037844387076, 1.000000000000000000, 0.8660254037844387076, 1.000000000000000000, 0.8660254037844387076, 1.000000000000000000, 0.8660254037844387076, 1.000000000000000000, 0.8660254037844387076, 1.000000000000000000, 0.8660254037844387076, 1.000000000000000000, 0.8660254037844387076, 1.000000000000000000, 0.8660254037844387076, 1.000000000000000000, 0.8660254037844387076, 1.000000000000000000, 0.8660254037844387076, 1.000000000000000000, 0.8660254037844387076, 1.000000000000000000, 0.8660254037844387076, 1.000000000000000000, 0.8660254037844387076, 1.000000000000000000, 0.8660254037844387076, 1.000000000000000000, 0.8660254037844387076, 1.000000000000000000, 0.8660254037844387076, 1.000000000000000000, 0.8660254037844387076, 1.000000000000000000, 0.8660254037844387076, 1.000000000000000000, 0.8660254037844387076, 1.000000000000000000, 0.8660254037844387076, 1.000000000000000000, 0.8660254037844387076, 1.000000000000000000, 0.8660254037844387076, 1.000000000000000000, 0.8660254037844387076, 1.000000000000000000, 0.8660254037844387076, 1.000000000000000000, 0.8660254037844387076, 1.000000000000000000, 0.8660254037844387076, 1.000000000000000000, 0.8660254037844387076, 1.000000000000000000, 0.8660254037844387076, 1.000000000000000000, 0.8660254037844387076, 1.000000000000000000, 0.8660254037844387076, 1.000000000000000000, 0.8660254037844387076, 1.000000000000000000, 0.8660254037844387076, 1.000000000000000000, 0.8660254037844387076, 1.000000000000000000, 0.8660254037844387076, 1.000000000000000000, 0.8660254037844387076, 1.000000000000000000, 0.8660254037844387076, 1.000000000000000000, 0.8660254037844387076, 1.000000000000000000, 0.8660254037844387076, 1.000000000000000000, 0.8660254037844387076, 1.000000000000000000, 0.8660254037844387076, 1.000000000000000000, 0.8660254037844387076, 1.000000000000000000, 0.8660254037844387076, 1.000000000000000000, 0.8660254037844387076, 1.000000000000000000, 0.8660254037844387076, 1.000000000000000000),
 ( 1.000000000000000000, 0.8660254037844387076, 1.000000000000000000, 0.8660254037844387076, 1.000000000000000000, 0.8660254037844387076, 1.000000000000000000, 0.8660254037844387076, 1.000000000000000000, 0.8660254037844387076, 1.000000000000000000, 0.8660254037844387076, 1.000000000000000000, 0.8660254037844387076, 1.000000000000000000, 0.8660254037844387076, 1.000000000000000000, 0.8660254037844387076, 1.000000000000000000, 0.8660254037844387076, 1.000000000000000000, 0.8660254037844387076, 1.000000000000000000, 0.8660254037844387076, 1.000000000000000000, 0.8660254037844387076, 1.000000000000000000, 0.8660254037844387076, 1.000000000000000000, 0.8660254037844387076, 1.000000000000000000, 0.8660254037844387076, 1.000000000000000000, 0.8660254037844387076, 1.000000000000000000, 0.8660254037844387076, 1.000000000000000000, 0.8660254037844387076, 1.000000000000000000, 0.8660254037844387076, 1.000000000000000000, 0.8660254037844387076, 1.000000000000000000, 0.8660254037844387076, 1.000000000000000000, 0.8660254037844387076, 1.000000000000000000, 0.8660254037844387076, 1.000000000000000000, 0.8660254037844387076, 1.000000000000000000, 0.8660254037844387076, 1.000000000000000000, 0.8660254037844387076, 1.000000000000000000, 0.8660254037844387076, 1.000000000000000000, 0.8660254037844387076, 1.000000000000000000, 0.8660254037844387076, 1.000000000000000000, 0.8660254037844387076, 1.000000000000000000, 0.8660254037844387076, 1.000000000000000000, 0.8660254037844387076, 1.000000000000000000, 0.8660254037844387076, 1.000000000000000000, 0.8660254037844387076, 1.000000000000000000, 0.8660254037844387076, 1.000000000000000000, 0.8660254037844387076, 1.000000000000000000, 0.8660254037844387076, 1.000000000000000000, 0.8660254037844387076, 1.000000000000000000, 0.8660254037844387076, 1.000000000000000000, 0.8660254037844387076, 1.000000000000000000, 0.8660254037844387076, 1.000000000000000000, 0.8660254037844387076, 1.000000000000000000, 0.8660254037844387076, 1.000000000000000000, 0.8660254037844387076, 1.000000000000000000, 0.8660254037844387076, 1.000000000000000000, 0.8660254037844387076, 1.000000000000000000, 0.8660254037844387076, 1.000000000000000000, 0.8660254037844387076, 1.000000000000000000, 0.8660254037844387076, 1.000000000000000000, 0.8660254037844387076, 1.000000000000000000, 0.8660254037844387076, 1.000000000000000000, 0.8660254037844387076, 1.000000000000000000, 0.8660254037844387076, 1.000000000000000000, 0.8660254037844387076, 1.000000000000000000, 0.8660254037844387076, 1.000000000000000000, 0.8660254037844387076, 1.000000000000000000, 0.8660254037844387076, 1.000000000000000000, 0.8660254037844387076, 1.000000000000000000, 0.8660254037844387076, 1.000000000000000000, 0.8660254037844387076, 1.000000000000000000, 0.8660254037844387076, 1.000000000000000000, 0.8660254037844387076, 1.000000000000000000, 0.8660254037844387076, 1.000000000000000000, 0.8660254037844387076, 1.000000000000000000, 0.8660254037844387076, 1.000000000000000000, 0.8660254037844387076, 1.000000000000000000, 0.8660254037844387076, 1.000000000000000000, 0.8660254037844387076, 1.000000000000000000, 0.8660254037844387076, 1.000000000000000000, 0.8660254037844387076, 1.000000000000000000, 0.8660254037844387076, 1.000000000000000000, 0.8660254037844387076, 1.000000000000000000, 0.8660254037844387076, 1.000000000000000000, 0.8660254037844387076, 1.000000000000000000, 0.8660254037844387076, 1.000000000000000000, 0.8660254037844387076, 1.000000000000000000, 0.8660254037844387076, 1.000000000000000000, 0.8660254037844387076, 1.000000000000000000, 0.8660254037844387076, 1.000000000000000000, 0.8660254037844387076, 1.000000000000000000, 0.8660254037844387076, 1.000000000000000000, 0.8660254037844387076, 1.000000000000000000, 0.8660254037844387076, 1.000000000000000000, 0.8660254037844387076, 1.000000000000000000, 0.8660254037844387076, 1.000000000000000000, 0.8660254037844387076, 1.000000000000000000, 0.8660254037844387076, 1.000000000000000000, 0.8660254037844387076, 1.000000000000000000, 0.8660254037844387076, 1.000000000000000000, 0.8660254037844387076, 1.000000000000000000, 0.8660254037844387076, 1.000000000000000000, 0.8660254037844387076, 1.000000000000000000, 0.8660254037844387076, 1.000000000000000000, 0.8660254037844387076, 1.000000000000000000, 0.8660254037844387076, 1.000000000000000000, 0.8660254037844387076, 1.000000000000000000, 0.8660254037844387076, 1.000000000000000000, 0.8660254037844387076, 1.000000000000000000, 0.8660254037844387076, 1.000000000000000000, 0.8660254037844387076, 1.000000000000000000, 0.8660254037844387076, 1.000000000000000000, 0.8660254037844387076, 1.000000000000000000, 0.8660254037844387076, 1.000000000000000000, 0.8660254037844387076, 1.000000000000000000, 0.8660254037844387076, 1.000000000000000000, 0.8660254037844387076, 1.000000000000000000, 0.8660254037844387076, 1.000000000000000000, 0.8660254037844387076, 1.000000000000000000, 0.8660254037844387076, 1.000000000000000000, 0.8660254037844387076, 1.000000000000000000, 0.8660254037844387076, 1.000000000000000000, 0.8660254037844387076, 1.000000000000000000, 0.8660254037844387076, 1.000000000000000000, 0.8660254037844387076, 1.000000000000000000, 0.8660254037844387076, 1.000000000000000000, 0.8660254037844387076, 1.000000000000000000, 0.8660254037844387076, 1.000000000000000000, 0.8660254037844387076, 1.000000000000000000, 0.8660254037844387076, 1.000000000000000000, 0.8660254037844387076, 1.000000000000000000, 0.8660254037844387076, 1.000000000000000000, 0.8660254037844387076, 1.000000000000000000, 0.8660254037844387076, 1.000000000000000000, 0.8660254037844387076, 1.000000000000000000, 0.8660254037844387076, 1.000000000000000000, 0.8660254037844387076, 1.000000000000000000, 0.8660254037844387076, 1.000000000000000000, 0.8660254037844387076, 1.000000000000000000, 0.8660254037844387076, 1.000000000000000000, 0.8660254037844387076, 1.000000000000000000, 0.8660254037844387076, 1.000000000000000000, 0.8660254037844387076, 1.000000000000000000, 0.8660254037844387076, 1.000000000000000000, 0.8660254037844387076, 1.000000000000000000, 0.8660254037844387076, 1.000000000000000000, 0.8660254037844387076, 1.000000000000000000, 0.8660254037844387076, 1.000000000000000000, 0.8660254037844387076, 1.000000000000000000, 0.8660254037844387076, 1.000000000000000000, 0.8660254037844387076, 1.000000000000000000, 0.8660254037844387076, 1.000000000000000000, 0.8660254037844387076, 1.000000000000000000, 0.8660254037844387076, 1.000000000000000000, 0.8660254037844387076, 1.000000000000000000, 0.8660254037844387076, 1.000000000000000000, 0.8660254037844387076, 1.000000000000000000, 0.8660254037844387076, 1.000000000000000000, 0.8660254037844387076, 1.000000000000000000, 0.8660254037844387076, 1.000000000000000000, 0.8660254037844387076, 1.000000000000000000, 0.8660254037844387076, 1.000000000000000000, 0.8660254037844387076, 1.000000000000000000, 0.8660254037844387076, 1.000000000000000000, 0.8660254037844387076, 1.000000000000000000, 0.8660254037844387076, 1.000000000000000000, 0.8660254037844387076, 1.000000000000000000, 0.8660254037844387076, 1.000000000000000000, 0.8660254037844387076, 1.000000000000000000, 0.8660254037844387076, 1.000000000000000000, 0.8660254037844387076, 1.000000000000000000, 0.8660254037844387076, 1.000000000000000000, 0.8660254037844387076, 1.000000000000000000, 0.8660254037844387076, 1.000000000000000000, 0.8660254037844387076, 1.000000000000000000, 0.8660254037844387076, 1.000000000000000000, 0.8660254037844387076, 1.000000000000000000, 0.8660254037844387076, 1.000000000000000000, 0.8660254037844387076, 1.000000000000000000, 0.8660254037844387076, 1.000000000000000000, 0.8660254037844387076, 1.000000000000000000, 0.8660254037844387076, 1.000000000000000000, 0.8660254037844387076, 1.000000000000000000, 0.8660254037844387076, 1.000000000000000000, 0.8660254037844387076, 1.000000000000000000, 0.8660254037844387076, 1.000000000000000000, 0.8660254037844387076, 1.000000000000000000, 0.8660254037844387076, 1.000000000000000000, 0.8660254037844387076, 1.000000000000000000, 0.8660254037844387076, 1.000000000000000000, 0.8660254037844387076, 1.000000000000000000, 0.8660254037844387076, 1.000000000000000000, 0.8660254037844387076, 1.000000000000000000, 0.8660254037844387076, 1.000000000000000000, 0.8660254037844387076, 1.000000000000000000, 0.8660254037844387076, 1.000000000000000000, 0.8660254037844387076, 1.000000000000000000, 0.8660254037844387076, 1.000000000000000000, 0.8660254037844387076, 1.000000000000000000, 0.8660254037844387076, 1.000000000000000000, 0.8660254037844387076, 1.000000000000000000, 0.8660254037844387076, 1.000000000000000000, 0.8660254037844387076, 1.000000000000000000, 0.8660254037844387076, 1.000000000000000000, 0.8660254037844387076, 1.000000000000000000, 0.8660254037844387076, 1.000000000000000000, 0.8660254037844387076, 1.000000000000000000, 0.8660254037844387076, 1.000000000000000000, 0.8660254037844387076, 1.000000000000000000, 0.8660254037844387076, 1.000000000000000000, 0.8660254037844387076, 1.000000000000000000, 0.8660254037844387076, 1.000000000000000000, 0.8660254037844387076, 1.000000000000000000, 0.8660254037844387076, 1.000000000000000000, 0.8660254037844387076, 1.000000000000000000, 0.8660254037844387076, 1.000000000000000000, 0.8660254037844387076, 1.000000000000000000, 0.8660254037844387076, 1.000000000000000000, 0.8660254037844387076, 1.000000000000000000, 0.8660254037844387076, 1.000000000000000000, 0.8660254037844387076, 1.000000000000000000, 0.8660254037844387076, 1.000000000000000000, 0.8660254037844387076, 1.000000000000000000, 0.8660254037844387076, 1.000000000000000000, 0.8660254037844387076, 1.000000000000000000, 0.8660254037844387076, 1.000000000000000000, 0.8660254037844387076, 1.000000000000000000, 0.8660254037844387076, 1.000000000000000000, 0.8660254037844387076, 1.000000000000000000, 0.8660254037844387076, 1.000000000000000000, 0.8660254037844387076, 1.000000000000000000, 0.8660254037844387076, 1.000000000000000000, 0.8660254037844387076, 1.000000000000000000, 0.8660254037844387076, 1.000000000000000000, 0.8660254037844387076, 1.000000000000000000, 0.8660254037844387076, 1.000000000000000000, 0.8660254037844387076, 1.000000000000000000, 0.8660254037844387076, 1.000000000000000000, 0.8660254037844387076, 1.000000000000000000, 0.8660254037844387076, 1.000000000000000000, 0.8660254037844387076, 1.000000000000000000, 0.8660254037844387076, 1.000000000000000000, 0.8660254037844387076, 1.000000000000000000, 0.8660254037844387076, 1.000000000000000000, 0.8660254037844387076, 1.000000000000000000, 0.8660254037844387076, 1.000000000000000000, 0.8660254037844387076, 1.000000000000000000, 0.8660254037844387076, 1.000000000000000000, 0.8660254037844387076, 1.000000000000000000, 0.8660254037844387076, 1.000000000000000000, 0.8660254037844387076, 1.000000000000000000, 0.8660254037844387076, 1.000000000000000000, 0.8660254037844387076, 1.000000000000000000, 0.8660254037844387076, 1.000000000000000000, 0.8660254037844387076, 1.000000000000000000, 0.8660254037844387076, 1.000000000000000000, 0.8660254037844387076, 1.000000000000000000, 0.8660254037844387076, 1.000000000000000000, 0.8660254037844387076, 1.000000000000000000, 0.8660254037844387076, 1.000000000000000000, 0.8660254037844387076, 1.000000000000000000, 0.8660254037844387076, 1.000000000000000000, 0.8660254037844387076, 1.000000000000000000, 0.8660254037844387076, 1.000000000000000000, 0.8660254037844387076, 1.000000000000000000, 0.8660254037844387076, 1.000000000000000000, 0.8660254037844387076, 1.000000000000000000, 0.8660254037844387076, 1.000000000000000000, 0.8660254037844387076, 1.000000000000000000, 0.8660254037844387076, 1.000000000000000000, 0.8660254037844387076, 1.000000000000000000, 0.8660254037844387076, 1.000000000000000000, 0.8660254037844387076, 1.000000000000000000, 0.8660254037844387076, 1.000000000000000000, 0.8660254037844387076, 1.000000000000000000, 0.8660254037844387076, 1.000000000000000000, 0.8660254037844387076, 1.000000000000000000, 0.8660254037844387076, 1.000000000000000000, 0.8660254037844387076, 1.000000000000000000, 0.8660254037844387076, 1.000000000000000000, 0.8660254037844387076, 1.000000000000000000, 0.8660254037844387076, 1.000000000000000000, 0.8660254037844387076, 1.000000000000000000, 0.8660254037844387076, 1.000000000000000000, 0.8660254037844387076, 1.000000000000000000, 0.8660254037844387076, 1.000000000000000000, 0.8660254037844387076, 1.000000000000000000, 0.8660254037844387076, 1.000000000000000000, 0.8660254037844387076, 1.000000000000000000, 0.8660254037844387076, 1.000000000000000000, 0.8660254037844387076, 1.000000000000000000, 0.8660254037844387076, 1.000000000000000000, 0.8660254037844387076, 1.000000000000000000, 0.8660254037844387076, 1.000000000000000000, 0.8660254037844387076, 1.000000000000000000, 0.8660254037844387076, 1.000000000000000000, 0.8660254037844387076, 1.000000000000000000, 0.8660254037844387076, 1.000000000000000000, 0.8660254037844387076, 1.000000000000000000, 0.8660254037844387076, 1.000000000000000000, 0.8660254037844387076, 1.000000000000000000, 0.8660254037844387076, 1.000000000000000000, 0.8660254037844387076, 1.000000000000000000, 0.8660254037844387076, 1.000000000000000000, 0.8660254037844387076, 1.000000000000000000, 0.8660254037844387076, 1.000000000000000000, 0.8660254037844387076, 1.000000000000000000, 0.8660254037844387076, 1.000000000000000000, 0.8660254037844387076, 1.000000000000000000, 0.8660254037844387076, 1.000000000000000000, 0.8660254037844387076, 1.000000000000000000, 0.8660254037844387076, 1.000000000000000000, 0.8660254037844387076, 1.000000000000000000, 0.8660254037844387076, 1.000000000000000000, 0.8660254037844387076, 1.000000000000000000, 0.8660254037844387076, 1.000000000000000000, 0.8660254037844387076, 1.000000000000000000, 0.8660254037844387076, 1.000000000000000000, 0.8660254037844387076, 1.000000000000000000, 0.8660254037844387076, 1.000000000000000000, 0.8660254037844387076, 1.000000000000000000, 0.8660254037844387076, 1.000000000000000000, 0.8660254037844387076, 1.000000000000000000, 0.8660254037844387076, 1.000000000000000000, 0.8660254037844387076, 1.000000000000000000, 0.8660254037844387076, 1.000000000000000000, 0.8660254037844387076, 1.000000000000000000, 0.8660254037844387076, 1.000000000000000000, 0.8660254037844387076, 1.000000000000000000, 0.8660254037844387076, 1.000000000000000000, 0.8660254037844387076, 1.000000000000000000, 0.8660254037844387076, 1.000000000000000000, 0.8660254037844387076, 1.000000000000000000, 0.8660254037844387076, 1.000000000000000000, 0.8660254037844387076, 1.000000000000000000, 0.8660254037844387076, 1.000000000000000000, 0.8660254037844387076, 1.000000000000000000, 0.8660254037844387076, 1.000000000000000000, 0.8660254037844387076, 1.000000000000000000, 0.8660254037844387076, 1.000000000000000000, 0.8660254037844387076, 1.000000000000000000, 0.8660254037844387076, 1.000000000000000000, 0.8660254037844387076, 1.000000000000000000, 0.8660254037844387076, 1.000000000000000000, 0.8660254037844387076, 1.000000000000000000, 0.8660254037844387076, 1.000000000000000000, 0.8660254037844387076, 1.000000000000000000, 0.8660254037844387076, 1.000000000000000000, 0.8660254037844387076, 1.000000000000000000, 0.8660254037844387076, 1.000000000000000000, 0.8660254037844387076, 1.000000000000000000, 0.8660254037844387076, 1.000000000000000000, 0.8660254037844387076, 1.000000000000000000, 0.8660254037844387076, 1.000000000000000000, 0.8660254037844387076, 1.000000000000000000, 0.8660254037844387076, 1.000000000000000000, 0.8660254037844387076, 1.000000000000000000, 0.8660254037844387076, 1.000000000000000000, 0.8660254037844387076, 1.000000000000000000, 0.8660254037844387076, 1.000000000000000000, 0.8660254037844387076, 1.000000000000000000, 0.8660254037844387076, 1.000000000000000000, 0.8660254037844387076, 1.000000000000000000, 0.8660254037844387076, 1.000000000000000000, 0.8660254037844387076, 1.000000000000000000, 0.8660254037844387076, 1.000000000000000000, 0.8660254037844387076, 1.000000000000000000, 0.8660254037844387076, 1.000000000000000000, 0.8660254037844387076, 1.000000000000000000, 0.8660254037844387076, 1.000000000000000000) ) ) 
 REPRESENTATION_ITEM ( '' )  SURFACE ( )  );
#40404 = AXIS2_PLACEMENT_3D ( 'NONE', #57697, #12275, #19248 ) ;
#40405 = CARTESIAN_POINT ( 'NONE',  ( 18.56250000122903288, -4.330127018922190985, -2.500000000000001332 ) ) ;
#40406 = CARTESIAN_POINT ( 'NONE',  ( 24.11249999999999716, 2.886751345948126879, 4.999999999999999112 ) ) ;
#40407 = CARTESIAN_POINT ( 'NONE',  ( -4.243569643749999898, 11.72187500061451892, -32.45002607614398471 ) ) ;
#40408 = CARTESIAN_POINT ( 'NONE',  ( 30.00000000000000000, 0.000000000000000000, 4.999999999999998224 ) ) ;
#40409 = EDGE_CURVE ( 'NONE', #23988, #15128, #13231, .T. ) ;
#40410 = CARTESIAN_POINT ( 'NONE',  ( 3.150000001229034119, -2.886751345948129988, 4.999999999999997335 ) ) ;
#40411 = CARTESIAN_POINT ( 'NONE',  ( 3.999999999999998668, 14.71250000000000213, 32.30940107675850470 ) ) ;
#40412 = CARTESIAN_POINT ( 'NONE',  ( 14.02499999999999858, 6.123233995736764310E-16, -4.999999999999998224 ) ) ;
#40413 = CARTESIAN_POINT ( 'NONE',  ( 19.43437500061451928, 4.541064518000418104, 2.621784821874999949 ) ) ;
#40414 = CARTESIAN_POINT ( 'NONE',  ( 4.000000000000000000, 12.50000000000000000, 30.00000000000000000 ) ) ;
#40415 = CARTESIAN_POINT ( 'NONE',  ( 13.30312500061451786, -4.541064518000417216, -2.621784821875001281 ) ) ;
#40416 = CARTESIAN_POINT ( 'NONE',  ( 9.468750001229032875, -5.773502691896255534, -1.060575238724906372E-15 ) ) ;
#40417 = CARTESIAN_POINT ( 'NONE',  ( 8.925000000000002487, -4.330127018922194537, 2.499999999999995559 ) ) ;
#40418 = CARTESIAN_POINT ( 'NONE',  ( 26.93437500061451573, 6.421520780324663323E-16, -5.243569643749999010 ) ) ;
#40419 = CARTESIAN_POINT ( 'NONE',  ( 17.70937500061451431, -5.492252693125287522, -1.008910452111647106E-15 ) ) ;
#40420 = CARTESIAN_POINT ( 'NONE',  ( 13.11562500061451786, 3.027376345333611329, 5.243569643749999010 ) ) ;
#40421 = CARTESIAN_POINT ( 'NONE',  ( 9.721875000614517148, -6.054752690667223547, -1.112240025338166033E-15 ) ) ;
#40422 = EDGE_LOOP ( 'NONE', ( #24767, #71052, #39496, #31526 ) ) ;
#40423 = CARTESIAN_POINT ( 'NONE',  ( 29.65312500061451573, 4.541064518000418104, -2.621784821874998173 ) ) ;
#40424 = CARTESIAN_POINT ( 'NONE',  ( 21.29062500061451502, -3.027376345333614438, 5.243569643749998122 ) ) ;
#40425 = CYLINDRICAL_SURFACE ( 'NONE', #29789, 4.999999999999998224 ) ;
#40426 = CARTESIAN_POINT ( 'NONE',  ( 2.000000000000001332, 15.31250000122903465, -26.53589838486224650 ) ) ;
#40427 = CARTESIAN_POINT ( 'NONE',  ( 9.225000000000001421, 4.330127018922191873, 2.499999999999999556 ) ) ;
#40428 = CARTESIAN_POINT ( 'NONE',  ( 22.38750000122903216, 4.330127018922191873, 2.499999999999999556 ) ) ;
#40429 = CARTESIAN_POINT ( 'NONE',  ( 17.12812500061451715, 4.541064518000418104, 2.621784821874999949 ) ) ;
#40430 = CARTESIAN_POINT ( 'NONE',  ( 9.834375000614514306, 5.492252693125287522, 3.363034840372157021E-16 ) ) ;
#40431 = VERTEX_POINT ( 'NONE', #341 ) ;
#40432 = CARTESIAN_POINT ( 'NONE',  ( 17.43750000000000355, -2.886751345948129988, 4.999999999999997335 ) ) ;
#40433 = CARTESIAN_POINT ( 'NONE',  ( 22.23750000000000071, 5.773502691896255534, 3.535250795749688894E-16 ) ) ;
#40434 = CARTESIAN_POINT ( 'NONE',  ( 19.65937500061451360, -4.541064518000417216, -2.621784821875001281 ) ) ;
#40435 = CARTESIAN_POINT ( 'NONE',  ( 24.47812500061451502, -4.541064518000419881, 2.621784821874995952 ) ) ;
#40436 = EDGE_LOOP ( 'NONE', ( #67029, #50212, #16520, #21023, #50381, #44975, #58741, #64342, #38765, #40905, #38330, #3323, #45042, #43340, #35233, #22302, #25661, #3049, #15474, #59422, #16571, #68611, #57128, #8345, #55565, #61230, #4779, #43065, #33288, #71506, #6595, #53631, #21250, #63395, #12494, #58572, #66568, #67642, #4649, #6723, #8037, #27040, #9798, #70988, #23546, #42168, #55727, #44805 ) ) ;
#40437 = CARTESIAN_POINT ( 'NONE',  ( -5.810221930991193690E-16, 18.65000000122903501, -34.00000000000000000 ) ) ;
#40438 = B_SPLINE_CURVE_WITH_KNOTS ( 'NONE', 3,
 ( #12304, #46658, #69198, #63635, #23026, #46293, #45582, #35561, #7489, #17830 ),
 .UNSPECIFIED., .F., .F.,
 ( 4, 3, 3, 4 ),
 ( 0.000000000000000000, 7.861231028638042341E-05, 0.0001572246814500608740, 0.0003053779378607085417 ),
 .UNSPECIFIED. ) ;
#40439 = CARTESIAN_POINT ( 'NONE',  ( 9.365625000614519635, 3.027376345333613106, -5.243569643749998122 ) ) ;
#40440 = FACE_OUTER_BOUND ( 'NONE', #16064, .T. ) ;
#40441 = CARTESIAN_POINT ( 'NONE',  ( 15.86250000000000249, 2.886751345948129099, -4.999999999999998224 ) ) ;
#40442 = CARTESIAN_POINT ( 'NONE',  ( -4.243569643749999898, 17.55312500061451786, 30.00000000000000000 ) ) ;
#40443 = CARTESIAN_POINT ( 'NONE',  ( 3.234375000614516438, 4.541064518000418104, 2.621784821874999949 ) ) ;
#40444 = CARTESIAN_POINT ( 'NONE',  ( 10.23750000000000071, -2.886751345948129988, 4.999999999999997335 ) ) ;
#40445 = CARTESIAN_POINT ( 'NONE',  ( 3.756430356250000102, 14.44062499938548250, 30.00000000000000000 ) ) ;
#40446 = CARTESIAN_POINT ( 'NONE',  ( 25.58437500061451431, 6.421520780324663323E-16, -5.243569643749999010 ) ) ;
#40447 = VERTEX_POINT ( 'NONE', #52030 ) ;
#40448 = CARTESIAN_POINT ( 'NONE',  ( 23.69062500061451004, -3.027376345333610441, -5.243569643749999898 ) ) ;
#40449 = CARTESIAN_POINT ( 'NONE',  ( 22.09687500061451715, 6.054752690667223547, 3.707466751127219781E-16 ) ) ;
#40450 = CARTESIAN_POINT ( 'NONE',  ( -4.243569643749999898, 17.10312500061459318, -30.00000000000000000 ) ) ;
#40451 = CARTESIAN_POINT ( 'NONE',  ( 10.72500000000000142, -4.330127018922194537, 2.499999999999995559 ) ) ;
#40452 = CARTESIAN_POINT ( 'NONE',  ( 8.165625000614516793, 3.027376345333611329, 5.243569643749999010 ) ) ;
#40453 = CARTESIAN_POINT ( 'NONE',  ( 28.69687500061451502, -2.746126346562641984, -4.756430356249999214 ) ) ;
#40454 = FACE_OUTER_BOUND ( 'NONE', #47149, .T. ) ;
#40455 = CARTESIAN_POINT ( 'NONE',  ( 26.99062500061451786, 6.054752690667223547, 3.707466751127219781E-16 ) ) ;
#40456 = CARTESIAN_POINT ( 'NONE',  ( 27.23437500061450933, -2.746126346562641984, -4.756430356249999214 ) ) ;
#40457 = CARTESIAN_POINT ( 'NONE',  ( 12.53437500061451537, 5.824947211148865298E-16, -4.756430356249998326 ) ) ;
#40458 = CARTESIAN_POINT ( 'NONE',  ( 19.43437500061451928, 4.541064518000418104, 2.621784821874999949 ) ) ;
#40459 = CARTESIAN_POINT ( 'NONE',  ( -4.243569643749997233, 12.24687500061451928, 32.45002607614398471 ) ) ;
#40460 = CARTESIAN_POINT ( 'NONE',  ( 18.57187500061451857, 3.027376345333611329, 5.243569643749999010 ) ) ;
#40461 = CARTESIAN_POINT ( 'NONE',  ( 27.53437500061451360, 4.541064518000418104, 2.621784821874999949 ) ) ;
#40462 = CARTESIAN_POINT ( 'NONE',  ( -2.121784821874996840, 16.33437500061451786, 33.67503911421598417 ) ) ;
#40463 = CARTESIAN_POINT ( 'NONE',  ( 8.428125000614517859, 6.421520780324663323E-16, -5.243569643749999010 ) ) ;
#40465 =( BOUNDED_CURVE ( )  B_SPLINE_CURVE ( 2, ( #58599, #19433, #13170, #35710, #36078, #41994, #64514, #13907, #36446 ),
 .UNSPECIFIED., .F., .F. ) 
 B_SPLINE_CURVE_WITH_KNOTS ( ( 3, 2, 2, 2, 3 ),
 ( 0.7916666666666667407, 0.7962962962962962798, 0.8055555555555555802, 0.8148148148148147696, 0.8194444444444444198 ),
 .UNSPECIFIED. ) 
 CURVE ( )  GEOMETRIC_REPRESENTATION_ITEM ( )  RATIONAL_B_SPLINE_CURVE ( ( 0.9330127018922192983, 0.9330127018922200755, 1.000000000000000000, 0.8660254037844387076, 1.000000000000000000, 0.8660254037844387076, 1.000000000000000000, 0.9330127018922194093, 0.9330127018922194093 ) ) 
 REPRESENTATION_ITEM ( '' )  );
#40464 = CARTESIAN_POINT ( 'NONE',  ( -2.000000000000000000, 19.02499999999999858, 26.53589838486224650 ) ) ;
#40466 = CARTESIAN_POINT ( 'NONE',  ( 3.759375000614517681, 0.000000000000000000, 5.243569643749999010 ) ) ;
#40467 = CARTESIAN_POINT ( 'NONE',  ( 25.91250000122903074, 4.330127018922192761, -2.499999999999997780 ) ) ;
#40468 = CARTESIAN_POINT ( 'NONE',  ( 4.190625000614518925, -3.027376345333614438, 5.243569643749998122 ) ) ;
#40469 = CARTESIAN_POINT ( 'NONE',  ( 10.24687500061451750, -3.027376345333610441, -5.243569643749999898 ) ) ;
#40470 = FILL_AREA_STYLE ('',( #39387 ) ) ;
#40471 = CARTESIAN_POINT ( 'NONE',  ( 17.02500000122903145, 2.886751345948126879, 4.999999999999999112 ) ) ;
#40472 = CARTESIAN_POINT ( 'NONE',  ( 5.671875000614519102, -6.054752690667223547, -1.112240025338166033E-15 ) ) ;
#40473 = CARTESIAN_POINT ( 'NONE',  ( 6.478125000614516793, -4.541064518000419881, 2.621784821874995952 ) ) ;
#40474 = CARTESIAN_POINT ( 'NONE',  ( 22.80000000000000071, 0.000000000000000000, 4.999999999999998224 ) ) ;
#40475 = CARTESIAN_POINT ( 'NONE',  ( 24.09375000122903288, 5.773502691896255534, 3.535250795749688894E-16 ) ) ;
#40476 = CARTESIAN_POINT ( 'NONE',  ( 16.80937500061451573, 0.000000000000000000, 5.243569643749999010 ) ) ;
#40477 = CARTESIAN_POINT ( 'NONE',  ( -5.810221930991193690E-16, 10.43750000000000000, 26.00000000000000355 ) ) ;
#40478 = ORIENTED_EDGE ( 'NONE', *, *, #58225, .T. ) ;
#40479 = CARTESIAN_POINT ( 'NONE',  ( 23.87812500061451715, 4.541064518000418104, 2.621784821874999949 ) ) ;
#40480 = CARTESIAN_POINT ( 'NONE',  ( 9.178125000614517859, -4.541064518000419881, 2.621784821874995952 ) ) ;
#40481 = CARTESIAN_POINT ( 'NONE',  ( 27.79687500061451644, -3.027376345333610441, -5.243569643749999898 ) ) ;
#40482 = CARTESIAN_POINT ( 'NONE',  ( 9.440625000614517148, 6.054752690667223547, 3.707466751127219781E-16 ) ) ;
#40483 = CARTESIAN_POINT ( 'NONE',  ( -4.243569643749999898, 10.37187500061451750, -32.45002607614398471 ) ) ;
#40484 = CARTESIAN_POINT ( 'NONE',  ( 11.28750000122903252, -4.330127018922194537, 2.499999999999995559 ) ) ;
#40485 = ADVANCED_FACE ( 'NONE', ( #12858 ), #57916, .T. ) ;
#40486 = CARTESIAN_POINT ( 'NONE',  ( 28.07812500061451289, -4.541064518000419881, 2.621784821874995952 ) ) ;
#40487 = CARTESIAN_POINT ( 'NONE',  ( 4.243569643749999010, 13.76562500061451644, -32.45002607614398471 ) ) ;
#40488 = CARTESIAN_POINT ( 'NONE',  ( 13.35000000122903430, 5.773502691896255534, 3.535250795749688894E-16 ) ) ;
#40489 = CARTESIAN_POINT ( 'NONE',  ( 10.49999999999999822, 4.330127018922192761, -2.499999999999997780 ) ) ;
#40490 = CARTESIAN_POINT ( 'NONE',  ( 21.14062500061451289, 6.054752690667223547, 3.707466751127219781E-16 ) ) ;
#40491 = CARTESIAN_POINT ( 'NONE',  ( 22.23750000122903003, 6.123233995736764310E-16, -4.999999999999998224 ) ) ;
#40492 = CARTESIAN_POINT ( 'NONE',  ( 19.46249999999999858, 2.886751345948129099, -4.999999999999998224 ) ) ;
#40493 = CARTESIAN_POINT ( 'NONE',  ( 8.625000001229034652, -5.773502691896255534, -1.060575238724906372E-15 ) ) ;
#40494 = CARTESIAN_POINT ( 'NONE',  ( 15.97500000122903430, 2.886751345948129099, -4.999999999999998224 ) ) ;
#40495 = CARTESIAN_POINT ( 'NONE',  ( 12.02812500061451573, 6.421520780324663323E-16, -5.243569643749999010 ) ) ;
#40496 = CARTESIAN_POINT ( 'NONE',  ( 14.84062500061451750, 6.054752690667223547, 3.707466751127219781E-16 ) ) ;
#40497 = CARTESIAN_POINT ( 'NONE',  ( 25.46250000122903501, 4.330127018922192761, -2.499999999999997780 ) ) ;
#40498 = CARTESIAN_POINT ( 'NONE',  ( 19.65000000000000213, 0.000000000000000000, 4.999999999999998224 ) ) ;
#40499 = CARTESIAN_POINT ( 'NONE',  ( 24.04687500061451644, -3.027376345333614438, 5.243569643749998122 ) ) ;
#40500 = DIRECTION ( 'NONE',  ( -1.000000000000000000, -0.000000000000000000, -0.000000000000000000 ) ) ;
#40501 = EDGE_CURVE ( 'NONE', #14527, #55334, #33115, .T. ) ;
#40502 = CARTESIAN_POINT ( 'NONE',  ( 9.450000001229033941, -2.886751345948129988, 4.999999999999997335 ) ) ;
#40503 = CARTESIAN_POINT ( 'NONE',  ( 8.109375000614518214, 4.541064518000418104, -2.621784821874998173 ) ) ;
#40504 = CARTESIAN_POINT ( 'NONE',  ( 25.50937500061451502, -4.541064518000417216, -2.621784821875001281 ) ) ;
#40505 = DIRECTION ( 'NONE',  ( 0.000000000000000000, 0.000000000000000000, 1.000000000000000000 ) ) ;
#40506 = CARTESIAN_POINT ( 'NONE',  ( 21.14062500061451289, 6.054752690667223547, 3.707466751127219781E-16 ) ) ;
#40507 = CARTESIAN_POINT ( 'NONE',  ( 26.59687500061451360, 6.054752690667223547, 3.707466751127219781E-16 ) ) ;
#40508 = CARTESIAN_POINT ( 'NONE',  ( 3.756430356250000546, 18.19062499938548427, 27.83122392262697886 ) ) ;
#40509 = CARTESIAN_POINT ( 'NONE',  ( 3.210790684466319878, -3.832931176703135989, 3.307821435622600337 ) ) ;
#40510 = CARTESIAN_POINT ( 'NONE',  ( 6.834375000614518747, 4.541064518000418104, 2.621784821874999949 ) ) ;
#40511 = CARTESIAN_POINT ( 'NONE',  ( 20.69062500061451715, 6.054752690667223547, 3.707466751127219781E-16 ) ) ;
#40512 = CARTESIAN_POINT ( 'NONE',  ( 5.000000000000000888, 2.882564675336284927E-11, 5.151554443534156036 ) ) ;
#40513 = CARTESIAN_POINT ( 'NONE',  ( 28.71562500061451573, 3.027376345333613106, -5.243569643749998122 ) ) ;
#40514 = CARTESIAN_POINT ( 'NONE',  ( 3.684375000614518836, 4.541064518000418104, 2.621784821874999949 ) ) ;
#40515 = EDGE_CURVE ( 'NONE', #68271, #19034, #50806, .T. ) ;
#40516 = CARTESIAN_POINT ( 'NONE',  ( 4.661467738957717266, -1.808512791952580301, -4.661467738957749241 ) ) ;
#40517 = CARTESIAN_POINT ( 'NONE',  ( 17.81250000000000355, 2.886751345948126879, 4.999999999999999112 ) ) ;
#40518 = ORIENTED_EDGE ( 'NONE', *, *, #35579, .T. ) ;
#40519 = CARTESIAN_POINT ( 'NONE',  ( 24.86250000000000071, 2.886751345948129099, -4.999999999999998224 ) ) ;
#40520 = CARTESIAN_POINT ( 'NONE',  ( 26.55937500061451573, 4.541064518000418104, -2.621784821874998173 ) ) ;
#40521 = ORIENTED_EDGE ( 'NONE', *, *, #23221, .F. ) ;
#40522 = CARTESIAN_POINT ( 'NONE',  ( 14.72812500061451679, 6.421520780324663323E-16, -5.243569643749999010 ) ) ;
#40523 = CARTESIAN_POINT ( 'NONE',  ( 7.003125000614518036, -4.541064518000417216, -2.621784821875001281 ) ) ;
#40524 = CARTESIAN_POINT ( 'NONE',  ( 19.13437500061451502, -2.746126346562642428, -4.756430356249999214 ) ) ;
#40525 = CARTESIAN_POINT ( 'NONE',  ( 4.359375000614517326, -4.541064518000417216, -2.621784821875001281 ) ) ;
#40526 = CARTESIAN_POINT ( 'NONE',  ( 14.36250000122903359, 0.000000000000000000, 4.999999999999998224 ) ) ;
#40527 = CARTESIAN_POINT ( 'NONE',  ( 21.03750000000000142, -2.886751345948129988, 4.999999999999997335 ) ) ;
#40528 = CARTESIAN_POINT ( 'NONE',  ( 4.898850051585143718E-16, 25.54316770519903557, 34.00000000000000000 ) ) ;
#40529 = CARTESIAN_POINT ( 'NONE',  ( 4.171875000614517326, 3.027376345333611329, 5.243569643749999010 ) ) ;
#40530 = CARTESIAN_POINT ( 'NONE',  ( 8.146875000614516082, 6.054752690667223547, 3.707466751127219781E-16 ) ) ;
#40531 = CARTESIAN_POINT ( 'NONE',  ( 20.82187500061451857, 3.027376345333611329, 5.243569643749999010 ) ) ;
#40532 = FACE_OUTER_BOUND ( 'NONE', #61776, .T. ) ;
#40533 = ORIENTED_EDGE ( 'NONE', *, *, #13214, .F. ) ;
#40534 = CARTESIAN_POINT ( 'NONE',  ( 4.321875000614517681, -6.054752690667223547, -1.112240025338166033E-15 ) ) ;
#40535 = CARTESIAN_POINT ( 'NONE',  ( 5.062500000000000888, 2.886751345948129099, -4.999999999999998224 ) ) ;
#40536 = CARTESIAN_POINT ( 'NONE',  ( 6.309375000614517504, 4.541064518000418104, -2.621784821874998173 ) ) ;
#40537 = CARTESIAN_POINT ( 'NONE',  ( 19.01249999999999929, 2.886751345948129099, -4.999999999999998224 ) ) ;
#40538 = CARTESIAN_POINT ( 'NONE',  ( 15.29062500061451679, 6.054752690667223547, 3.707466751127219781E-16 ) ) ;
#40539 = CARTESIAN_POINT ( 'NONE',  ( -8.484601909799255319E-16, 19.58749999999999858, 34.61880215351700940 ) ) ;
#40540 = FACE_OUTER_BOUND ( 'NONE', #31884, .T. ) ;
#40541 = CARTESIAN_POINT ( 'NONE',  ( 20.18437500061451573, 5.824947211148865298E-16, -4.756430356249998326 ) ) ;
#40542 = CARTESIAN_POINT ( 'NONE',  ( 9.290625000614515017, -3.027376345333610441, -5.243569643749999898 ) ) ;
#40543 = CARTESIAN_POINT ( 'NONE',  ( 27.79687500061451999, -3.027376345333610441, -5.243569643749999898 ) ) ;
#40544 = CARTESIAN_POINT ( 'NONE',  ( 19.53750000122903430, 6.123233995736764310E-16, -4.999999999999998224 ) ) ;
#40545 = CARTESIAN_POINT ( 'NONE',  ( 25.69687500061451502, 6.054752690667223547, 3.707466751127219781E-16 ) ) ;
#40546 = CARTESIAN_POINT ( 'NONE',  ( 7.162500000000001421, -5.773502691896255534, -1.060575238724906372E-15 ) ) ;
#40547 = CARTESIAN_POINT ( 'NONE',  ( -3.999999999999997335, 13.85000000122903607, 32.30940107675850470 ) ) ;
#40548 = CARTESIAN_POINT ( 'NONE',  ( 14.01562500061451644, 3.027376345333611329, 5.243569643749999010 ) ) ;
#40549 = CARTESIAN_POINT ( 'NONE',  ( 6.712500001229034119, 0.000000000000000000, 4.999999999999998224 ) ) ;
#40550 = CARTESIAN_POINT ( 'NONE',  ( 18.45937500061451431, 4.541064518000418104, -2.621784821874998173 ) ) ;
#40551 = CARTESIAN_POINT ( 'NONE',  ( 11.78437500061451892, 4.541064518000418104, 2.621784821874999949 ) ) ;
#40552 = CARTESIAN_POINT ( 'NONE',  ( -3.943440097865042571, 3.074283834720752839, -30.68362617565046335 ) ) ;
#40553 = VERTEX_POINT ( 'NONE', #12504 ) ;
#40554 = CARTESIAN_POINT ( 'NONE',  ( 12.96562500061451750, 3.027376345333613106, -5.243569643749998122 ) ) ;
#40555 = CARTESIAN_POINT ( 'NONE',  ( 25.31250000122903288, -4.330127018922190985, -2.500000000000001332 ) ) ;
#40556 = CARTESIAN_POINT ( 'NONE',  ( 12.30937500061451573, 0.000000000000000000, 5.243569643749999010 ) ) ;
#40557 = CARTESIAN_POINT ( 'NONE',  ( 4.027635003466097707, 2.962795348797195416, -4.326299380533228600 ) ) ;
#40558 = CARTESIAN_POINT ( 'NONE',  ( 14.20312500061451644, -4.541064518000417216, -2.621784821875001281 ) ) ;
#40559 = CARTESIAN_POINT ( 'NONE',  ( 29.53125000122903288, 4.330127018922191873, 2.499999999999999556 ) ) ;
#40560 = CARTESIAN_POINT ( 'NONE',  ( 22.92187500061451644, 3.027376345333613106, -5.243569643749998122 ) ) ;
#40561 = CARTESIAN_POINT ( 'NONE',  ( -4.243569643749999898, 10.31562500061451715, 27.54997392385601529 ) ) ;
#40562 = CARTESIAN_POINT ( 'NONE',  ( 10.83750000122903501, -4.330127018922194537, 2.499999999999995559 ) ) ;
#40563 = DIRECTION ( 'NONE',  ( -1.000000000000000000, -0.000000000000000000, -0.000000000000000000 ) ) ;
#40564 = CARTESIAN_POINT ( 'NONE',  ( 8.100000001229034297, -2.886751345948130876, 4.999999999999996447 ) ) ;
#40565 = CARTESIAN_POINT ( 'NONE',  ( 4.243569643749999010, 16.07187500061451857, -32.45002607614398471 ) ) ;
#40566 = CARTESIAN_POINT ( 'NONE',  ( 18.12187500061451573, 3.027376345333611329, 5.243569643749999010 ) ) ;
#40567 = CARTESIAN_POINT ( 'NONE',  ( 20.06250000122903643, 4.330127018922192761, -2.499999999999997780 ) ) ;
#40568 = CARTESIAN_POINT ( 'NONE',  ( 13.80937500061451750, -4.541064518000417216, -2.621784821875001281 ) ) ;
#40569 = CARTESIAN_POINT ( 'NONE',  ( 4.243569643749999898, 10.14687500061451786, 32.45002607614398471 ) ) ;
#40570 = CARTESIAN_POINT ( 'NONE',  ( 19.72500000122903074, 2.886751345948126879, 4.999999999999999112 ) ) ;
#40571 = CARTESIAN_POINT ( 'NONE',  ( 14.91562500061451679, 3.027376345333611329, 5.243569643749999010 ) ) ;
#40572 = ORIENTED_EDGE ( 'NONE', *, *, #67682, .T. ) ;
#40573 = ORIENTED_EDGE ( 'NONE', *, *, #60856, .T. ) ;
#40574 = CARTESIAN_POINT ( 'NONE',  ( 18.37500000000000355, -4.330127018922194537, 2.499999999999995559 ) ) ;
#40575 = CARTESIAN_POINT ( 'NONE',  ( 1.071796769724495002, 15.50134618820330168, 34.00000000000000000 ) ) ;
#40576 = CARTESIAN_POINT ( 'NONE',  ( 2.840625000614518392, -3.027376345333614438, 5.243569643749998122 ) ) ;
#40577 = CARTESIAN_POINT ( 'NONE',  ( 15.90000000122903501, -2.886751345948125991, -5.000000000000000000 ) ) ;
#40578 = CARTESIAN_POINT ( 'NONE',  ( 26.40937500061451715, -4.541064518000417216, -2.621784821875001281 ) ) ;
#40579 = CARTESIAN_POINT ( 'NONE',  ( 19.45312500061451644, 0.000000000000000000, 5.243569643749999010 ) ) ;
#40580 = EDGE_CURVE ( 'NONE', #26527, #31980, #38287, .T. ) ;
#40581 = CARTESIAN_POINT ( 'NONE',  ( 23.31562500061451715, 3.027376345333613106, -5.243569643749998122 ) ) ;
#40582 = CARTESIAN_POINT ( 'NONE',  ( 3.553125000614516082, 4.541064518000418104, -2.621784821874998173 ) ) ;
#40583 = CARTESIAN_POINT ( 'NONE',  ( 28.46249999999999858, 2.886751345948129099, -4.999999999999998224 ) ) ;
#40584 = CARTESIAN_POINT ( 'NONE',  ( 4.627512969954662658, 1.893775943066041245, 4.889672281578874902 ) ) ;
#40585 = CARTESIAN_POINT ( 'NONE',  ( 10.09687500061451715, -2.746126346562646425, 4.756430356249996549 ) ) ;
#40586 = CARTESIAN_POINT ( 'NONE',  ( 4.000000000000000000, 17.89999999999999858, 30.00000000000000000 ) ) ;
#40587 = CARTESIAN_POINT ( 'NONE',  ( 28.72500000000000142, -4.330127018922194537, 2.499999999999995559 ) ) ;
#40588 = CARTESIAN_POINT ( 'NONE',  ( 4.243569643749999898, 16.89687500061451786, -27.54997392385601529 ) ) ;
#40589 = CARTESIAN_POINT ( 'NONE',  ( 6.112500001229034474, 4.330127018922192761, -2.499999999999997780 ) ) ;
#40590 = CARTESIAN_POINT ( 'NONE',  ( 5.625000000000001776, 4.330127018922191873, 2.499999999999999556 ) ) ;
#40591 = CARTESIAN_POINT ( 'NONE',  ( 3.150000001229034119, -2.886751345948129988, 4.999999999999997335 ) ) ;
#40592 = CARTESIAN_POINT ( 'NONE',  ( 9.646875000614516082, -3.027376345333614438, 5.243569643749998122 ) ) ;
#40593 = DIRECTION ( 'NONE',  ( -1.000000000000000000, -0.000000000000000000, -0.000000000000000000 ) ) ;
#40594 = FACE_OUTER_BOUND ( 'NONE', #36423, .T. ) ;
#40595 = CARTESIAN_POINT ( 'NONE',  ( -5.989433049342593129, 8.007954590042437815, -30.40871493912334955 ) ) ;
#40596 = LINE ( 'NONE', #62039, #50139 ) ;
#40597 = CARTESIAN_POINT ( 'NONE',  ( 8.821875000614518569, -6.054752690667223547, -1.112240025338166033E-15 ) ) ;
#40598 = CARTESIAN_POINT ( 'NONE',  ( 14.70937500061451786, -4.541064518000417216, -2.621784821875001281 ) ) ;
#40599 = CARTESIAN_POINT ( 'NONE',  ( 6.299999999999999822, -4.330127018922190985, -2.500000000000001332 ) ) ;
#40600 = CARTESIAN_POINT ( 'NONE',  ( -4.243569643749999898, 16.16562500061459673, 27.54997392385601529 ) ) ;
#40601 = CARTESIAN_POINT ( 'NONE',  ( 20.52187500061451786, -6.054752690667223547, -1.112240025338166033E-15 ) ) ;
#40602 =( BOUNDED_CURVE ( )  B_SPLINE_CURVE ( 2, ( #42176, #42540, #25917, #65431, #31083, #14457, #3015 ),
 .UNSPECIFIED., .F., .F. ) 
 B_SPLINE_CURVE_WITH_KNOTS ( ( 3, 2, 2, 3 ),
 ( 0.3099999999999999978, 0.3133333333333333526, 0.3166666666666665964, 0.3199999999999999512 ),
 .UNSPECIFIED. ) 
 CURVE ( )  GEOMETRIC_REPRESENTATION_ITEM ( )  RATIONAL_B_SPLINE_CURVE ( ( 1.000000000000000000, 0.8660254037844387076, 1.000000000000000000, 0.8660254037844387076, 1.000000000000000000, 0.8660254037844409281, 0.9999999999999977796 ) ) 
 REPRESENTATION_ITEM ( '' )  );
#40603 = CARTESIAN_POINT ( 'NONE',  ( 2.841718689647413587, -4.113985430540962440, 3.174331389344874577 ) ) ;
#40604 = CARTESIAN_POINT ( 'NONE',  ( 26.55000000122902648, -2.886751345948129988, 4.999999999999997335 ) ) ;
#40605 = CARTESIAN_POINT ( 'NONE',  ( 18.27187500061451431, 5.824947211148865298E-16, -4.756430356249998326 ) ) ;
#40606 = CARTESIAN_POINT ( 'NONE',  ( 22.15312500061451573, 0.000000000000000000, 5.243569643749999010 ) ) ;
#40607 = CARTESIAN_POINT ( 'NONE',  ( 12.89062500061451821, -3.027376345333610441, -5.243569643749999898 ) ) ;
#40608 = CARTESIAN_POINT ( 'NONE',  ( 26.37187500061451573, 5.824947211148865298E-16, -4.756430356249998326 ) ) ;
#40609 = CARTESIAN_POINT ( 'NONE',  ( 10.99687500061451750, -3.027376345333614438, 5.243569643749998122 ) ) ;
#40610 = CARTESIAN_POINT ( 'NONE',  ( 28.12499999999999645, 4.330127018922191873, 2.499999999999999556 ) ) ;
#40611 = CARTESIAN_POINT ( 'NONE',  ( 23.47500000122903430, -5.773502691896255534, -1.060575238724906372E-15 ) ) ;
#40612 = AXIS2_PLACEMENT_3D ( 'NONE', #43959, #60927, #1075 ) ;
#40613 = DIRECTION ( 'NONE',  ( -0.000000000000000000, -1.000000000000000000, -0.000000000000000000 ) ) ;
#40614 = CARTESIAN_POINT ( 'NONE',  ( 11.29687500061451644, 6.054752690667223547, 3.707466751127219781E-16 ) ) ;
#40615 = CARTESIAN_POINT ( 'NONE',  ( 29.40937500061451715, 0.000000000000000000, 5.243569643749999010 ) ) ;
#40616 = CARTESIAN_POINT ( 'NONE',  ( 7.320879633048903241E-15, 18.20000000122903216, -34.00000000000000000 ) ) ;
#40617 = EDGE_CURVE ( 'NONE', #17518, #18233, #69395, .T. ) ;
#40618 = CARTESIAN_POINT ( 'NONE',  ( -3.137519842735245283E-14, 14.71250000000000213, 34.00000000000000000 ) ) ;
#40619 = CARTESIAN_POINT ( 'NONE',  ( 21.45937500061451786, -4.541064518000417216, -2.621784821875001281 ) ) ;
#40620 = CARTESIAN_POINT ( 'NONE',  ( 13.84687500061451537, -3.027376345333610441, -5.243569643749999898 ) ) ;
#40621 = EDGE_CURVE ( 'NONE', #48662, #26352, #25277, .T. ) ;
#40622 = CARTESIAN_POINT ( 'NONE',  ( 1.878215178125000495, 18.22812499938548214, 26.74683588394047007 ) ) ;
#40623 = CARTESIAN_POINT ( 'NONE',  ( 24.93750000000000355, 5.773502691896255534, 3.535250795749688894E-16 ) ) ;
#40624 = CARTESIAN_POINT ( 'NONE',  ( 0.6522896842281029617, 20.64114846093740852, 33.69936307885641469 ) ) ;
#40625 = CARTESIAN_POINT ( 'NONE',  ( 26.37187500061451217, -5.492252693125287522, -1.008910452111647106E-15 ) ) ;
#40626 = CARTESIAN_POINT ( 'NONE',  ( 16.67812500061451786, 4.541064518000418104, 2.621784821874999949 ) ) ;
#40627 = CARTESIAN_POINT ( 'NONE',  ( 7.575000000000001954, -4.330127018922194537, 2.499999999999995559 ) ) ;
#40628 = CARTESIAN_POINT ( 'NONE',  ( 0.000000000000000000, 20.00000000000000000, 30.00000000000000000 ) ) ;
#40629 = CARTESIAN_POINT ( 'NONE',  ( 14.69999999999999929, 0.000000000000000000, 4.999999999999998224 ) ) ;
#40630 = CARTESIAN_POINT ( 'NONE',  ( -4.243569643749997233, 10.39062500061451644, 32.45002607614398471 ) ) ;
#40631 = DIRECTION ( 'NONE',  ( -1.000000000000000000, -0.000000000000000000, -0.000000000000000000 ) ) ;
#40632 = CARTESIAN_POINT ( 'NONE',  ( 25.28437500061451715, 4.541064518000418104, 2.621784821874999949 ) ) ;
#40633 = ORIENTED_EDGE ( 'NONE', *, *, #5973, .T. ) ;
#40634 = CARTESIAN_POINT ( 'NONE',  ( 23.05312500061451431, 0.000000000000000000, 5.243569643749999010 ) ) ;
#40635 = CARTESIAN_POINT ( 'NONE',  ( 20.55937500061451573, -4.541064518000417216, -2.621784821875001281 ) ) ;
#40636 = CARTESIAN_POINT ( 'NONE',  ( 3.374999999999999556, 4.330127018922191873, 2.499999999999999556 ) ) ;
#40637 = CARTESIAN_POINT ( 'NONE',  ( 5.990625000614517859, -3.027376345333614438, 5.243569643749998122 ) ) ;
#40638 = CARTESIAN_POINT ( 'NONE',  ( 21.81562500061451004, -6.054752690667223547, -1.112240025338166033E-15 ) ) ;
#40639 = CARTESIAN_POINT ( 'NONE',  ( 13.24687500061451750, -3.027376345333614438, 5.243569643749998122 ) ) ;
#40640 = CARTESIAN_POINT ( 'NONE',  ( 17.44687500061451857, -3.027376345333610441, -5.243569643749999898 ) ) ;
#40641 = CARTESIAN_POINT ( 'NONE',  ( 2.121784821875001281, 18.15312500061451928, 33.67503911421598417 ) ) ;
#40642 = CARTESIAN_POINT ( 'NONE',  ( 18.71250000122903145, 4.330127018922192761, -2.499999999999997780 ) ) ;
#40643 = CARTESIAN_POINT ( 'NONE',  ( 15.68437500061451573, 5.824947211148865298E-16, -4.756430356249998326 ) ) ;
#40644 = CARTESIAN_POINT ( 'NONE',  ( 9.103125000614515017, 0.000000000000000000, 5.243569643749999010 ) ) ;
#40645 = CARTESIAN_POINT ( 'NONE',  ( 4.996875000614516615, 6.054752690667223547, 3.707466751127219781E-16 ) ) ;
#40646 = CARTESIAN_POINT ( 'NONE',  ( 3.946875000614517681, -3.027376345333610441, -5.243569643749999898 ) ) ;
#40647 = CARTESIAN_POINT ( 'NONE',  ( 25.92187500061451999, -6.054752690667223547, -1.112240025338166033E-15 ) ) ;
#40648 = CARTESIAN_POINT ( 'NONE',  ( 17.31562500061451715, -6.054752690667223547, -1.112240025338166033E-15 ) ) ;
#40649 = CARTESIAN_POINT ( 'NONE',  ( 28.08750000122903145, 6.123233995736764310E-16, -4.999999999999998224 ) ) ;
#40650 = CARTESIAN_POINT ( 'NONE',  ( 26.20312500061451644, 0.000000000000000000, 5.243569643749999010 ) ) ;
#40651 = CARTESIAN_POINT ( 'NONE',  ( 21.23437500061451644, 4.541064518000418104, 2.621784821874999949 ) ) ;
#40652 = CARTESIAN_POINT ( 'NONE',  ( 17.46562500061451217, 3.027376345333613106, -5.243569643749998122 ) ) ;
#40653 = CARTESIAN_POINT ( 'NONE',  ( 2.121784821875001281, 18.20937500061451786, 33.67503911421598417 ) ) ;
#40654 = CARTESIAN_POINT ( 'NONE',  ( 22.00312500061451360, 4.541064518000418104, -2.621784821874998173 ) ) ;
#40655 = CARTESIAN_POINT ( 'NONE',  ( 3.450000001229036162, 5.773502691896255534, 3.535250795749688894E-16 ) ) ;
#40656 = VERTEX_POINT ( 'NONE', #2872 ) ;
#40657 = CARTESIAN_POINT ( 'NONE',  ( 24.97499999999999787, 4.330127018922191873, 2.499999999999999556 ) ) ;
#40658 = CARTESIAN_POINT ( 'NONE',  ( -2.000000000000000000, 14.07500000000000107, -33.46410161513775705 ) ) ;
#40659 = CARTESIAN_POINT ( 'NONE',  ( -0.6941636114358130660, 20.72676549290719450, 33.93677660682192965 ) ) ;
#40660 = CARTESIAN_POINT ( 'NONE',  ( 28.19062500061451715, -3.027376345333610441, -5.243569643749999898 ) ) ;
#40661 = CARTESIAN_POINT ( 'NONE',  ( 10.00312500061451715, 0.000000000000000000, 5.243569643749999010 ) ) ;
#40662 = CARTESIAN_POINT ( 'NONE',  ( 22.61250000122903003, -4.330127018922190985, -2.500000000000001332 ) ) ;
#40663 =( BOUNDED_CURVE ( )  B_SPLINE_CURVE ( 2, ( #8050, #53480, #70474, #53854, #3246, #36122, #20211 ),
 .UNSPECIFIED., .F., .F. ) 
 B_SPLINE_CURVE_WITH_KNOTS ( ( 3, 2, 2, 3 ),
 ( 0.5300000000000000266, 0.5333333333333333259, 0.5366666666666667362, 0.5400000000000001465 ),
 .UNSPECIFIED. ) 
 CURVE ( )  GEOMETRIC_REPRESENTATION_ITEM ( )  RATIONAL_B_SPLINE_CURVE ( ( 1.000000000000000000, 0.8660254037844387076, 1.000000000000000000, 0.8660254037844387076, 1.000000000000000000, 0.8660254037844342667, 1.000000000000004441 ) ) 
 REPRESENTATION_ITEM ( '' )  );
#40664 = CARTESIAN_POINT ( 'NONE',  ( 26.95312500061451644, 4.541064518000418104, -2.621784821874998173 ) ) ;
#40665 = CARTESIAN_POINT ( 'NONE',  ( 27.97500000000000142, 6.123233995736764310E-16, -4.999999999999998224 ) ) ;
#40666 = CARTESIAN_POINT ( 'NONE',  ( 3.999999999999998668, 16.77500000122903145, -32.30940107675850470 ) ) ;
#40667 = DIRECTION ( 'NONE',  ( 0.000000000000000000, 0.000000000000000000, 1.000000000000000000 ) ) ;
#40668 = CARTESIAN_POINT ( 'NONE',  ( 9.928125000614517859, 4.541064518000418104, 2.621784821874999949 ) ) ;
#40669 = VERTEX_POINT ( 'NONE', #42036 ) ;
#40670 = CARTESIAN_POINT ( 'NONE',  ( 26.05312500061451431, 4.541064518000418104, -2.621784821874998173 ) ) ;
#40671 = CARTESIAN_POINT ( 'NONE',  ( 7.040625000614517681, -3.027376345333610441, -5.243569643749999898 ) ) ;
#40672 = AXIS2_PLACEMENT_3D ( 'NONE', #33774, #5706, #22681 ) ;
#40673 = CARTESIAN_POINT ( 'NONE',  ( 6.178125000614518747, 6.421520780324663323E-16, -5.243569643749999010 ) ) ;
#40674 = CARTESIAN_POINT ( 'NONE',  ( 15.83437500061451608, 4.119189519843966529, 2.378215178124999607 ) ) ;
#40675 = FACE_BOUND ( 'NONE', #59126, .T. ) ;
#40676 = CARTESIAN_POINT ( 'NONE',  ( 16.57499999999999929, -4.330127018922194537, 2.499999999999995559 ) ) ;
#40677 =( BOUNDED_CURVE ( )  B_SPLINE_CURVE ( 2, ( #62257, #35261, #6106, #51899, #24537, #12009, #63339, #58142, #1297, #7548, #57428, #51541, #51175, #18619, #68892, #18249, #34532, #34900, #46722, #29720, #11654, #40822, #12725, #69257, #6832, #57783, #579, #57062, #2026, #23449, #23807, #40453, #34169, #45642, #46358, #942, #7192, #41184, #68532, #63693, #29004, #13084, #35622, #40099, #17893, #30082, #6469, #23084, #52620, #18977, #68174, #17537, #2377, #64788, #65525, #20073, #71069, #65153, #14179, #59235, #64056, #13436, #26369, #31547, #3107, #35986, #20444, #47440, #54087, #54449, #36713, #48542, #71440, #24895, #30810, #14543, #53343, #8643, #2741, #64424, #30452, #31172, #25260, #69972, #42629, #3848, #53715, #25636, #42994, #48909, #8280, #41538, #37079, #58505, #48174, #7915, #13816, #59603, #37453, #70698, #59972, #9017, #3485, #26003, #14911, #9381, #31913, #52981, #19342, #41897, #36356, #47807, #58870, #70336, #19713, #42265, #55183, #10475, #21547, #27843, #38175, #55905, #32642, #66628, #39286, #72168, #55543, #60699, #60333, #11203, #21180, #33730, #15274, #4578, #4939, #5297, #44474, #28201, #10112, #56276, #33369, #61077, #33004, #37813, #43732, #61800, #27108, #72530, #27473, #50374, #50005, #22281, #71810, #49641, #16366, #15634, #9742, #21918, #50730, #67005, #38921, #5665, #66256, #20815, #72899, #10833, #61440, #44102, #16005, #32276, #65894, #43370, #44833, #67368, #54810, #16731, #26744, #4216, #49277, #38554, #7104, #45908, #29633, #51808, #40362, #11922, #56975, #28912, #62881, #6019, #68439, #62525, #28554, #1211, #12997, #23360, #12277, #52171, #7463, #40011, #133, #29989, #34809, #57699, #63607, #57340, #34447, #12640, #17453, #58054, #68806, #40731, #6745, #18162, #1573, #29278, #67720, #63246, #39653, #51089, #6379, #23717, #485, #24082, #51450, #46267, #853, #46629, #17802, #35175, #69171, #18531, #35533, #41096, #22638, #62172, #45188, #22995, #11569, #17093, #34084, #56625, #45555, #68086, #3018, #59890, #69885, #14825, #65069, #24807, #53254, #14461, #19990, #52531, #25549, #42911, #59517, #70251, #2653, #9295, #58784, #65434, #13728, #47712, #30722, #42543, #37367, #25171, #8930, #1939, #35892, #41805, #48092, #64336, #19623, #36270, #2291, #41450, #31460, #8194, #42180, #53626, #24445, #64705, #14089, #54003, #46993, #19250, #69529, #70616, #18888, #36629, #63968, #47352, #36994, #48460, #59150, #70984, #8559, #31087, #13351, #3399, #25920, #20360, #58416, #7829, #30365, #52894, #43648, #43286, #66537, #60246, #61355, #66172, #21460, #32559, #38840, #49194, #27026, #15548, #4852, #50290, #10023, #15917, #71727, #71353, #22197, #32194, #44751, #26285, #38091, #38465, #66916, #55460, #39200, #21097, #67285, #44391, #4130, #55097, #16285, #60991, #60614, #10390, #32922, #72442, #4497, #27386, #48822, #26660, #16644, #49557, #72078, #44015, #3761, #15188, #49918, #21826, #10752, #33283, #55822, #5210, #27751, #72814, #61714, #9660, #31828, #54366, #20727, #65806, #37726, #54727, #51363, #45823, #45102, #34358, #35092, #62801, #40643, #34721, #56890, #45465, #5579, #56186, #69087, #1128, #68359, #28116, #63162, #17004, #39927, #765, #39561, #6295, #399, #62086, #12194, #23998, #28824, #23273, #12557, #17720, #6665, #67997, #18448, #40280, #68722, #1492, #57251, #51001, #23637, #28466, #41013, #29193, #51727, #46183, #18082, #57617, #7020, #50645, #29551, #17370, #11113, #52087, #46546, #33642, #49, #22554, #67638, #11479, #34002, #56539, #5932, #22907, #62441, #11839, #8839, #41723, #25087, #30278, #29910, #52450, #36182, #2934, #70900, #2211, #70163, #2567, #47269, #58331, #58700, #7742, #42098, #19540, #57972, #30638, #64620, #69803, #14007, #36545, #31005, #64250, #20272, #19169, #8110, #13638, #53170, #47630, #19910, #59065, #8470, #7379, #63880, #31375, #52810, #53538, #25463, #48007, #70535, #64985, #41370, #42463, #14376, #12915, #36911, #59431, #1856, #53916, #24363, #3309, #13271, #63528, #25836, #48373, #35448, #35809, #24726, #46910, #69449, #18806, #32839, #4770, #71261, #60903, #9574, #27303, #20641, #26199, #32476, #15464, #49837, #21377, #9938, #54639, #26569, #49110, #37641, #38009, #60164, #43931, #49469, #55009, #72002, #71639, #66457, #15834, #10306, #66086, #38379, #37280, #15105, #55738, #4044, #60531, #21012, #14738, #48738, #26944, #32106, #55376, #72361, #21742, #44303, #66832, #16204, #38755, #43199, #43564, #61276, #4415, #59802, #10669, #50205, #33199, #5132, #3675, #27666, #72730, #42824, #65348, #9208, #65719, #31743, #54281, #67201, #6942, #12118, #56809, #16563, #1049, #28035, #34642, #35011, #67917, #29114, #52010, #5496, #11400, #45746, #33919, #39850, #50922, #62363, #50564, #17288, #56462, #73091, #23192, #57541, #45381, #11760, #23558, #29473, #61999, #22114, #68282, #39114, #34277, #44671, #45023, #17643 ),
 .UNSPECIFIED., .F., .F. ) 
 B_SPLINE_CURVE_WITH_KNOTS ( ( 3, 2, 2, 2, 2, 2, 2, 2, 2, 2, 2, 2, 2, 2, 2, 2, 2, 2, 2, 2, 2, 2, 2, 2, 2, 2, 2, 2, 2, 2, 2, 2, 2, 2, 2, 2, 2, 2, 2, 2, 2, 2, 2, 2, 2, 2, 2, 2, 2, 2, 2, 2, 2, 2, 2, 2, 2, 2, 2, 2, 2, 2, 2, 2, 2, 2, 2, 2, 2, 2, 2, 2, 2, 2, 2, 2, 2, 2, 2, 2, 2, 2, 2, 2, 2, 2, 2, 2, 2, 2, 2, 2, 2, 2, 2, 2, 2, 2, 2, 2, 2, 2, 2, 2, 2, 2, 2, 2, 2, 2, 2, 2, 2, 2, 2, 2, 2, 2, 2, 2, 2, 2, 2, 2, 2, 2, 2, 2, 2, 2, 2, 2, 2, 2, 2, 2, 2, 2, 2, 2, 2, 2, 2, 2, 2, 2, 2, 2, 2, 2, 2, 2, 2, 2, 2, 2, 2, 2, 2, 2, 2, 2, 2, 2, 2, 2, 2, 2, 2, 2, 2, 2, 2, 2, 2, 2, 2, 2, 2, 2, 2, 2, 2, 2, 2, 2, 2, 2, 2, 2, 2, 2, 2, 2, 2, 2, 2, 2, 2, 2, 2, 2, 2, 2, 2, 2, 2, 2, 2, 2, 2, 2, 2, 2, 2, 2, 2, 2, 2, 2, 2, 2, 2, 2, 2, 2, 2, 2, 2, 2, 2, 2, 2, 2, 2, 2, 2, 2, 2, 2, 2, 2, 2, 2, 2, 2, 2, 2, 2, 2, 2, 2, 2, 2, 2, 2, 2, 2, 2, 2, 2, 2, 2, 2, 2, 2, 2, 2, 2, 2, 2, 2, 2, 2, 2, 2, 2, 2, 2, 2, 2, 2, 2, 2, 2, 2, 2, 2, 2, 2, 2, 2, 2, 2, 2, 2, 2, 2, 2, 2, 3 ),
 ( 0.000000000000000000, 0.003333333333333333547, 0.006666666666666667095, 0.01000000000000000021, 0.01333333333333333419, 0.01666666666666666644, 0.02000000000000000042, 0.02333333333333333440, 0.02666666666666666838, 0.02999999999999999889, 0.03333333333333333287, 0.03666666666666666685, 0.04000000000000000083, 0.04333333333333333481, 0.04666666666666666879, 0.05000000000000000278, 0.05333333333333333676, 0.05666666666666666380, 0.05999999999999999778, 0.06333333333333333870, 0.06666666666666666574, 0.07000000000000000666, 0.07333333333333333370, 0.07666666666666666075, 0.08000000000000000167, 0.08333333333333332871, 0.08666666666666666963, 0.08999999999999999667, 0.09333333333333333759, 0.09666666666666666463, 0.1000000000000000056, 0.1033333333333333326, 0.1066666666666666735, 0.1100000000000000006, 0.1133333333333333276, 0.1166666666666666685, 0.1199999999999999956, 0.1233333333333333365, 0.1266666666666666774, 0.1300000000000000044, 0.1333333333333333315, 0.1366666666666666585, 0.1400000000000000133, 0.1433333333333333404, 0.1466666666666666674, 0.1499999999999999944, 0.1533333333333333215, 0.1566666666666666763, 0.1600000000000000033, 0.1633333333333333304, 0.1666666666666666574, 0.1700000000000000122, 0.1733333333333333393, 0.1766666666666666663, 0.1799999999999999933, 0.1833333333333333204, 0.1866666666666666752, 0.1900000000000000022, 0.1933333333333333293, 0.1966666666666666563, 0.2000000000000000111, 0.2033333333333333381, 0.2066666666666666652, 0.2099999999999999922, 0.2133333333333333470, 0.2166666666666666741, 0.2200000000000000011, 0.2233333333333333282, 0.2266666666666666552, 0.2300000000000000100, 0.2333333333333333370, 0.2366666666666666641, 0.2399999999999999911, 0.2433333333333333459, 0.2466666666666666730, 0.2500000000000000000, 0.2533333333333333548, 0.2566666666666666541, 0.2600000000000000089, 0.2633333333333333082, 0.2666666666666666630, 0.2700000000000000178, 0.2733333333333333171, 0.2766666666666666718, 0.2800000000000000266, 0.2833333333333333259, 0.2866666666666666807, 0.2899999999999999800, 0.2933333333333333348, 0.2966666666666666896, 0.2999999999999999889, 0.3033333333333333437, 0.3066666666666666430, 0.3099999999999999978, 0.3133333333333333526, 0.3166666666666666519, 0.3200000000000000067, 0.3233333333333333059, 0.3266666666666666607, 0.3300000000000000155, 0.3333333333333333148, 0.3366666666666666696, 0.3400000000000000244, 0.3433333333333333237, 0.3466666666666666785, 0.3499999999999999778, 0.3533333333333333326, 0.3566666666666666874, 0.3599999999999999867, 0.3633333333333333415, 0.3666666666666666408, 0.3699999999999999956, 0.3733333333333333504, 0.3766666666666666496, 0.3800000000000000044, 0.3833333333333333592, 0.3866666666666666585, 0.3900000000000000133, 0.3933333333333333126, 0.3966666666666666674, 0.4000000000000000222, 0.4033333333333333215, 0.4066666666666666763, 0.4099999999999999756, 0.4133333333333333304, 0.4166666666666666852, 0.4199999999999999845, 0.4233333333333333393, 0.4266666666666666941, 0.4299999999999999933, 0.4333333333333333481, 0.4366666666666666474, 0.4400000000000000022, 0.4433333333333333570, 0.4466666666666666563, 0.4500000000000000111, 0.4533333333333333104, 0.4566666666666666652, 0.4600000000000000200, 0.4633333333333333193, 0.4666666666666666741, 0.4699999999999999734, 0.4733333333333333282, 0.4766666666666666829, 0.4799999999999999822, 0.4833333333333333370, 0.4866666666666666918, 0.4899999999999999911, 0.4933333333333333459, 0.4966666666666666452, 0.5000000000000000000, 0.5033333333333332993, 0.5066666666666667096, 0.5100000000000000089, 0.5133333333333333082, 0.5166666666666667185, 0.5200000000000000178, 0.5233333333333333171, 0.5266666666666666163, 0.5300000000000000266, 0.5333333333333333259, 0.5366666666666666252, 0.5400000000000000355, 0.5433333333333333348, 0.5466666666666666341, 0.5500000000000000444, 0.5533333333333333437, 0.5566666666666666430, 0.5600000000000000533, 0.5633333333333333526, 0.5666666666666666519, 0.5699999999999999512, 0.5733333333333333615, 0.5766666666666666607, 0.5799999999999999600, 0.5833333333333333703, 0.5866666666666666696, 0.5899999999999999689, 0.5933333333333333792, 0.5966666666666666785, 0.5999999999999999778, 0.6033333333333333881, 0.6066666666666666874, 0.6099999999999999867, 0.6133333333333332860, 0.6166666666666666963, 0.6199999999999999956, 0.6233333333333332948, 0.6266666666666667052, 0.6300000000000000044, 0.6333333333333333037, 0.6366666666666667140, 0.6400000000000000133, 0.6433333333333333126, 0.6466666666666666119, 0.6500000000000000222, 0.6533333333333333215, 0.6566666666666666208, 0.6600000000000000311, 0.6633333333333333304, 0.6666666666666666297, 0.6700000000000000400, 0.6733333333333333393, 0.6766666666666666385, 0.6800000000000000488, 0.6833333333333333481, 0.6866666666666666474, 0.6899999999999999467, 0.6933333333333333570, 0.6966666666666666563, 0.6999999999999999556, 0.7033333333333333659, 0.7066666666666666652, 0.7099999999999999645, 0.7133333333333333748, 0.7166666666666666741, 0.7199999999999999734, 0.7233333333333333837, 0.7266666666666666829, 0.7299999999999999822, 0.7333333333333332815, 0.7366666666666666918, 0.7399999999999999911, 0.7433333333333332904, 0.7466666666666667007, 0.7500000000000000000, 0.7533333333333332993, 0.7566666666666667096, 0.7600000000000000089, 0.7633333333333333082, 0.7666666666666667185, 0.7700000000000000178, 0.7733333333333333171, 0.7766666666666666163, 0.7800000000000000266, 0.7833333333333333259, 0.7866666666666666252, 0.7900000000000000355, 0.7933333333333333348, 0.7966666666666666341, 0.8000000000000000444, 0.8033333333333333437, 0.8066666666666666430, 0.8100000000000000533, 0.8133333333333333526, 0.8166666666666666519, 0.8199999999999999512, 0.8233333333333333615, 0.8266666666666666607, 0.8299999999999999600, 0.8333333333333333703, 0.8366666666666666696, 0.8399999999999999689, 0.8433333333333333792, 0.8466666666666666785, 0.8499999999999999778, 0.8533333333333333881, 0.8566666666666666874, 0.8599999999999999867, 0.8633333333333332860, 0.8666666666666666963, 0.8699999999999999956, 0.8733333333333332948, 0.8766666666666667052, 0.8800000000000000044, 0.8833333333333333037, 0.8866666666666667140, 0.8900000000000000133, 0.8933333333333333126, 0.8966666666666666119, 0.9000000000000000222, 0.9033333333333333215, 0.9066666666666666208, 0.9100000000000000311, 0.9133333333333333304, 0.9166666666666666297, 0.9200000000000000400, 0.9233333333333333393, 0.9266666666666666385, 0.9300000000000000488, 0.9333333333333333481, 0.9366666666666666474, 0.9399999999999999467, 0.9433333333333333570, 0.9466666666666666563, 0.9499999999999999556, 0.9533333333333333659, 0.9566666666666666652, 0.9599999999999999645, 0.9633333333333333748, 0.9666666666666666741, 0.9699999999999999734, 0.9733333333333333837, 0.9766666666666666829, 0.9799999999999999822, 0.9833333333333332815, 0.9866666666666666918, 0.9899999999999999911, 0.9933333333333332904, 0.9966666666666667007, 1.000000000000000000 ),
 .UNSPECIFIED. ) 
 CURVE ( )  GEOMETRIC_REPRESENTATION_ITEM ( )  RATIONAL_B_SPLINE_CURVE ( ( 1.000000000000000000, 0.8660254037844387076, 1.000000000000000000, 0.8660254037844387076, 1.000000000000000000, 0.8660254037844387076, 1.000000000000000000, 0.8660254037844387076, 1.000000000000000000, 0.8660254037844387076, 1.000000000000000000, 0.8660254037844387076, 1.000000000000000000, 0.8660254037844387076, 1.000000000000000000, 0.8660254037844387076, 1.000000000000000000, 0.8660254037844387076, 1.000000000000000000, 0.8660254037844387076, 1.000000000000000000, 0.8660254037844387076, 1.000000000000000000, 0.8660254037844387076, 1.000000000000000000, 0.8660254037844387076, 1.000000000000000000, 0.8660254037844387076, 1.000000000000000000, 0.8660254037844387076, 1.000000000000000000, 0.8660254037844387076, 1.000000000000000000, 0.8660254037844387076, 1.000000000000000000, 0.8660254037844387076, 1.000000000000000000, 0.8660254037844387076, 1.000000000000000000, 0.8660254037844387076, 1.000000000000000000, 0.8660254037844387076, 1.000000000000000000, 0.8660254037844387076, 1.000000000000000000, 0.8660254037844387076, 1.000000000000000000, 0.8660254037844387076, 1.000000000000000000, 0.8660254037844387076, 1.000000000000000000, 0.8660254037844387076, 1.000000000000000000, 0.8660254037844387076, 1.000000000000000000, 0.8660254037844387076, 1.000000000000000000, 0.8660254037844387076, 1.000000000000000000, 0.8660254037844387076, 1.000000000000000000, 0.8660254037844387076, 1.000000000000000000, 0.8660254037844387076, 1.000000000000000000, 0.8660254037844387076, 1.000000000000000000, 0.8660254037844387076, 1.000000000000000000, 0.8660254037844387076, 1.000000000000000000, 0.8660254037844387076, 1.000000000000000000, 0.8660254037844387076, 1.000000000000000000, 0.8660254037844387076, 1.000000000000000000, 0.8660254037844387076, 1.000000000000000000, 0.8660254037844387076, 1.000000000000000000, 0.8660254037844387076, 1.000000000000000000, 0.8660254037844387076, 1.000000000000000000, 0.8660254037844387076, 1.000000000000000000, 0.8660254037844387076, 1.000000000000000000, 0.8660254037844387076, 1.000000000000000000, 0.8660254037844387076, 1.000000000000000000, 0.8660254037844387076, 1.000000000000000000, 0.8660254037844387076, 1.000000000000000000, 0.8660254037844387076, 1.000000000000000000, 0.8660254037844387076, 1.000000000000000000, 0.8660254037844387076, 1.000000000000000000, 0.8660254037844387076, 1.000000000000000000, 0.8660254037844387076, 1.000000000000000000, 0.8660254037844387076, 1.000000000000000000, 0.8660254037844387076, 1.000000000000000000, 0.8660254037844387076, 1.000000000000000000, 0.8660254037844387076, 1.000000000000000000, 0.8660254037844387076, 1.000000000000000000, 0.8660254037844387076, 1.000000000000000000, 0.8660254037844387076, 1.000000000000000000, 0.8660254037844387076, 1.000000000000000000, 0.8660254037844387076, 1.000000000000000000, 0.8660254037844387076, 1.000000000000000000, 0.8660254037844387076, 1.000000000000000000, 0.8660254037844387076, 1.000000000000000000, 0.8660254037844387076, 1.000000000000000000, 0.8660254037844387076, 1.000000000000000000, 0.8660254037844387076, 1.000000000000000000, 0.8660254037844387076, 1.000000000000000000, 0.8660254037844387076, 1.000000000000000000, 0.8660254037844387076, 1.000000000000000000, 0.8660254037844387076, 1.000000000000000000, 0.8660254037844387076, 1.000000000000000000, 0.8660254037844387076, 1.000000000000000000, 0.8660254037844387076, 1.000000000000000000, 0.8660254037844387076, 1.000000000000000000, 0.8660254037844387076, 1.000000000000000000, 0.8660254037844387076, 1.000000000000000000, 0.8660254037844387076, 1.000000000000000000, 0.8660254037844387076, 1.000000000000000000, 0.8660254037844387076, 1.000000000000000000, 0.8660254037844387076, 1.000000000000000000, 0.8660254037844387076, 1.000000000000000000, 0.8660254037844387076, 1.000000000000000000, 0.8660254037844387076, 1.000000000000000000, 0.8660254037844387076, 1.000000000000000000, 0.8660254037844387076, 1.000000000000000000, 0.8660254037844387076, 1.000000000000000000, 0.8660254037844387076, 1.000000000000000000, 0.8660254037844387076, 1.000000000000000000, 0.8660254037844387076, 1.000000000000000000, 0.8660254037844387076, 1.000000000000000000, 0.8660254037844387076, 1.000000000000000000, 0.8660254037844387076, 1.000000000000000000, 0.8660254037844387076, 1.000000000000000000, 0.8660254037844387076, 1.000000000000000000, 0.8660254037844387076, 1.000000000000000000, 0.8660254037844387076, 1.000000000000000000, 0.8660254037844387076, 1.000000000000000000, 0.8660254037844387076, 1.000000000000000000, 0.8660254037844387076, 1.000000000000000000, 0.8660254037844387076, 1.000000000000000000, 0.8660254037844387076, 1.000000000000000000, 0.8660254037844387076, 1.000000000000000000, 0.8660254037844387076, 1.000000000000000000, 0.8660254037844387076, 1.000000000000000000, 0.8660254037844387076, 1.000000000000000000, 0.8660254037844387076, 1.000000000000000000, 0.8660254037844387076, 1.000000000000000000, 0.8660254037844387076, 1.000000000000000000, 0.8660254037844387076, 1.000000000000000000, 0.8660254037844387076, 1.000000000000000000, 0.8660254037844387076, 1.000000000000000000, 0.8660254037844387076, 1.000000000000000000, 0.8660254037844387076, 1.000000000000000000, 0.8660254037844387076, 1.000000000000000000, 0.8660254037844387076, 1.000000000000000000, 0.8660254037844387076, 1.000000000000000000, 0.8660254037844387076, 1.000000000000000000, 0.8660254037844387076, 1.000000000000000000, 0.8660254037844387076, 1.000000000000000000, 0.8660254037844387076, 1.000000000000000000, 0.8660254037844387076, 1.000000000000000000, 0.8660254037844387076, 1.000000000000000000, 0.8660254037844387076, 1.000000000000000000, 0.8660254037844387076, 1.000000000000000000, 0.8660254037844387076, 1.000000000000000000, 0.8660254037844387076, 1.000000000000000000, 0.8660254037844387076, 1.000000000000000000, 0.8660254037844387076, 1.000000000000000000, 0.8660254037844387076, 1.000000000000000000, 0.8660254037844387076, 1.000000000000000000, 0.8660254037844387076, 1.000000000000000000, 0.8660254037844387076, 1.000000000000000000, 0.8660254037844387076, 1.000000000000000000, 0.8660254037844387076, 1.000000000000000000, 0.8660254037844387076, 1.000000000000000000, 0.8660254037844387076, 1.000000000000000000, 0.8660254037844387076, 1.000000000000000000, 0.8660254037844387076, 1.000000000000000000, 0.8660254037844387076, 1.000000000000000000, 0.8660254037844387076, 1.000000000000000000, 0.8660254037844387076, 1.000000000000000000, 0.8660254037844387076, 1.000000000000000000, 0.8660254037844387076, 1.000000000000000000, 0.8660254037844387076, 1.000000000000000000, 0.8660254037844387076, 1.000000000000000000, 0.8660254037844387076, 1.000000000000000000, 0.8660254037844387076, 1.000000000000000000, 0.8660254037844387076, 1.000000000000000000, 0.8660254037844387076, 1.000000000000000000, 0.8660254037844387076, 1.000000000000000000, 0.8660254037844387076, 1.000000000000000000, 0.8660254037844387076, 1.000000000000000000, 0.8660254037844387076, 1.000000000000000000, 0.8660254037844387076, 1.000000000000000000, 0.8660254037844387076, 1.000000000000000000, 0.8660254037844387076, 1.000000000000000000, 0.8660254037844387076, 1.000000000000000000, 0.8660254037844387076, 1.000000000000000000, 0.8660254037844387076, 1.000000000000000000, 0.8660254037844387076, 1.000000000000000000, 0.8660254037844387076, 1.000000000000000000, 0.8660254037844387076, 1.000000000000000000, 0.8660254037844387076, 1.000000000000000000, 0.8660254037844387076, 1.000000000000000000, 0.8660254037844387076, 1.000000000000000000, 0.8660254037844387076, 1.000000000000000000, 0.8660254037844387076, 1.000000000000000000, 0.8660254037844387076, 1.000000000000000000, 0.8660254037844387076, 1.000000000000000000, 0.8660254037844387076, 1.000000000000000000, 0.8660254037844387076, 1.000000000000000000, 0.8660254037844387076, 1.000000000000000000, 0.8660254037844387076, 1.000000000000000000, 0.8660254037844387076, 1.000000000000000000, 0.8660254037844387076, 1.000000000000000000, 0.8660254037844387076, 1.000000000000000000, 0.8660254037844387076, 1.000000000000000000, 0.8660254037844387076, 1.000000000000000000, 0.8660254037844387076, 1.000000000000000000, 0.8660254037844387076, 1.000000000000000000, 0.8660254037844387076, 1.000000000000000000, 0.8660254037844387076, 1.000000000000000000, 0.8660254037844387076, 1.000000000000000000, 0.8660254037844387076, 1.000000000000000000, 0.8660254037844387076, 1.000000000000000000, 0.8660254037844387076, 1.000000000000000000, 0.8660254037844387076, 1.000000000000000000, 0.8660254037844387076, 1.000000000000000000, 0.8660254037844387076, 1.000000000000000000, 0.8660254037844387076, 1.000000000000000000, 0.8660254037844387076, 1.000000000000000000, 0.8660254037844387076, 1.000000000000000000, 0.8660254037844387076, 1.000000000000000000, 0.8660254037844387076, 1.000000000000000000, 0.8660254037844387076, 1.000000000000000000, 0.8660254037844387076, 1.000000000000000000, 0.8660254037844387076, 1.000000000000000000, 0.8660254037844387076, 1.000000000000000000, 0.8660254037844387076, 1.000000000000000000, 0.8660254037844387076, 1.000000000000000000, 0.8660254037844387076, 1.000000000000000000, 0.8660254037844387076, 1.000000000000000000, 0.8660254037844387076, 1.000000000000000000, 0.8660254037844387076, 1.000000000000000000, 0.8660254037844387076, 1.000000000000000000, 0.8660254037844387076, 1.000000000000000000, 0.8660254037844387076, 1.000000000000000000, 0.8660254037844387076, 1.000000000000000000, 0.8660254037844387076, 1.000000000000000000, 0.8660254037844387076, 1.000000000000000000, 0.8660254037844387076, 1.000000000000000000, 0.8660254037844387076, 1.000000000000000000, 0.8660254037844387076, 1.000000000000000000, 0.8660254037844387076, 1.000000000000000000, 0.8660254037844387076, 1.000000000000000000, 0.8660254037844387076, 1.000000000000000000, 0.8660254037844387076, 1.000000000000000000, 0.8660254037844387076, 1.000000000000000000, 0.8660254037844387076, 1.000000000000000000, 0.8660254037844387076, 1.000000000000000000, 0.8660254037844387076, 1.000000000000000000, 0.8660254037844387076, 1.000000000000000000, 0.8660254037844387076, 1.000000000000000000, 0.8660254037844387076, 1.000000000000000000, 0.8660254037844387076, 1.000000000000000000, 0.8660254037844387076, 1.000000000000000000, 0.8660254037844387076, 1.000000000000000000, 0.8660254037844387076, 1.000000000000000000, 0.8660254037844387076, 1.000000000000000000, 0.8660254037844387076, 1.000000000000000000, 0.8660254037844387076, 1.000000000000000000, 0.8660254037844387076, 1.000000000000000000, 0.8660254037844387076, 1.000000000000000000, 0.8660254037844387076, 1.000000000000000000, 0.8660254037844387076, 1.000000000000000000, 0.8660254037844387076, 1.000000000000000000, 0.8660254037844387076, 1.000000000000000000, 0.8660254037844387076, 1.000000000000000000, 0.8660254037844387076, 1.000000000000000000, 0.8660254037844387076, 1.000000000000000000, 0.8660254037844387076, 1.000000000000000000, 0.8660254037844387076, 1.000000000000000000, 0.8660254037844387076, 1.000000000000000000, 0.8660254037844387076, 1.000000000000000000, 0.8660254037844387076, 1.000000000000000000, 0.8660254037844387076, 1.000000000000000000, 0.8660254037844387076, 1.000000000000000000, 0.8660254037844387076, 1.000000000000000000, 0.8660254037844387076, 1.000000000000000000, 0.8660254037844387076, 1.000000000000000000, 0.8660254037844387076, 1.000000000000000000, 0.8660254037844387076, 1.000000000000000000, 0.8660254037844387076, 1.000000000000000000, 0.8660254037844387076, 1.000000000000000000, 0.8660254037844387076, 1.000000000000000000, 0.8660254037844387076, 1.000000000000000000, 0.8660254037844387076, 1.000000000000000000, 0.8660254037844387076, 1.000000000000000000, 0.8660254037844387076, 1.000000000000000000, 0.8660254037844387076, 1.000000000000000000, 0.8660254037844387076, 1.000000000000000000, 0.8660254037844387076, 1.000000000000000000, 0.8660254037844387076, 1.000000000000000000, 0.8660254037844387076, 1.000000000000000000, 0.8660254037844387076, 1.000000000000000000, 0.8660254037844387076, 1.000000000000000000, 0.8660254037844387076, 1.000000000000000000, 0.8660254037844387076, 1.000000000000000000, 0.8660254037844387076, 1.000000000000000000, 0.8660254037844387076, 1.000000000000000000, 0.8660254037844387076, 1.000000000000000000, 0.8660254037844387076, 1.000000000000000000, 0.8660254037844387076, 1.000000000000000000, 0.8660254037844387076, 1.000000000000000000, 0.8660254037844387076, 1.000000000000000000, 0.8660254037844387076, 1.000000000000000000, 0.8660254037844387076, 1.000000000000000000, 0.8660254037844387076, 1.000000000000000000, 0.8660254037844387076, 1.000000000000000000, 0.8660254037844387076, 1.000000000000000000, 0.8660254037844387076, 1.000000000000000000, 0.8660254037844387076, 1.000000000000000000, 0.8660254037844387076, 1.000000000000000000, 0.8660254037844387076, 1.000000000000000000, 0.8660254037844387076, 1.000000000000000000, 0.8660254037844387076, 1.000000000000000000, 0.8660254037844387076, 1.000000000000000000, 0.8660254037844387076, 1.000000000000000000, 0.8660254037844387076, 1.000000000000000000, 0.8660254037844387076, 1.000000000000000000, 0.8660254037844387076, 1.000000000000000000, 0.8660254037844387076, 1.000000000000000000, 0.8660254037844387076, 1.000000000000000000, 0.8660254037844387076, 1.000000000000000000, 0.8660254037844387076, 1.000000000000000000, 0.8660254037844387076, 1.000000000000000000, 0.8660254037844387076, 1.000000000000000000, 0.8660254037844387076, 1.000000000000000000 ) ) 
 REPRESENTATION_ITEM ( '' )  );
#40679 = CARTESIAN_POINT ( 'NONE',  ( 13.80937500061451750, -4.541064518000417216, -2.621784821875001281 ) ) ;
#40678 = VECTOR ( 'NONE', #20907, 1000.000000000000000 ) ;
#40680 = CARTESIAN_POINT ( 'NONE',  ( 10.72500000122903252, 2.886751345948126879, 4.999999999999999112 ) ) ;
#40681 = CARTESIAN_POINT ( 'NONE',  ( 15.90937500061451892, 0.000000000000000000, 5.243569643749999010 ) ) ;
#40682 = CARTESIAN_POINT ( 'NONE',  ( 17.10000000000000142, -4.330127018922190985, -2.500000000000001332 ) ) ;
#40683 = CARTESIAN_POINT ( 'NONE',  ( 22.05937500061451573, 4.541064518000418104, -2.621784821874998173 ) ) ;
#40684 = CARTESIAN_POINT ( 'NONE',  ( -2.121784821874999949, 12.07812500061451821, -33.67503911421598417 ) ) ;
#40685 = AXIS2_PLACEMENT_3D ( 'NONE', #5165, #16594, #39147 ) ;
#40686 = CARTESIAN_POINT ( 'NONE',  ( 3.504965621013899746, 3.565840152826760256, 3.504965621013765631 ) ) ;
#40687 = CARTESIAN_POINT ( 'NONE',  ( 22.92187500061451644, 4.119189519843966529, 2.378215178124999607 ) ) ;
#40688 = CARTESIAN_POINT ( 'NONE',  ( 1.071796769724490561, 13.25134618820330168, 34.00000000000000000 ) ) ;
#40689 = CARTESIAN_POINT ( 'NONE',  ( 25.52812500061451573, 6.421520780324663323E-16, -5.243569643749999010 ) ) ;
#40690 = CARTESIAN_POINT ( 'NONE',  ( 17.25000000122903288, -2.886751345948092684, -5.000000000000057732 ) ) ;
#40691 = CARTESIAN_POINT ( 'NONE',  ( 27.98437500061451289, 4.541064518000418104, 2.621784821874999949 ) ) ;
#40692 = CARTESIAN_POINT ( 'NONE',  ( 24.22500000000000142, -4.330127018922194537, 2.499999999999995559 ) ) ;
#40693 = CARTESIAN_POINT ( 'NONE',  ( 7.228125000614517681, 4.541064518000418104, 2.621784821874999949 ) ) ;
#40694 = CARTESIAN_POINT ( 'NONE',  ( 24.90937500061451004, -5.492252693125287522, -1.008910452111647106E-15 ) ) ;
#40695 =( BOUNDED_CURVE ( )  B_SPLINE_CURVE ( 2, ( #63269, #58075, #69551, #41827, #6404, #28936, #51472 ),
 .UNSPECIFIED., .F., .F. ) 
 B_SPLINE_CURVE_WITH_KNOTS ( ( 3, 2, 2, 3 ),
 ( 0.4500000000000001221, 0.4527777777777778345, 0.4555555555555555469, 0.4583333333333332593 ),
 .UNSPECIFIED. ) 
 CURVE ( )  GEOMETRIC_REPRESENTATION_ITEM ( )  RATIONAL_B_SPLINE_CURVE ( ( 0.9999999999999946709, 0.8660254037844440367, 1.000000000000000000, 0.8660254037844387076, 1.000000000000000000, 0.8660254037844413721, 0.9999999999999973355 ) ) 
 REPRESENTATION_ITEM ( '' )  );
#40696 = CARTESIAN_POINT ( 'NONE',  ( 18.68437500061451928, -4.541064518000419881, 2.621784821874995952 ) ) ;
#40697 = CARTESIAN_POINT ( 'NONE',  ( 11.70937500061451608, 2.746126346562643317, 4.756430356249998326 ) ) ;
#40698 = CARTESIAN_POINT ( 'NONE',  ( 28.68750000122903288, 4.330127018922191873, 2.499999999999999556 ) ) ;
#40699 = CARTESIAN_POINT ( 'NONE',  ( 8.596875000614518925, 6.054752690667223547, 3.707466751127219781E-16 ) ) ;
#40700 = VERTEX_POINT ( 'NONE', #3614 ) ;
#40701 = CARTESIAN_POINT ( 'NONE',  ( 18.98437500061451644, 4.541064518000418104, 2.621784821874999949 ) ) ;
#40702 = CARTESIAN_POINT ( 'NONE',  ( 13.76250000122903394, 4.330127018922192761, -2.499999999999997780 ) ) ;
#40703 = CARTESIAN_POINT ( 'NONE',  ( 25.53750000000000142, -2.886751345948129988, 4.999999999999997335 ) ) ;
#40704 = CARTESIAN_POINT ( 'NONE',  ( 3.374999999999999556, 4.330127018922191873, 2.499999999999999556 ) ) ;
#40705 = CARTESIAN_POINT ( 'NONE',  ( 29.69999999999999574, -4.330127018922190985, -2.500000000000001332 ) ) ;
#40706 = CARTESIAN_POINT ( 'NONE',  ( 15.90000000000000036, 4.330127018922192761, -2.499999999999997780 ) ) ;
#40707 = VERTEX_POINT ( 'NONE', #59005 ) ;
#40708 = CARTESIAN_POINT ( 'NONE',  ( 9.674999999999998934, 4.330127018922191873, 2.499999999999999556 ) ) ;
#40709 = CARTESIAN_POINT ( 'NONE',  ( 12.90937500061451537, 2.746126346562645981, -4.756430356249997438 ) ) ;
#40710 = CARTESIAN_POINT ( 'NONE',  ( 25.56562500061452070, 3.027376345333613106, -5.243569643749998122 ) ) ;
#40711 = CARTESIAN_POINT ( 'NONE',  ( 13.16249999999999964, 2.886751345948129099, -4.999999999999998224 ) ) ;
#40712 = EDGE_CURVE ( 'NONE', #68026, #17299, #20788, .T. ) ;
#40713 = CARTESIAN_POINT ( 'NONE',  ( 9.675000001229035362, 2.886751345948129099, -4.999999999999998224 ) ) ;
#40714 = CARTESIAN_POINT ( 'NONE',  ( 8.540625000614518569, 6.054752690667223547, 3.707466751127219781E-16 ) ) ;
#40715 = CARTESIAN_POINT ( 'NONE',  ( 21.30000000000000071, 4.330127018922192761, -2.499999999999997780 ) ) ;
#40716 = CARTESIAN_POINT ( 'NONE',  ( 20.20312500061451644, 4.541064518000418104, -2.621784821874998173 ) ) ;
#40717 = CARTESIAN_POINT ( 'NONE',  ( 30.00000000000000000, 0.000000000000000000, 0.000000000000000000 ) ) ;
#40718 = CARTESIAN_POINT ( 'NONE',  ( 26.32500000122903216, 2.886751345948129099, -4.999999999999998224 ) ) ;
#40719 = CARTESIAN_POINT ( 'NONE',  ( -1.878215178125001827, 16.09062499938548285, 33.25316411605952283 ) ) ;
#40720 = CARTESIAN_POINT ( 'NONE',  ( 6.825000000000001066, 6.123233995736764310E-16, -4.999999999999998224 ) ) ;
#40721 = AXIS2_PLACEMENT_3D ( 'NONE', #68631, #18718, #46823 ) ;
#40722 = VERTEX_POINT ( 'NONE', #13949 ) ;
#40723 = CARTESIAN_POINT ( 'NONE',  ( 22.19062500061451715, -3.027376345333614438, 5.243569643749998122 ) ) ;
#40724 = DIRECTION ( 'NONE',  ( 1.000000000000000000, 0.000000000000000000, 0.000000000000000000 ) ) ;
#40725 = CARTESIAN_POINT ( 'NONE',  ( 28.20937500061451786, -4.541064518000417216, -2.621784821875001281 ) ) ;
#40726 = CARTESIAN_POINT ( 'NONE',  ( 19.69687500061451857, -3.027376345333610441, -5.243569643749999898 ) ) ;
#40727 = CARTESIAN_POINT ( 'NONE',  ( 15.44062500061451537, -3.027376345333614438, 5.243569643749998122 ) ) ;
#40728 = CARTESIAN_POINT ( 'NONE',  ( 12.16875000122903394, -5.773502691896255534, -1.060575238724906372E-15 ) ) ;
#40729 = VECTOR ( 'NONE', #34156, 1000.000000000000000 ) ;
#40730 = CARTESIAN_POINT ( 'NONE',  ( 26.43750000122903288, 4.330127018922191873, 2.499999999999999556 ) ) ;
#40731 = CARTESIAN_POINT ( 'NONE',  ( 21.94687500061451502, -2.746126346562641984, -4.756430356249999214 ) ) ;
#40732 = CARTESIAN_POINT ( 'NONE',  ( 16.30312500061451786, 0.000000000000000000, 5.243569643749999010 ) ) ;
#40733 = DIRECTION ( 'NONE',  ( 0.000000000000000000, 0.000000000000000000, 1.000000000000000000 ) ) ;
#40734 = DIRECTION ( 'NONE',  ( -0.000000000000000000, -1.000000000000000000, -0.000000000000000000 ) ) ;
#40735 = CARTESIAN_POINT ( 'NONE',  ( 11.67187500061451821, 3.027376345333613106, -5.243569643749998122 ) ) ;
#40736 = CARTESIAN_POINT ( 'NONE',  ( 12.90937500061451537, -4.541064518000417216, -2.621784821875001281 ) ) ;
#40737 = CARTESIAN_POINT ( 'NONE',  ( 19.13437500061451857, -4.541064518000419881, 2.621784821874995952 ) ) ;
#40738 = ORIENTED_EDGE ( 'NONE', *, *, #66190, .F. ) ;
#40739 = CARTESIAN_POINT ( 'NONE',  ( 25.26562500061451289, 3.027376345333611329, 5.243569643749999010 ) ) ;
#40740 = VECTOR ( 'NONE', #22780, 1000.000000000000000 ) ;
#40741 = CARTESIAN_POINT ( 'NONE',  ( 19.43437500061451928, 4.541064518000418104, 2.621784821874999949 ) ) ;
#40742 = CARTESIAN_POINT ( 'NONE',  ( 24.55312500061451786, -4.541064518000417216, -2.621784821875001281 ) ) ;
#40743 = CARTESIAN_POINT ( 'NONE',  ( 27.07499999999999929, 6.123233995736764310E-16, -4.999999999999998224 ) ) ;
#40744 = CARTESIAN_POINT ( 'NONE',  ( -2.000000000000000000, 13.62500000000000178, 26.53589838486224650 ) ) ;
#40745 = CARTESIAN_POINT ( 'NONE',  ( 28.22812500061451502, 6.421520780324663323E-16, -5.243569643749999010 ) ) ;
#40746 = CARTESIAN_POINT ( 'NONE',  ( 10.57500000122903572, 2.886751345948129099, -4.999999999999998224 ) ) ;
#40747 = VECTOR ( 'NONE', #42688, 1000.000000000000000 ) ;
#40748 = CARTESIAN_POINT ( 'NONE',  ( 5.587500001229033231, 6.123233995736764310E-16, -4.999999999999998224 ) ) ;
#40749 = CARTESIAN_POINT ( 'NONE',  ( 21.26249999999999574, 2.886751345948129099, -4.999999999999997335 ) ) ;
#40750 = CARTESIAN_POINT ( 'NONE',  ( 27.00000000122903288, -2.886751345948129988, 4.999999999999997335 ) ) ;
#40751 = CARTESIAN_POINT ( 'NONE',  ( 1.878215178124997609, 13.57812499938548356, 33.25316411605952993 ) ) ;
#40752 = CARTESIAN_POINT ( 'NONE',  ( 17.04375000122903216, -2.886751345948129988, 4.999999999999997335 ) ) ;
#40753 = CARTESIAN_POINT ( 'NONE',  ( 8.334375000614516082, -4.541064518000419881, 2.621784821874995952 ) ) ;
#40754 = CARTESIAN_POINT ( 'NONE',  ( 1.071796769724489895, 10.07990381179669903, 26.00000000000000355 ) ) ;
#40755 = CARTESIAN_POINT ( 'NONE',  ( 16.97812500061451502, 6.421520780324663323E-16, -5.243569643749999010 ) ) ;
#40756 = CARTESIAN_POINT ( 'NONE',  ( 9.909375000614517148, 4.541064518000418104, -2.621784821874998173 ) ) ;
#40757 = CARTESIAN_POINT ( 'NONE',  ( 28.23750000122903359, 4.330127018922191873, 2.499999999999999556 ) ) ;
#40758 = CARTESIAN_POINT ( 'NONE',  ( 19.13437500061451857, -4.541064518000419881, 2.621784821874995952 ) ) ;
#40759 = CARTESIAN_POINT ( 'NONE',  ( 7.996875000614519280, -3.027376345333610441, -5.243569643749999898 ) ) ;
#40760 = CARTESIAN_POINT ( 'NONE',  ( 3.215625000614518836, 3.027376345333611329, 5.243569643749999010 ) ) ;
#40761 = CARTESIAN_POINT ( 'NONE',  ( 10.80000000000000071, -4.330127018922190985, -2.500000000000001332 ) ) ;
#40762 = CARTESIAN_POINT ( 'NONE',  ( 7.603125000614517681, 4.541064518000418104, -2.621784821874998173 ) ) ;
#40763 = CARTESIAN_POINT ( 'NONE',  ( 17.61562500061451786, 3.027376345333611329, 5.243569643749999010 ) ) ;
#40764 = EDGE_CURVE ( 'NONE', #33074, #17652, #30939, .T. ) ;
#40765 = ORIENTED_EDGE ( 'NONE', *, *, #53394, .F. ) ;
#40766 = CARTESIAN_POINT ( 'NONE',  ( 6.112500001229034474, 4.330127018922192761, -2.499999999999997780 ) ) ;
#40767 = CARTESIAN_POINT ( 'NONE',  ( 15.02812500061451750, -4.541064518000419881, 2.621784821874995952 ) ) ;
#40768 = CARTESIAN_POINT ( 'NONE',  ( 12.21562500061451573, 3.027376345333611329, 5.243569643749999010 ) ) ;
#40769 = CARTESIAN_POINT ( 'NONE',  ( 22.92187500061451644, 2.746126346562645981, -4.756430356249997438 ) ) ;
#40770 = CARTESIAN_POINT ( 'NONE',  ( 12.78749999999999964, 5.773502691896255534, 3.535250795749688894E-16 ) ) ;
#40771 = CARTESIAN_POINT ( 'NONE',  ( 6.637500001229035718, 4.330127018922191873, 2.499999999999999556 ) ) ;
#40772 = CARTESIAN_POINT ( 'NONE',  ( 3.628125000614518036, 4.541064518000418104, 2.621784821874999949 ) ) ;
#40773 = CARTESIAN_POINT ( 'NONE',  ( 19.16250000122903430, 4.330127018922192761, -2.499999999999997780 ) ) ;
#40774 = CARTESIAN_POINT ( 'NONE',  ( 24.89999999999999858, 4.330127018922192761, -2.499999999999997780 ) ) ;
#40775 = B_SPLINE_CURVE_WITH_KNOTS ( 'NONE', 1,
 ( #21267, #5385 ),
 .UNSPECIFIED., .F., .F.,
 ( 2, 2 ),
 ( 0.000000000000000000, 1.000000000000000000 ),
 .UNSPECIFIED. ) ;
#40776 = CARTESIAN_POINT ( 'NONE',  ( 2.121784821875001281, 12.35937500061451821, -26.32496088578401938 ) ) ;
#40777 = LINE ( 'NONE', #40408, #34751 ) ;
#40778 = CARTESIAN_POINT ( 'NONE',  ( 12.88125000122903430, 4.330127018922191873, 2.499999999999999556 ) ) ;
#40779 = CARTESIAN_POINT ( 'NONE',  ( 2.962500001229034119, 4.330127018922192761, -2.499999999999997780 ) ) ;
#40780 = CARTESIAN_POINT ( 'NONE',  ( 24.60000000000000142, 0.000000000000000000, 4.999999999999998224 ) ) ;
#40781 = CARTESIAN_POINT ( 'NONE',  ( 19.17187500061451999, -6.054752690667223547, -1.112240025338166033E-15 ) ) ;
#40782 = DIRECTION ( 'NONE',  ( -0.000000000000000000, -1.000000000000000000, -0.000000000000000000 ) ) ;
#40783 = AXIS2_PLACEMENT_3D ( 'NONE', #18312, #56413, #39428 ) ;
#40784 = CARTESIAN_POINT ( 'NONE',  ( 14.54062500061451679, -3.027376345333614438, 5.243569643749998122 ) ) ;
#40785 = CARTESIAN_POINT ( 'NONE',  ( 10.18125000122903323, 4.330127018922191873, 2.499999999999999556 ) ) ;
#40786 = CARTESIAN_POINT ( 'NONE',  ( 0.000000000000000000, 20.00000000000000000, -33.99999999999999289 ) ) ;
#40787 = CARTESIAN_POINT ( 'NONE',  ( 25.77187500061451075, 3.027376345333611329, 5.243569643749999010 ) ) ;
#40788 = CARTESIAN_POINT ( 'NONE',  ( 18.19687500061451502, -4.119189519843965641, -2.378215178125001383 ) ) ;
#40789 = CARTESIAN_POINT ( 'NONE',  ( 11.91562500061451857, -6.054752690667223547, -1.112240025338166033E-15 ) ) ;
#40790 = AXIS2_PLACEMENT_3D ( 'NONE', #32980, #28177, #4914 ) ;
#40791 = CARTESIAN_POINT ( 'NONE',  ( 15.90937500061451892, 0.000000000000000000, 5.243569643749999010 ) ) ;
#40792 = EDGE_LOOP ( 'NONE', ( #13734, #48752, #39803, #47342 ) ) ;
#40793 = CARTESIAN_POINT ( 'NONE',  ( 28.56562500061451715, -6.054752690667223547, -1.112240025338166033E-15 ) ) ;
#40794 = CARTESIAN_POINT ( 'NONE',  ( 21.10312500061451502, 4.541064518000418104, -2.621784821874998173 ) ) ;
#40795 = CARTESIAN_POINT ( 'NONE',  ( 2.000000000000001332, 13.06250000122903465, -26.53589838486224650 ) ) ;
#40796 = DIRECTION ( 'NONE',  ( 0.000000000000000000, 0.000000000000000000, -1.000000000000000000 ) ) ;
#40797 = CARTESIAN_POINT ( 'NONE',  ( 9.375000000000001776, -4.330127018922194537, 2.499999999999995559 ) ) ;
#40798 = CARTESIAN_POINT ( 'NONE',  ( 20.21250000122903145, 0.000000000000000000, 4.999999999999998224 ) ) ;
#40799 = CARTESIAN_POINT ( 'NONE',  ( -3.999999999999999112, 10.06250000000000178, 27.69059892324149885 ) ) ;
#40800 = CARTESIAN_POINT ( 'NONE',  ( 11.59687500061451537, 4.119189519843966529, -2.378215178124998275 ) ) ;
#40801 = VERTEX_POINT ( 'NONE', #47945 ) ;
#40802 = CARTESIAN_POINT ( 'NONE',  ( 18.78749999999999432, -2.886751345948129988, 4.999999999999997335 ) ) ;
#40803 = CARTESIAN_POINT ( 'NONE',  ( 21.56250000000000000, -5.773502691896255534, -1.060575238724906372E-15 ) ) ;
#40804 = CARTESIAN_POINT ( 'NONE',  ( 19.32187500061451857, 3.027376345333613106, -5.243569643749998122 ) ) ;
#40805 = CARTESIAN_POINT ( 'NONE',  ( 24.17812500061451786, 6.421520780324663323E-16, -5.243569643749999010 ) ) ;
#40806 = EDGE_LOOP ( 'NONE', ( #66995, #34438, #39917, #25454 ) ) ;
#40807 = CARTESIAN_POINT ( 'NONE',  ( 28.01250000122903216, -4.330127018922190985, -2.500000000000001332 ) ) ;
#40808 = CARTESIAN_POINT ( 'NONE',  ( 5.053125000614517859, 0.000000000000000000, 5.243569643749999010 ) ) ;
#40809 = DIRECTION ( 'NONE',  ( -0.000000000000000000, -1.000000000000000000, -0.000000000000000000 ) ) ;
#40810 = CARTESIAN_POINT ( 'NONE',  ( 14.81250000000000000, -5.773502691896255534, -1.060575238724906372E-15 ) ) ;
#40811 = CARTESIAN_POINT ( 'NONE',  ( -4.243569643749999898, 17.10312500061451502, 30.00000000000000000 ) ) ;
#40812 = CARTESIAN_POINT ( 'NONE',  ( 28.22812500061451502, 6.421520780324663323E-16, -5.243569643749999010 ) ) ;
#40813 = CARTESIAN_POINT ( 'NONE',  ( 9.449999999999999289, -4.330127018922190985, -2.500000000000001332 ) ) ;
#40814 = CARTESIAN_POINT ( 'NONE',  ( -3.756430356250001434, 18.30312499938548143, 32.16877607737301048 ) ) ;
#40815 = CARTESIAN_POINT ( 'NONE',  ( 25.95937500061451431, -4.541064518000417216, -2.621784821875001281 ) ) ;
#40816 = VERTEX_POINT ( 'NONE', #13577 ) ;
#40817 = CARTESIAN_POINT ( 'NONE',  ( 21.74062500061451431, -3.027376345333614438, 5.243569643749998122 ) ) ;
#40818 = CARTESIAN_POINT ( 'NONE',  ( 22.54687500061451999, 6.054752690667223547, 3.707466751127219781E-16 ) ) ;
#40819 = CARTESIAN_POINT ( 'NONE',  ( 2.121784821875001281, 15.90312500061459566, -26.32496088578401938 ) ) ;
#40820 = CARTESIAN_POINT ( 'NONE',  ( 10.27499999999999858, -4.330127018922194537, 2.499999999999995559 ) ) ;
#40821 = CARTESIAN_POINT ( 'NONE',  ( 6.740625000614516082, 6.054752690667223547, 3.707466751127219781E-16 ) ) ;
#40822 = CARTESIAN_POINT ( 'NONE',  ( 29.07187500061451502, -5.492252693125287522, -1.008910452111647106E-15 ) ) ;
#40823 = CARTESIAN_POINT ( 'NONE',  ( 22.94062500061451004, 6.054752690667223547, 3.707466751127219781E-16 ) ) ;
#40824 = CARTESIAN_POINT ( 'NONE',  ( 28.58437500061451431, -2.746126346562641984, -4.756430356249999214 ) ) ;
#40825 = CARTESIAN_POINT ( 'NONE',  ( 13.95937500061451786, 4.119189519843966529, -2.378215178124998275 ) ) ;
#40826 = CARTESIAN_POINT ( 'NONE',  ( 17.10937500061451999, 4.541064518000418104, -2.621784821874998173 ) ) ;
#40827 = CARTESIAN_POINT ( 'NONE',  ( 4.243569643749999010, 12.47187500061451715, 27.54997392385601174 ) ) ;
#40828 = CARTESIAN_POINT ( 'NONE',  ( 19.92187500061451644, 3.027376345333611329, 5.243569643749999010 ) ) ;
#40829 = CARTESIAN_POINT ( 'NONE',  ( 27.49687500061451217, 6.054752690667223547, 3.707466751127219781E-16 ) ) ;
#40830 = CARTESIAN_POINT ( 'NONE',  ( 4.243569643749999898, 16.89687500061451786, 32.45002607614398471 ) ) ;
#40831 = CARTESIAN_POINT ( 'NONE',  ( 8.615625000614517859, 3.027376345333611329, 5.243569643749999010 ) ) ;
#40832 = CARTESIAN_POINT ( 'NONE',  ( -5.810221930991193690E-16, 10.55000000122903359, -34.00000000000000000 ) ) ;
#40833 = CARTESIAN_POINT ( 'NONE',  ( 4.321875000614517681, -6.054752690667223547, -1.112240025338166033E-15 ) ) ;
#40834 = CYLINDRICAL_SURFACE ( 'NONE', #43099, 4.999999999999998224 ) ;
#40835 = VECTOR ( 'NONE', #43874, 1000.000000000000000 ) ;
#40836 = CARTESIAN_POINT ( 'NONE',  ( 4.340625000614515727, -3.027376345333610441, -5.243569643749999898 ) ) ;
#40837 = CARTESIAN_POINT ( 'NONE',  ( 8.709375000614517859, 0.000000000000000000, 5.243569643749999010 ) ) ;
#40838 = CARTESIAN_POINT ( 'NONE',  ( 16.72500000122903430, -5.773502691896255534, -1.060575238724906372E-15 ) ) ;
#40839 = CARTESIAN_POINT ( 'NONE',  ( 5.071875000614519458, 3.027376345333611329, 5.243569643749999010 ) ) ;
#40840 = CARTESIAN_POINT ( 'NONE',  ( 7.715625000614515727, 3.027376345333611329, 5.243569643749999010 ) ) ;
#40841 = CARTESIAN_POINT ( 'NONE',  ( -3.999999999999999556, 13.08124999877096606, 27.69059892324149175 ) ) ;
#40842 = CARTESIAN_POINT ( 'NONE',  ( 22.85625000122903216, 0.000000000000000000, 4.999999999999998224 ) ) ;
#40843 = CARTESIAN_POINT ( 'NONE',  ( 16.35937500061451644, 0.000000000000000000, 5.243569643749999010 ) ) ;
#40844 = FACE_OUTER_BOUND ( 'NONE', #66852, .T. ) ;
#40845 = ORIENTED_EDGE ( 'NONE', *, *, #62835, .T. ) ;
#40846 = CARTESIAN_POINT ( 'NONE',  ( 24.47812500061451502, -4.541064518000419881, 2.621784821874995952 ) ) ;
#40847 = CARTESIAN_POINT ( 'NONE',  ( 8.840625000614515727, -3.027376345333610441, -5.243569643749999898 ) ) ;
#40848 = CARTESIAN_POINT ( 'NONE',  ( 27.64687500061452141, -3.027376345333614438, 5.243569643749998122 ) ) ;
#40849 = CARTESIAN_POINT ( 'NONE',  ( 10.00312500061451715, 0.000000000000000000, 5.243569643749999010 ) ) ;
#40850 = CARTESIAN_POINT ( 'NONE',  ( 4.544497808834801589, -2.085075457992688897, -4.544497808831748920 ) ) ;
#40851 =( BOUNDED_CURVE ( )  B_SPLINE_CURVE ( 2, ( #33056, #67419, #49695, #50424, #38975, #39339, #33781 ),
 .UNSPECIFIED., .F., .F. ) 
 B_SPLINE_CURVE_WITH_KNOTS ( ( 3, 2, 2, 3 ),
 ( 0.6900000000000000577, 0.6933333333333334680, 0.6966666666666668783, 0.7000000000000001776 ),
 .UNSPECIFIED. ) 
 CURVE ( )  GEOMETRIC_REPRESENTATION_ITEM ( )  RATIONAL_B_SPLINE_CURVE ( ( 0.9999999999999955591, 0.8660254037844431485, 1.000000000000000000, 0.8660254037844387076, 1.000000000000000000, 0.8660254037844298258, 1.000000000000008882 ) ) 
 REPRESENTATION_ITEM ( '' )  );
#40852 = CARTESIAN_POINT ( 'NONE',  ( 10.05000000122903181, -2.886751345948125991, -5.000000000000000000 ) ) ;
#40853 = CARTESIAN_POINT ( 'NONE',  ( 23.87812500061451715, 4.541064518000418104, 2.621784821874999949 ) ) ;
#40854 = ADVANCED_FACE ( 'NONE', ( #58275 ), #2507, .F. ) ;
#40855 = CARTESIAN_POINT ( 'NONE',  ( 2.121784821875001281, 13.65312500061451750, -26.32496088578401938 ) ) ;
#40856 = CARTESIAN_POINT ( 'NONE',  ( 12.52500000122903145, 2.886751345948126879, 4.999999999999999112 ) ) ;
#40857 = CARTESIAN_POINT ( 'NONE',  ( 22.97812500061451857, 4.541064518000418104, 2.621784821874999949 ) ) ;
#40858 = CARTESIAN_POINT ( 'NONE',  ( 11.17500000000000071, -4.330127018922194537, 2.499999999999995559 ) ) ;
#40859 = CARTESIAN_POINT ( 'NONE',  ( 19.34062500061451573, 6.054752690667223547, 3.707466751127219781E-16 ) ) ;
#40860 = CARTESIAN_POINT ( 'NONE',  ( 5.371875000614516615, 3.027376345333612662, -5.243569643749998122 ) ) ;
#40861 = CARTESIAN_POINT ( 'NONE',  ( 20.43749999999999645, 5.773502691896255534, 3.535250795749688894E-16 ) ) ;
#40862 = CARTESIAN_POINT ( 'NONE',  ( 15.37500000122903465, -5.773502691896255534, -1.060575238724906372E-15 ) ) ;
#40863 = CARTESIAN_POINT ( 'NONE',  ( 11.69062500061451360, 6.054752690667223547, 3.707466751127219781E-16 ) ) ;
#40864 = CARTESIAN_POINT ( 'NONE',  ( 16.37812500061451715, -4.541064518000419881, 2.621784821874995952 ) ) ;
#40865 = CARTESIAN_POINT ( 'NONE',  ( 25.98750000122903003, 4.330127018922191873, 2.499999999999999556 ) ) ;
#40866 = CARTESIAN_POINT ( 'NONE',  ( 19.38749999999999929, -2.886751345948125991, -5.000000000000000000 ) ) ;
#40867 = CARTESIAN_POINT ( 'NONE',  ( 22.73437500061451644, -4.541064518000419881, 2.621784821874995952 ) ) ;
#40868 = CARTESIAN_POINT ( 'NONE',  ( 14.69999999999999929, 0.000000000000000000, 4.999999999999998224 ) ) ;
#40869 = CARTESIAN_POINT ( 'NONE',  ( 11.28750000122903252, -4.330127018922194537, 2.499999999999995559 ) ) ;
#40870 = CARTESIAN_POINT ( 'NONE',  ( 9.234375000614518214, -4.541064518000419881, 2.621784821874995952 ) ) ;
#40871 = CARTESIAN_POINT ( 'NONE',  ( 25.32187500061451857, 3.027376345333611329, 5.243569643749999010 ) ) ;
#40872 = CARTESIAN_POINT ( 'NONE',  ( 15.48750000122903359, 6.123233995736764310E-16, -4.999999999999998224 ) ) ;
#40873 = CARTESIAN_POINT ( 'NONE',  ( 20.84062500061451573, -3.027376345333614438, 5.243569643749998122 ) ) ;
#40874 = CARTESIAN_POINT ( 'NONE',  ( 27.60937500061451644, 0.000000000000000000, 5.243569643749999010 ) ) ;
#40875 = CARTESIAN_POINT ( 'NONE',  ( -7.967954043666661671E-16, 16.24062499938548143, 34.33755215474603517 ) ) ;
#40876 = DIRECTION ( 'NONE',  ( 1.000000000000000000, 0.000000000000000000, 0.000000000000000000 ) ) ;
#40877 = VECTOR ( 'NONE', #45055, 1000.000000000000000 ) ;
#40878 = CARTESIAN_POINT ( 'NONE',  ( 7.621875000614519280, 3.027376345333613106, -5.243569643749998122 ) ) ;
#40879 = CARTESIAN_POINT ( 'NONE',  ( 19.37812500061451715, 4.541064518000418104, 2.621784821874999949 ) ) ;
#40880 = ORIENTED_EDGE ( 'NONE', *, *, #64083, .T. ) ;
#40881 = CARTESIAN_POINT ( 'NONE',  ( 27.17812500061451786, -4.541064518000419881, 2.621784821874995952 ) ) ;
#40882 = CARTESIAN_POINT ( 'NONE',  ( 3.234375000614516438, 4.541064518000418104, 2.621784821874999949 ) ) ;
#40883 = LINE ( 'NONE', #63030, #40740 ) ;
#40884 = DIRECTION ( 'NONE',  ( 0.000000000000000000, 0.000000000000000000, -1.000000000000000000 ) ) ;
#40885 = CARTESIAN_POINT ( 'NONE',  ( 16.23750000000000071, -2.886751345948125991, -5.000000000000000000 ) ) ;
#40886 = CARTESIAN_POINT ( 'NONE',  ( 21.55312500061451431, 4.541064518000418104, -2.621784821874998173 ) ) ;
#40887 = VERTEX_POINT ( 'NONE', #2155 ) ;
#40888 = CARTESIAN_POINT ( 'NONE',  ( 25.83749999999999858, 5.773502691896255534, 3.535250795749688894E-16 ) ) ;
#40889 =( BOUNDED_CURVE ( )  B_SPLINE_CURVE ( 2, ( #35249, #34521, #13070, #7180, #18964, #41524, #35972 ),
 .UNSPECIFIED., .F., .F. ) 
 B_SPLINE_CURVE_WITH_KNOTS ( ( 3, 2, 2, 3 ),
 ( 0.9100000000000000311, 0.9133333333333333304, 0.9166666666666667407, 0.9200000000000001510 ),
 .UNSPECIFIED. ) 
 CURVE ( )  GEOMETRIC_REPRESENTATION_ITEM ( )  RATIONAL_B_SPLINE_CURVE ( ( 1.000000000000000000, 0.8660254037844387076, 1.000000000000000000, 0.8660254037844387076, 1.000000000000000000, 0.8660254037844342667, 1.000000000000004441 ) ) 
 REPRESENTATION_ITEM ( '' )  );
#40890 = CARTESIAN_POINT ( 'NONE',  ( 26.97187500061451360, 3.027376345333613106, -5.243569643749998122 ) ) ;
#40891 = EDGE_CURVE ( 'NONE', #9764, #72010, #40663, .T. ) ;
#40892 = ORIENTED_EDGE ( 'NONE', *, *, #56668, .T. ) ;
#40893 = CARTESIAN_POINT ( 'NONE',  ( 15.32812500061451644, 4.541064518000418104, 2.621784821874999949 ) ) ;
#40894 = CARTESIAN_POINT ( 'NONE',  ( 6.740625000614516082, 6.054752690667223547, 3.707466751127219781E-16 ) ) ;
#40895 = CARTESIAN_POINT ( 'NONE',  ( 18.57187500061451857, -4.119189519843968306, 2.378215178124996054 ) ) ;
#40896 = CARTESIAN_POINT ( 'NONE',  ( 29.54062500061451502, -3.027376345333610441, -5.243569643749999898 ) ) ;
#40897 = ADVANCED_FACE ( 'NONE', ( #70103 ), #37217, .T. ) ;
#40898 = CARTESIAN_POINT ( 'NONE',  ( 14.25000000122903465, 5.773502691896255534, 3.535250795749688894E-16 ) ) ;
#40899 = CARTESIAN_POINT ( 'NONE',  ( 21.15000000000000213, -4.330127018922190985, -2.500000000000001332 ) ) ;
#40900 = CARTESIAN_POINT ( 'NONE',  ( 28.42499999999999716, 6.123233995736764310E-16, -4.999999999999998224 ) ) ;
#40901 = CARTESIAN_POINT ( 'NONE',  ( 5.184375000614516615, -4.541064518000419881, 2.621784821874995952 ) ) ;
#40902 = CARTESIAN_POINT ( 'NONE',  ( 8.859375000614518214, -4.541064518000417216, -2.621784821875001281 ) ) ;
#40903 = CARTESIAN_POINT ( 'NONE',  ( 20.29687500061451644, 6.054752690667223547, 3.707466751127219781E-16 ) ) ;
#40904 = CARTESIAN_POINT ( 'NONE',  ( 30.00000000000000000, 0.000000000000000000, 0.000000000000000000 ) ) ;
#40905 = ORIENTED_EDGE ( 'NONE', *, *, #29319, .F. ) ;
#40906 = CARTESIAN_POINT ( 'NONE',  ( 27.92812500061451431, 4.541064518000418104, 2.621784821874999949 ) ) ;
#40907 = CARTESIAN_POINT ( 'NONE',  ( 3.187500000000002220, -2.886751345948125991, -5.000000000000000000 ) ) ;
#40908 = CARTESIAN_POINT ( 'NONE',  ( 4.846875000614519813, -3.027376345333610441, -5.243569643749999898 ) ) ;
#40909 = CARTESIAN_POINT ( 'NONE',  ( 18.18750000000000000, 5.773502691896255534, 3.535250795749688894E-16 ) ) ;
#40910 = CARTESIAN_POINT ( 'NONE',  ( 14.01562500061451644, 3.027376345333611329, 5.243569643749999010 ) ) ;
#40911 = CARTESIAN_POINT ( 'NONE',  ( 2.929172373741449675, 20.54242198200764946, 33.54521906142198162 ) ) ;
#40912 = CARTESIAN_POINT ( 'NONE',  ( 5.700000000000000178, 0.000000000000000000, 4.999999999999998224 ) ) ;
#40913 = CARTESIAN_POINT ( 'NONE',  ( 11.26875000122903181, -5.773502691896255534, -1.060575238724906372E-15 ) ) ;
#40914 = CARTESIAN_POINT ( 'NONE',  ( 20.89687500061452141, -2.746126346562646425, 4.756430356249996549 ) ) ;
#40915 = CARTESIAN_POINT ( 'NONE',  ( 8.840625000614515727, -3.027376345333610441, -5.243569643749999898 ) ) ;
#40916 = CARTESIAN_POINT ( 'NONE',  ( 26.14687500061451431, 6.054752690667223547, 3.707466751127219781E-16 ) ) ;
#40917 = EDGE_CURVE ( 'NONE', #32704, #100, #66688, .T. ) ;
#40918 = CARTESIAN_POINT ( 'NONE',  ( -2.121784821874999949, 18.43437500061451928, 26.32496088578401938 ) ) ;
#40919 = CARTESIAN_POINT ( 'NONE',  ( 27.12187500061451573, 3.027376345333611329, 5.243569643749999010 ) ) ;
#40920 = CARTESIAN_POINT ( 'NONE',  ( 6.712500000000000355, -5.773502691896255534, -1.060575238724906372E-15 ) ) ;
#40921 = CARTESIAN_POINT ( 'NONE',  ( 8.484601909799253346E-16, 13.47500000122903430, 34.61880215351700230 ) ) ;
#40922 = CARTESIAN_POINT ( 'NONE',  ( 15.89062500061451289, -3.027376345333614438, 5.243569643749998122 ) ) ;
#40923 = CARTESIAN_POINT ( 'NONE',  ( 6.187500001229032875, 4.330127018922191873, 2.499999999999999556 ) ) ;
#40924 = CARTESIAN_POINT ( 'NONE',  ( 18.64687500061451786, -3.027376345333614438, 5.243569643749998122 ) ) ;
#40925 = CARTESIAN_POINT ( 'NONE',  ( 12.79687500061451821, -3.027376345333614438, 5.243569643749998122 ) ) ;
#40926 = CARTESIAN_POINT ( 'NONE',  ( -3.858979783667864538, 3.180598473748192490, -28.91336298736815635 ) ) ;
#40927 = ORIENTED_EDGE ( 'NONE', *, *, #11525, .T. ) ;
#40928 = CARTESIAN_POINT ( 'NONE',  ( 13.34062500061451750, -3.027376345333610441, -5.243569643749999898 ) ) ;
#40929 = CARTESIAN_POINT ( 'NONE',  ( 24.97500000122903430, 2.886751345948129099, -4.999999999999998224 ) ) ;
#40930 = CARTESIAN_POINT ( 'NONE',  ( 12.98437500061451821, 6.421520780324663323E-16, -5.243569643749999010 ) ) ;
#40931 = CARTESIAN_POINT ( 'NONE',  ( 15.85312500061451857, 0.000000000000000000, 5.243569643749999010 ) ) ;
#40932 = EDGE_CURVE ( 'NONE', #66981, #27675, #28356, .T. ) ;
#40933 = CARTESIAN_POINT ( 'NONE',  ( 4.400918202330496243, -2.373166445152071535, -4.675799785326651303 ) ) ;
#40934 = CARTESIAN_POINT ( 'NONE',  ( 23.44687500061451502, 6.054752690667223547, 3.707466751127219781E-16 ) ) ;
#40935 = DIRECTION ( 'NONE',  ( -1.000000000000000000, -0.000000000000000000, -0.000000000000000000 ) ) ;
#40936 = CARTESIAN_POINT ( 'NONE',  ( 12.93750000122903465, 4.330127018922191873, 2.499999999999999556 ) ) ;
#40937 = DIRECTION ( 'NONE',  ( -1.000000000000000000, -0.000000000000000000, -0.000000000000000000 ) ) ;
#40938 = CARTESIAN_POINT ( 'NONE',  ( 3.103125000614517237, 4.541064518000418104, -2.621784821874998173 ) ) ;
#40939 = CARTESIAN_POINT ( 'NONE',  ( 2.121784821874999061, 17.45937500061451786, -33.67503911421598417 ) ) ;
#40940 = CARTESIAN_POINT ( 'NONE',  ( 18.98437500061451644, 4.541064518000418104, 2.621784821874999949 ) ) ;
#40941 = CARTESIAN_POINT ( 'NONE',  ( 16.50000000122903288, 5.773502691896255534, 3.535250795749688894E-16 ) ) ;
#40942 = CARTESIAN_POINT ( 'NONE',  ( 15.45937500061451608, 0.000000000000000000, 5.243569643749999010 ) ) ;
#40943 = CARTESIAN_POINT ( 'NONE',  ( 45.00000000000000000, 0.000000000000000000, 0.000000000000000000 ) ) ;
#40944 = CARTESIAN_POINT ( 'NONE',  ( 21.03750000122903074, 4.330127018922191873, 2.499999999999999556 ) ) ;
#40945 = CARTESIAN_POINT ( 'NONE',  ( 14.72812500061451679, 6.421520780324663323E-16, -5.243569643749999010 ) ) ;
#40946 = EDGE_LOOP ( 'NONE', ( #65492, #34893, #10986, #70681 ) ) ;
#40947 = ORIENTED_EDGE ( 'NONE', *, *, #37794, .T. ) ;
#40948 = CARTESIAN_POINT ( 'NONE',  ( 18.14999999999999858, 4.330127018922192761, -2.499999999999997780 ) ) ;
#40949 = CARTESIAN_POINT ( 'NONE',  ( 1.351293209486982505, 4.820886669536883495, 26.22567693883006967 ) ) ;
#40950 = CARTESIAN_POINT ( 'NONE',  ( 15.22500000122903252, 2.886751345948126879, 4.999999999999999112 ) ) ;
#40951 = CARTESIAN_POINT ( 'NONE',  ( 26.52187500061451431, 3.027376345333613106, -5.243569643749998122 ) ) ;
#40952 = CARTESIAN_POINT ( 'NONE',  ( 20.01562500061451644, -6.054752690667223547, -1.112240025338166033E-15 ) ) ;
#40953 = CARTESIAN_POINT ( 'NONE',  ( 22.94062500061451715, 6.054752690667223547, 3.707466751127219781E-16 ) ) ;
#40954 = CARTESIAN_POINT ( 'NONE',  ( 4.003125000614518925, 4.541064518000418104, -2.621784821874998173 ) ) ;
#40955 = CARTESIAN_POINT ( 'NONE',  ( 27.93750000000000000, -2.886751345948125991, -5.000000000000000000 ) ) ;
#40956 = CARTESIAN_POINT ( 'NONE',  ( 0.000000000000000000, 20.00000000000000000, -33.99999999999999289 ) ) ;
#40957 = CARTESIAN_POINT ( 'NONE',  ( 10.20937500061451786, -4.119189519843965641, -2.378215178125001383 ) ) ;
#40958 = CARTESIAN_POINT ( 'NONE',  ( -0.7368881354385758975, 9.803648613939515144, -34.17910028561248481 ) ) ;
#40959 = CARTESIAN_POINT ( 'NONE',  ( 20.34375000122903643, -2.886751345948098013, -5.000000000000047073 ) ) ;
#40960 = CARTESIAN_POINT ( 'NONE',  ( -4.243569643749999898, 17.15937500061451715, -30.00000000000000000 ) ) ;
#40961 = CARTESIAN_POINT ( 'NONE',  ( 4.987500001229032698, -4.330127018922194537, 2.499999999999995559 ) ) ;
#40962 = CARTESIAN_POINT ( 'NONE',  ( 6.562500000000001776, 2.886751345948126879, 4.999999999999999112 ) ) ;
#40963 = CARTESIAN_POINT ( 'NONE',  ( 16.27499999999999858, 6.123233995736764310E-16, -4.999999999999998224 ) ) ;
#40964 = CARTESIAN_POINT ( 'NONE',  ( 8.709375000614517859, 0.000000000000000000, 5.243569643749999010 ) ) ;
#40965 = CARTESIAN_POINT ( 'NONE',  ( 28.00312500061451715, 0.000000000000000000, 5.243569643749999010 ) ) ;
#40966 = CARTESIAN_POINT ( 'NONE',  ( 27.52500000122903145, -5.773502691896255534, -1.060575238724906372E-15 ) ) ;
#40967 = DIRECTION ( 'NONE',  ( -1.000000000000000000, -0.000000000000000000, -0.000000000000000000 ) ) ;
#40968 = CARTESIAN_POINT ( 'NONE',  ( 3.999999999999999112, 19.43750000122903288, 30.00000000000000000 ) ) ;
#40969 = CARTESIAN_POINT ( 'NONE',  ( 7.921875000614517326, -6.054752690667223547, -1.112240025338166033E-15 ) ) ;
#40970 = CARTESIAN_POINT ( 'NONE',  ( 11.85937500061451644, 0.000000000000000000, 5.243569643749999010 ) ) ;
#40971 = CARTESIAN_POINT ( 'NONE',  ( 5.400000000000002132, -4.330127018922190985, -2.500000000000001332 ) ) ;
#40972 = CARTESIAN_POINT ( 'NONE',  ( -4.243569643749998122, 15.34062500061459744, 32.45002607614398471 ) ) ;
#40973 = CARTESIAN_POINT ( 'NONE',  ( 4.912500000000000533, -5.773502691896255534, -1.060575238724906372E-15 ) ) ;
#40974 = CARTESIAN_POINT ( 'NONE',  ( 6.375000000000001776, 6.123233995736764310E-16, -4.999999999999998224 ) ) ;
#40975 = CARTESIAN_POINT ( 'NONE',  ( 26.81250000122903288, 4.330127018922192761, -2.499999999999997780 ) ) ;
#40976 = CARTESIAN_POINT ( 'NONE',  ( 18.60937500061451289, -5.492252693125287522, -1.008910452111647106E-15 ) ) ;
#40977 = CARTESIAN_POINT ( 'NONE',  ( 22.67812500061451431, -4.541064518000419881, 2.621784821874995952 ) ) ;
#40978 = CARTESIAN_POINT ( 'NONE',  ( 13.11562500061451786, 3.027376345333611329, 5.243569643749999010 ) ) ;
#40979 = CARTESIAN_POINT ( 'NONE',  ( 25.84687500061451360, -4.119189519843965641, -2.378215178125001383 ) ) ;
#40980 = CARTESIAN_POINT ( 'NONE',  ( 8.896875000614517859, -3.027376345333610441, -5.243569643749999898 ) ) ;
#40981 = CARTESIAN_POINT ( 'NONE',  ( 27.33750000000000213, -2.886751345948129988, 4.999999999999997335 ) ) ;
#40982 = CARTESIAN_POINT ( 'NONE',  ( 21.56250000122903288, 0.000000000000000000, 4.999999999999998224 ) ) ;
#40983 = CARTESIAN_POINT ( 'NONE',  ( 7.320879633048903241E-15, 18.20000000122903216, -34.00000000000000000 ) ) ;
#40984 = CARTESIAN_POINT ( 'NONE',  ( 11.33437500061451608, 4.541064518000418104, 2.621784821874999949 ) ) ;
#40985 = CARTESIAN_POINT ( 'NONE',  ( 27.04687500061451644, 6.054752690667223547, 3.707466751127219781E-16 ) ) ;
#40986 = CARTESIAN_POINT ( 'NONE',  ( 21.88125000122903074, 4.330127018922191873, 2.499999999999999556 ) ) ;
#40987 = CARTESIAN_POINT ( 'NONE',  ( 1.071796769724491893, 13.49509619066136779, -26.00000000000000355 ) ) ;
#40988 = CARTESIAN_POINT ( 'NONE',  ( 22.58437500061451431, 4.541064518000418104, 2.621784821874999949 ) ) ;
#40989 = CARTESIAN_POINT ( 'NONE',  ( 12.00937500061451857, -4.541064518000417216, -2.621784821875001281 ) ) ;
#40990 = CARTESIAN_POINT ( 'NONE',  ( 2.655984681222220721E-16, 19.16562499938548214, 25.66244784525396483 ) ) ;
#40991 = CARTESIAN_POINT ( 'NONE',  ( 24.82499999999999929, 6.123233995736764310E-16, -4.999999999999998224 ) ) ;
#40992 = CARTESIAN_POINT ( 'NONE',  ( -3.999999999999999556, 13.58750000000000213, 27.69059892324149175 ) ) ;
#40993 = CARTESIAN_POINT ( 'NONE',  ( -4.243569643749999898, 15.77187500061451608, -32.45002607614398471 ) ) ;
#40994 = CARTESIAN_POINT ( 'NONE',  ( 26.55937500061451573, 4.119189519843966529, -2.378215178124998275 ) ) ;
#40995 = CARTESIAN_POINT ( 'NONE',  ( 17.16562500061451502, 3.027376345333611329, 5.243569643749999010 ) ) ;
#40996 = CARTESIAN_POINT ( 'NONE',  ( 7.800000000000001599, 4.330127018922192761, -2.499999999999997780 ) ) ;
#40997 = ADVANCED_FACE ( 'NONE', ( #14673 ), #7682, .F. ) ;
#40998 = CARTESIAN_POINT ( 'NONE',  ( 45.00000000000000000, 6.123233995736764310E-16, -4.999999999999998224 ) ) ;
#40999 = CARTESIAN_POINT ( 'NONE',  ( 15.82499999999999929, 6.123233995736764310E-16, -4.999999999999998224 ) ) ;
#41000 = CARTESIAN_POINT ( 'NONE',  ( 4.000000000000000000, 19.40000000122903856, 32.30940107675849049 ) ) ;
#41001 = CARTESIAN_POINT ( 'NONE',  ( 13.80000000122903181, 5.773502691896255534, 3.535250795749688894E-16 ) ) ;
#41002 = CARTESIAN_POINT ( 'NONE',  ( 25.62187500061451573, 3.027376345333613106, -5.243569643749998122 ) ) ;
#41003 = ORIENTED_EDGE ( 'NONE', *, *, #57235, .F. ) ;
#41004 = CARTESIAN_POINT ( 'NONE',  ( 19.97812500061451502, -4.541064518000419881, 2.621784821874995952 ) ) ;
#41005 = CARTESIAN_POINT ( 'NONE',  ( 19.99687500061451573, -3.027376345333614438, 5.243569643749998122 ) ) ;
#41006 = CARTESIAN_POINT ( 'NONE',  ( 3.000000000000002665, 0.000000000000000000, 4.999999999999998224 ) ) ;
#41007 = CARTESIAN_POINT ( 'NONE',  ( 7.640625000614517326, 6.054752690667223547, 3.707466751127219781E-16 ) ) ;
#41008 = CARTESIAN_POINT ( 'NONE',  ( 21.02812500061451573, 6.421520780324663323E-16, -5.243569643749999010 ) ) ;
#41009 = CARTESIAN_POINT ( 'NONE',  ( 12.15937500061451892, 4.541064518000418104, -2.621784821874998173 ) ) ;
#41010 = CARTESIAN_POINT ( 'NONE',  ( 18.00937500061451502, 4.541064518000418104, -2.621784821874998173 ) ) ;
#41011 = CARTESIAN_POINT ( 'NONE',  ( 4.243569643749999898, 14.14062500061451644, 32.45002607614398471 ) ) ;
#41012 = CARTESIAN_POINT ( 'NONE',  ( 18.48750000122903359, -4.330127018922194537, 2.499999999999995559 ) ) ;
#41013 = CARTESIAN_POINT ( 'NONE',  ( 14.40937500061451715, 4.119189519843966529, -2.378215178124998275 ) ) ;
#41014 = CARTESIAN_POINT ( 'NONE',  ( 8.615625000614517859, 3.027376345333611329, 5.243569643749999010 ) ) ;
#41015 = CARTESIAN_POINT ( 'NONE',  ( 3.796875000614517326, -3.027376345333614438, 5.243569643749998122 ) ) ;
#41016 = CARTESIAN_POINT ( 'NONE',  ( 28.64062500061451289, -3.027376345333610441, -5.243569643749999898 ) ) ;
#41017 = CARTESIAN_POINT ( 'NONE',  ( 24.83437500061451431, 4.541064518000418104, 2.621784821874999949 ) ) ;
#41018 = CARTESIAN_POINT ( 'NONE',  ( 16.56562500061451715, 3.027376345333613106, -5.243569643749998122 ) ) ;
#41019 = CARTESIAN_POINT ( 'NONE',  ( 24.56250000122903288, 4.330127018922192761, -2.499999999999997780 ) ) ;
#41020 = CARTESIAN_POINT ( 'NONE',  ( 24.92812500061451431, -4.541064518000419881, 2.621784821874995952 ) ) ;
#41021 = CARTESIAN_POINT ( 'NONE',  ( 21.34687500061451715, -3.027376345333614438, 5.243569643749998122 ) ) ;
#41022 = CARTESIAN_POINT ( 'NONE',  ( 16.56562500061451715, 3.027376345333613106, -5.243569643749998122 ) ) ;
#41023 = CARTESIAN_POINT ( 'NONE',  ( -2.121784821874999949, 17.98437500061451999, 26.32496088578401938 ) ) ;
#41024 = CARTESIAN_POINT ( 'NONE',  ( 22.45312500061451644, 4.541064518000418104, -2.621784821874998173 ) ) ;
#41025 = CARTESIAN_POINT ( 'NONE',  ( 34.99999999999999289, -2.499999999999999556, 3.499999999999999556 ) ) ;
#41026 = ORIENTED_EDGE ( 'NONE', *, *, #17437, .T. ) ;
#41027 = CARTESIAN_POINT ( 'NONE',  ( 24.86250000000000071, 2.886751345948129099, -4.999999999999998224 ) ) ;
#41028 = CARTESIAN_POINT ( 'NONE',  ( 2.000000000000001332, 12.50000000000000000, -26.53589838486224650 ) ) ;
#41029 = CARTESIAN_POINT ( 'NONE',  ( -7.967954043666661671E-16, 19.39062499938548001, 34.33755215474603517 ) ) ;
#41030 = CARTESIAN_POINT ( 'NONE',  ( 29.61562500061451431, 3.027376345333613106, -5.243569643749998122 ) ) ;
#41031 = CARTESIAN_POINT ( 'NONE',  ( 10.04062500061451502, -3.027376345333614438, 5.243569643749998122 ) ) ;
#41032 = CARTESIAN_POINT ( 'NONE',  ( 22.01250000122903216, 0.000000000000000000, 4.999999999999998224 ) ) ;
#41033 = ADVANCED_FACE ( 'NONE', ( #43131 ), #3477, .T. ) ;
#41034 = CARTESIAN_POINT ( 'NONE',  ( 26.39062500061451644, -3.027376345333610441, -5.243569643749999898 ) ) ;
#41035 = CARTESIAN_POINT ( 'NONE',  ( 25.31250000000000000, 2.886751345948129099, -4.999999999999998224 ) ) ;
#41036 = CARTESIAN_POINT ( 'NONE',  ( 2.000000000000001332, 15.31250000122903465, -26.53589838486224650 ) ) ;
#41037 = CARTESIAN_POINT ( 'NONE',  ( 29.16562500061451502, 3.027376345333613106, -5.243569643749998122 ) ) ;
#41038 = CARTESIAN_POINT ( 'NONE',  ( 11.01562500061451821, -6.054752690667223547, -1.112240025338166033E-15 ) ) ;
#41040 = ORIENTED_EDGE ( 'NONE', *, *, #43153, .T. ) ;
#41039=STYLED_ITEM('',(#73144),#21999);
#41041 = CARTESIAN_POINT ( 'NONE',  ( 26.35312500061451857, -4.541064518000417216, -2.621784821875001281 ) ) ;
#41042 = CARTESIAN_POINT ( 'NONE',  ( 8.540625000614518569, 6.054752690667223547, 3.707466751127219781E-16 ) ) ;
#41043 = CARTESIAN_POINT ( 'NONE',  ( 3.215625000614518836, 3.027376345333611329, 5.243569643749999010 ) ) ;
#41044 = CARTESIAN_POINT ( 'NONE',  ( 15.27187500061451786, 2.746126346562645981, -4.756430356249997438 ) ) ;
#41045 = EDGE_CURVE ( 'NONE', #55745, #54151, #46265, .T. ) ;
#41046 = FACE_OUTER_BOUND ( 'NONE', #27402, .T. ) ;
#41047 = CARTESIAN_POINT ( 'NONE',  ( 12.82499999999999929, 4.330127018922191873, 2.499999999999999556 ) ) ;
#41048 = CARTESIAN_POINT ( 'NONE',  ( 13.28437500061451715, -4.541064518000419881, 2.621784821874995952 ) ) ;
#41049 = CARTESIAN_POINT ( 'NONE',  ( 10.12500000122903465, 2.886751345948129099, -4.999999999999998224 ) ) ;
#41050 = CARTESIAN_POINT ( 'NONE',  ( 15.87187500061451573, 3.027376345333611329, 5.243569643749999010 ) ) ;
#41051 = CARTESIAN_POINT ( 'NONE',  ( 18.33749999999999858, -2.886751345948129988, 4.999999999999997335 ) ) ;
#41052 = CARTESIAN_POINT ( 'NONE',  ( 7.846875000614518036, -3.027376345333614438, 5.243569643749998122 ) ) ;
#41053 = CARTESIAN_POINT ( 'NONE',  ( -4.243569643749999898, 10.80312500061451786, -30.00000000000000000 ) ) ;
#41054 = DIRECTION ( 'NONE',  ( 0.000000000000000000, 0.000000000000000000, -1.000000000000000000 ) ) ;
#41055 = CARTESIAN_POINT ( 'NONE',  ( 23.48437500061451289, -2.746126346562646425, 4.756430356249996549 ) ) ;
#41056 = VERTEX_POINT ( 'NONE', #24620 ) ;
#41057 = CARTESIAN_POINT ( 'NONE',  ( 25.49062500061451786, -3.027376345333610441, -5.243569643749999898 ) ) ;
#41058 = CARTESIAN_POINT ( 'NONE',  ( 4.898587196589412829E-16, 27.50000000000000000, 34.00000000000000000 ) ) ;
#41059 = CARTESIAN_POINT ( 'NONE',  ( 27.60937500061451644, 0.000000000000000000, 5.243569643749999010 ) ) ;
#41060 = CARTESIAN_POINT ( 'NONE',  ( 23.43750000000000000, -2.886751345948125991, -5.000000000000000000 ) ) ;
#41061 = CARTESIAN_POINT ( 'NONE',  ( 7.078125000614516438, 6.421520780324663323E-16, -5.243569643749999010 ) ) ;
#41062 = CARTESIAN_POINT ( 'NONE',  ( 24.57187500061451502, 5.824947211148865298E-16, -4.756430356249998326 ) ) ;
#41063 = CARTESIAN_POINT ( 'NONE',  ( 18.42187500061451644, 3.027376345333613106, -5.243569643749998122 ) ) ;
#41064 = CARTESIAN_POINT ( 'NONE',  ( 11.55937500061451573, 2.746126346562645981, -4.756430356249997438 ) ) ;
#41065 = CARTESIAN_POINT ( 'NONE',  ( 29.21250000122903145, 0.000000000000000000, 4.999999999999998224 ) ) ;
#41066 = CARTESIAN_POINT ( 'NONE',  ( 8.671875000614518214, 3.027376345333611329, 5.243569643749999010 ) ) ;
#41067 = ORIENTED_EDGE ( 'NONE', *, *, #30679, .F. ) ;
#41068 = CARTESIAN_POINT ( 'NONE',  ( 18.83437500061451431, 6.421520780324663323E-16, -5.243569643749999010 ) ) ;
#41069 = CYLINDRICAL_SURFACE ( 'NONE', #7774, 3.999999999999996447 ) ;
#41070 = CARTESIAN_POINT ( 'NONE',  ( 27.86249999999999716, -5.773502691896255534, -1.060575238724906372E-15 ) ) ;
#41071 = CARTESIAN_POINT ( 'NONE',  ( 29.37187500061451928, 3.027376345333611329, 5.243569643749999010 ) ) ;
#41072 = CARTESIAN_POINT ( 'NONE',  ( 1.592000809091587073E-14, 16.85000000122903785, -34.00000000000000000 ) ) ;
#41073 = CARTESIAN_POINT ( 'NONE',  ( -1.487416814333745711E-14, 15.72500000122903430, -26.00000000000000000 ) ) ;
#41074 = EDGE_LOOP ( 'NONE', ( #26068, #1551, #24275, #4658 ) ) ;
#41075 = CARTESIAN_POINT ( 'NONE',  ( 11.32500000000000107, 6.123233995736764310E-16, -4.999999999999998224 ) ) ;
#41076 = CARTESIAN_POINT ( 'NONE',  ( 11.67187500061451644, 4.119189519843966529, 2.378215178124999607 ) ) ;
#41077 = CARTESIAN_POINT ( 'NONE',  ( 23.76562500061451644, 3.027376345333613106, -5.243569643749998122 ) ) ;
#41078 = CARTESIAN_POINT ( 'NONE',  ( 15.37500000000000000, 6.123233995736764310E-16, -4.999999999999998224 ) ) ;
#41079 = EDGE_CURVE ( 'NONE', #36820, #16786, #33525, .T. ) ;
#41080 = CARTESIAN_POINT ( 'NONE',  ( 8.587500001229035007, -4.330127018922194537, 2.499999999999995559 ) ) ;
#41081 = CARTESIAN_POINT ( 'NONE',  ( 7.565625000614518036, 3.027376345333613106, -5.243569643749998122 ) ) ;
#41082 = CARTESIAN_POINT ( 'NONE',  ( 20.92500000000000071, 4.330127018922191873, 2.499999999999999556 ) ) ;
#41083 = CARTESIAN_POINT ( 'NONE',  ( 20.80312500061451431, 0.000000000000000000, 5.243569643749999010 ) ) ;
#41084 = CARTESIAN_POINT ( 'NONE',  ( 1.012874171167973181, -4.999999999999998224, -1.012874171167973181 ) ) ;
#41085 = CARTESIAN_POINT ( 'NONE',  ( 25.05000000122903714, 5.773502691896255534, 3.535250795749688894E-16 ) ) ;
#41086 = CARTESIAN_POINT ( 'NONE',  ( 3.756430356249998770, 18.00312499938548427, 32.16877607737301759 ) ) ;
#41087 = CARTESIAN_POINT ( 'NONE',  ( 4.949999999999999289, -4.330127018922190985, -2.500000000000001332 ) ) ;
#41088 = VERTEX_POINT ( 'NONE', #2826 ) ;
#41089 = CARTESIAN_POINT ( 'NONE',  ( 21.96562500061451573, 3.027376345333613106, -5.243569643749998122 ) ) ;
#41090 = CARTESIAN_POINT ( 'NONE',  ( 27.47812500061451502, 4.541064518000418104, 2.621784821874999949 ) ) ;
#41091 = CARTESIAN_POINT ( 'NONE',  ( 27.72187500061451715, -6.054752690667223547, -1.112240025338166033E-15 ) ) ;
#41092 = CARTESIAN_POINT ( 'NONE',  ( 15.51562500061451644, -6.054752690667223547, -1.112240025338166033E-15 ) ) ;
#41093 = CYLINDRICAL_SURFACE ( 'NONE', #47468, 3.999999999999996447 ) ;
#41094 =( BOUNDED_CURVE ( )  B_SPLINE_CURVE ( 2, ( #62859, #57317, #65780, #42885, #3373, #71701, #25146, #54701, #64679 ),
 .UNSPECIFIED., .F., .F. ) 
 B_SPLINE_CURVE_WITH_KNOTS ( ( 3, 2, 2, 2, 3 ),
 ( 0.3750000000000000000, 0.3796296296296296502, 0.3888888888888888951, 0.3981481481481481399, 0.4027777777777777901 ),
 .UNSPECIFIED. ) 
 CURVE ( )  GEOMETRIC_REPRESENTATION_ITEM ( )  RATIONAL_B_SPLINE_CURVE ( ( 0.9330127018922194093, 0.9330127018922194093, 1.000000000000000000, 0.8660254037844387076, 1.000000000000000000, 0.8660254037844387076, 1.000000000000000000, 0.9330127018922189652, 0.9330127018922194093 ) ) 
 REPRESENTATION_ITEM ( '' )  );
#41095 = CARTESIAN_POINT ( 'NONE',  ( 25.42500000122903359, 2.886751345948129099, -4.999999999999998224 ) ) ;
#41096 = CARTESIAN_POINT ( 'NONE',  ( 21.12187500061451573, 2.746126346562645981, -4.756430356249997438 ) ) ;
#41097 = CARTESIAN_POINT ( 'NONE',  ( 16.22812500061451857, 4.541064518000418104, 2.621784821874999949 ) ) ;
#41098 = CARTESIAN_POINT ( 'NONE',  ( 1.592000809091587073E-14, 16.73750000000000071, -34.00000000000000000 ) ) ;
#41099 = CARTESIAN_POINT ( 'NONE',  ( 4.575000001229033941, -5.773502691896255534, -1.060575238724906372E-15 ) ) ;
#41100 = CARTESIAN_POINT ( 'NONE',  ( 10.84687500061451892, 6.054752690667223547, 3.707466751127219781E-16 ) ) ;
#41101 = CARTESIAN_POINT ( 'NONE',  ( 13.13437500061451857, 4.541064518000418104, 2.621784821874999949 ) ) ;
#41102 = CARTESIAN_POINT ( 'NONE',  ( 19.20937500061451786, -4.541064518000417216, -2.621784821875001281 ) ) ;
#41103 = ORIENTED_EDGE ( 'NONE', *, *, #56240, .T. ) ;
#41104 = CARTESIAN_POINT ( 'NONE',  ( -1.587936087009578445, 9.880963660774181534, 24.20021078848421681 ) ) ;
#41105 = CARTESIAN_POINT ( 'NONE',  ( 23.12812500061451360, -4.541064518000419881, 2.621784821874995952 ) ) ;
#41106 = CARTESIAN_POINT ( 'NONE',  ( 19.92187500061451644, 3.027376345333611329, 5.243569643749999010 ) ) ;
#41107 = CARTESIAN_POINT ( 'NONE',  ( 23.99062500061451786, -3.027376345333614438, 5.243569643749998122 ) ) ;
#41108 = CARTESIAN_POINT ( 'NONE',  ( 1.071796769724479237, 18.83615380933863293, 25.99999999999999645 ) ) ;
#41109 = CARTESIAN_POINT ( 'NONE',  ( -3.999999999999999112, 14.15000000000000036, 30.00000000000000000 ) ) ;
#41110 = CARTESIAN_POINT ( 'NONE',  ( 2.859375000614519546, 0.000000000000000000, 5.243569643749999010 ) ) ;
#41111 = CARTESIAN_POINT ( 'NONE',  ( 9.187500001229034652, 6.123233995736764310E-16, -4.999999999999998224 ) ) ;
#41112 = CARTESIAN_POINT ( 'NONE',  ( 4.725000001229034297, 2.886751345948129099, -4.999999999999998224 ) ) ;
#41113 = CARTESIAN_POINT ( 'NONE',  ( 21.30000000000000071, 4.330127018922192761, -2.499999999999997780 ) ) ;
#41114 = CARTESIAN_POINT ( 'NONE',  ( 27.26250000122903216, 4.330127018922192761, -2.499999999999997780 ) ) ;
#41115 = CARTESIAN_POINT ( 'NONE',  ( -3.756430356249999214, 13.84062499938548463, 27.83122392262697531 ) ) ;
#41116 = CARTESIAN_POINT ( 'NONE',  ( 9.534375000614517148, 4.541064518000418104, 2.621784821874999949 ) ) ;
#41117 = CARTESIAN_POINT ( 'NONE',  ( 7.724999999999999645, 6.123233995736764310E-16, -4.999999999999998224 ) ) ;
#41118 = CARTESIAN_POINT ( 'NONE',  ( 18.44062500061451715, 6.054752690667223547, 3.707466751127219781E-16 ) ) ;
#41119 = CARTESIAN_POINT ( 'NONE',  ( 11.85937500061451644, 0.000000000000000000, 5.243569643749999010 ) ) ;
#41120 = CARTESIAN_POINT ( 'NONE',  ( 29.51250000122903216, 4.330127018922192761, -2.499999999999997780 ) ) ;
#41121 = CARTESIAN_POINT ( 'NONE',  ( 20.93437500061451573, -4.541064518000419881, 2.621784821874995952 ) ) ;
#41122 = CARTESIAN_POINT ( 'NONE',  ( 7.171875000614517326, 3.027376345333613106, -5.243569643749998122 ) ) ;
#41123 = CARTESIAN_POINT ( 'NONE',  ( 3.290625000614516793, -3.027376345333614438, 5.243569643749998122 ) ) ;
#41124 = CARTESIAN_POINT ( 'NONE',  ( 2.000000000000001332, 16.21250000122903501, 33.46410161513774995 ) ) ;
#41125 = CARTESIAN_POINT ( 'NONE',  ( 7.940625000614518036, -3.027376345333610441, -5.243569643749999898 ) ) ;
#41126 = CARTESIAN_POINT ( 'NONE',  ( 17.35312500061451502, -4.541064518000417216, -2.621784821875001281 ) ) ;
#41127 =( BOUNDED_CURVE ( )  B_SPLINE_CURVE ( 2, ( #37535, #54170, #31998, #30893, #8728, #26090, #25353 ),
 .UNSPECIFIED., .F., .F. ) 
 B_SPLINE_CURVE_WITH_KNOTS ( ( 3, 2, 2, 3 ),
 ( 0.5999999999999999778, 0.6033333333333334991, 0.6066666666666667984, 0.6100000000000002087 ),
 .UNSPECIFIED. ) 
 CURVE ( )  GEOMETRIC_REPRESENTATION_ITEM ( )  RATIONAL_B_SPLINE_CURVE ( ( 1.000000000000000000, 0.8660254037844387076, 1.000000000000000000, 0.8660254037844387076, 1.000000000000000000, 0.8660254037844298258, 1.000000000000008882 ) ) 
 REPRESENTATION_ITEM ( '' )  );
#41128 = EDGE_LOOP ( 'NONE', ( #66096, #17444, #17710, #28561 ) ) ;
#41129 = CARTESIAN_POINT ( 'NONE',  ( 6.600000001229032520, 5.773502691896255534, 3.535250795749688894E-16 ) ) ;
#41130 = CARTESIAN_POINT ( 'NONE',  ( 13.86562500061451431, 3.027376345333613106, -5.243569643749998122 ) ) ;
#41131 = CARTESIAN_POINT ( 'NONE',  ( 13.79062500061451502, -3.027376345333610441, -5.243569643749999898 ) ) ;
#41132 = CARTESIAN_POINT ( 'NONE',  ( 22.54687500061451999, 5.492252693125287522, 3.363034840372157021E-16 ) ) ;
#41133 = CARTESIAN_POINT ( 'NONE',  ( 12.52500000000000213, -4.330127018922194537, 2.499999999999995559 ) ) ;
#41134 = EDGE_CURVE ( 'NONE', #26352, #48852, #51719, .T. ) ;
#41135 = CARTESIAN_POINT ( 'NONE',  ( 6.975000001229032520, 2.886751345948129099, -4.999999999999998224 ) ) ;
#41136 = CARTESIAN_POINT ( 'NONE',  ( 14.85937500061451644, 4.541064518000418104, -2.621784821874998173 ) ) ;
#41137 = CARTESIAN_POINT ( 'NONE',  ( 19.08750000122903145, 6.123233995736764310E-16, -4.999999999999998224 ) ) ;
#41138 = CARTESIAN_POINT ( 'NONE',  ( 25.12499999999999645, -4.330127018922194537, 2.499999999999995559 ) ) ;
#41139 =( BOUNDED_CURVE ( )  B_SPLINE_CURVE ( 2, ( #59374, #2516, #53862, #25782, #48319, #18396, #40963 ),
 .UNSPECIFIED., .F., .F. ) 
 B_SPLINE_CURVE_WITH_KNOTS ( ( 3, 2, 2, 3 ),
 ( 0.5000000000000000000, 0.5027777777777777679, 0.5055555555555556468, 0.5083333333333334147 ),
 .UNSPECIFIED. ) 
 CURVE ( )  GEOMETRIC_REPRESENTATION_ITEM ( )  RATIONAL_B_SPLINE_CURVE ( ( 1.000000000000000000, 0.8660254037844387076, 1.000000000000000000, 0.8660254037844387076, 1.000000000000000000, 0.8660254037844333785, 1.000000000000005329 ) ) 
 REPRESENTATION_ITEM ( '' )  );
#41140 = CARTESIAN_POINT ( 'NONE',  ( -2.121784821874996840, 18.07812500061451644, -26.32496088578401583 ) ) ;
#41141 = CARTESIAN_POINT ( 'NONE',  ( -4.000000000000000000, 13.17500000000000071, 30.00000000000000000 ) ) ;
#41142 = CARTESIAN_POINT ( 'NONE',  ( 0.000000000000000000, 27.50000000000000000, 30.00000000000000000 ) ) ;
#41143 = CARTESIAN_POINT ( 'NONE',  ( 9.600000001229034297, -2.886751345948126435, -5.000000000000000000 ) ) ;
#41144 = CARTESIAN_POINT ( 'NONE',  ( 13.98750000000000071, -2.886751345948193048, -4.999999999999883649 ) ) ;
#41145 = CARTESIAN_POINT ( 'NONE',  ( 19.47187500061451360, 3.027376345333611329, 5.243569643749999010 ) ) ;
#41146 = CARTESIAN_POINT ( 'NONE',  ( 10.65000000122903323, 5.773502691896255534, 3.535250795749688401E-16 ) ) ;
#41147 = CARTESIAN_POINT ( 'NONE',  ( 14.16562500061451679, -6.054752690667223547, -1.112240025338166033E-15 ) ) ;
#41148 = CARTESIAN_POINT ( 'NONE',  ( 9.881250001229032520, -4.330127018922194537, 2.499999999999995559 ) ) ;
#41149 = CARTESIAN_POINT ( 'NONE',  ( 0.6945855708053418898, 20.89427347822356751, 33.93923227099254092 ) ) ;
#41150 = CARTESIAN_POINT ( 'NONE',  ( 25.65937500061451715, 4.541064518000418104, -2.621784821874998173 ) ) ;
#41151 = CARTESIAN_POINT ( 'NONE',  ( 18.08437500061451075, -2.746126346562646425, 4.756430356249996549 ) ) ;
#41152 = CARTESIAN_POINT ( 'NONE',  ( 11.20312500061451644, 4.541064518000418104, -2.621784821874998173 ) ) ;
#41153 = CARTESIAN_POINT ( 'NONE',  ( 15.19687500061451857, -3.027376345333610441, -5.243569643749999898 ) ) ;
#41154 = ORIENTED_EDGE ( 'NONE', *, *, #25568, .T. ) ;
#41155 = CARTESIAN_POINT ( 'NONE',  ( 27.77812500061451573, 6.421520780324663323E-16, -5.243569643749999010 ) ) ;
#41156 = CARTESIAN_POINT ( 'NONE',  ( 20.99062500061451431, -3.027376345333610441, -5.243569643749999898 ) ) ;
#41157 = CARTESIAN_POINT ( 'NONE',  ( 29.42812500061451431, -4.541064518000419881, 2.621784821874995952 ) ) ;
#41158 = CARTESIAN_POINT ( 'NONE',  ( 3.999999999999999112, 14.82500000000000107, 30.00000000000000000 ) ) ;
#41159 = CARTESIAN_POINT ( 'NONE',  ( 11.02500000000000036, 4.330127018922191873, 2.499999999999999556 ) ) ;
#41160 = CARTESIAN_POINT ( 'NONE',  ( 19.01250000122903216, -4.330127018922190985, -2.500000000000001332 ) ) ;
#41161 = CARTESIAN_POINT ( 'NONE',  ( 23.32500000122903216, 2.886751345948143754, 4.999999999999969802 ) ) ;
#41162 = CARTESIAN_POINT ( 'NONE',  ( 9.796875000614514661, 4.119189519843966529, -2.378215178124998275 ) ) ;
#41163 = VERTEX_POINT ( 'NONE', #31999 ) ;
#41164 = CARTESIAN_POINT ( 'NONE',  ( 16.53750000000000142, -2.886751345948129988, 4.999999999999997335 ) ) ;
#41165 = CARTESIAN_POINT ( 'NONE',  ( 20.69999999999999929, -4.330127018922190985, -2.500000000000001332 ) ) ;
#41166 = CARTESIAN_POINT ( 'NONE',  ( 18.00937500061451502, 4.541064518000418104, -2.621784821874998173 ) ) ;
#41167 = CARTESIAN_POINT ( 'NONE',  ( 14.95312500061451644, 0.000000000000000000, 5.243569643749999010 ) ) ;
#41168 = ADVANCED_FACE ( 'NONE', ( #47900 ), #58596, .T. ) ;
#41169 = ORIENTED_EDGE ( 'NONE', *, *, #65842, .T. ) ;
#41170 = CARTESIAN_POINT ( 'NONE',  ( 19.83750000000000213, -2.886751345948126435, -5.000000000000000000 ) ) ;
#41171 = CARTESIAN_POINT ( 'NONE',  ( 4.903125000614516615, 4.541064518000418104, -2.621784821874998173 ) ) ;
#41172 = CARTESIAN_POINT ( 'NONE',  ( 12.07499999999999929, -4.330127018922194537, 2.499999999999995559 ) ) ;
#41173 = CARTESIAN_POINT ( 'NONE',  ( 28.35937500061451644, 2.746126346562643317, 4.756430356249998326 ) ) ;
#41174 = CARTESIAN_POINT ( 'NONE',  ( 4.243569643749999010, 16.91562500061451502, 27.54997392385601174 ) ) ;
#41175 = CARTESIAN_POINT ( 'NONE',  ( 2.934375000614518392, -4.541064518000419881, 2.621784821874995952 ) ) ;
#41176 = CARTESIAN_POINT ( 'NONE',  ( 10.98750000000000071, 5.773502691896255534, 3.535250795749688894E-16 ) ) ;
#41177 = CARTESIAN_POINT ( 'NONE',  ( -3.756430356249999214, 16.87812499938548427, 27.83122392262697531 ) ) ;
#41178 = CARTESIAN_POINT ( 'NONE',  ( 25.09687500061451715, -3.027376345333610441, -5.243569643749999898 ) ) ;
#41179 = VERTEX_POINT ( 'NONE', #3568 ) ;
#41180 = CARTESIAN_POINT ( 'NONE',  ( 21.70312500061451644, 0.000000000000000000, 5.243569643749999010 ) ) ;
#41181 = CARTESIAN_POINT ( 'NONE',  ( 22.28437500061451715, -4.541064518000419881, 2.621784821874995952 ) ) ;
#41182 = CARTESIAN_POINT ( 'NONE',  ( -2.121784821874999949, 15.67812500061459247, -33.67503911421598417 ) ) ;
#41183 = CARTESIAN_POINT ( 'NONE',  ( 7.040625000614517681, -3.027376345333610441, -5.243569643749999898 ) ) ;
#41184 = CARTESIAN_POINT ( 'NONE',  ( 28.47187500061451715, 2.746126346562643317, 4.756430356249998326 ) ) ;
#41185 = CARTESIAN_POINT ( 'NONE',  ( 25.07812500061451644, 6.421520780324663323E-16, -5.243569643749999010 ) ) ;
#41186 = CARTESIAN_POINT ( 'NONE',  ( 28.50937500061451502, -5.492252693125287522, -1.008910452111647106E-15 ) ) ;
#41187 = CARTESIAN_POINT ( 'NONE',  ( 10.62187500061451928, -5.492252693125287522, -1.008910452111647106E-15 ) ) ;
#41188 = CARTESIAN_POINT ( 'NONE',  ( 17.67187500061451644, 3.027376345333611329, 5.243569643749999010 ) ) ;
#41189 = CARTESIAN_POINT ( 'NONE',  ( 19.73437500061451644, 6.421520780324663323E-16, -5.243569643749999010 ) ) ;
#41190 = CARTESIAN_POINT ( 'NONE',  ( 27.12187500061451573, 3.027376345333611329, 5.243569643749999010 ) ) ;
#41191 = CARTESIAN_POINT ( 'NONE',  ( -3.000416591977282496E-16, 17.49687500061451573, 25.09994784771203058 ) ) ;
#41192 = CARTESIAN_POINT ( 'NONE',  ( 8.315625000614515372, -6.054752690667223547, -1.112240025338166033E-15 ) ) ;
#41193 = CARTESIAN_POINT ( 'NONE',  ( 7.320879633048903241E-15, 18.08749999999999858, -34.00000000000000000 ) ) ;
#41194 = CARTESIAN_POINT ( 'NONE',  ( 5.596875000614516260, -3.027376345333614438, 5.243569643749998122 ) ) ;
#41195 = CARTESIAN_POINT ( 'NONE',  ( 4.000000000000000000, 17.44999999999999929, 30.00000000000000000 ) ) ;
#41196 = CARTESIAN_POINT ( 'NONE',  ( 5.465625000614517504, 3.027376345333611329, 5.243569643749999010 ) ) ;
#41197 = CARTESIAN_POINT ( 'NONE',  ( 10.50937500061451679, 0.000000000000000000, 5.243569643749999010 ) ) ;
#41198 = CARTESIAN_POINT ( 'NONE',  ( 17.28750000122903430, 6.123233995736764310E-16, -4.999999999999998224 ) ) ;
#41199 = CARTESIAN_POINT ( 'NONE',  ( 5.596875000614516260, -3.027376345333614438, 5.243569643749998122 ) ) ;
#41200 = CARTESIAN_POINT ( 'NONE',  ( 8.053125000614516082, 4.541064518000418104, -2.621784821874998173 ) ) ;
#41201 = CARTESIAN_POINT ( 'NONE',  ( 4.000000000000000000, 14.69374999877096677, 30.00000000000000000 ) ) ;
#41202 = CARTESIAN_POINT ( 'NONE',  ( 23.60625000122903216, 4.330127018922192761, -2.499999999999997780 ) ) ;
#41203 = CARTESIAN_POINT ( 'NONE',  ( 16.69687500061451502, 6.054752690667223547, 3.707466751127219781E-16 ) ) ;
#41204 = CARTESIAN_POINT ( 'NONE',  ( 27.63749999999999929, 5.773502691896255534, 3.535250795749688401E-16 ) ) ;
#41205 = VERTEX_POINT ( 'NONE', #70428 ) ;
#41206 = CARTESIAN_POINT ( 'NONE',  ( 24.55312500061451786, -4.541064518000417216, -2.621784821875001281 ) ) ;
#41207 = CARTESIAN_POINT ( 'NONE',  ( 10.37812500061451715, 4.541064518000418104, 2.621784821874999949 ) ) ;
#41208 = CARTESIAN_POINT ( 'NONE',  ( 27.94687500061451502, 6.054752690667223547, 3.707466751127219781E-16 ) ) ;
#41209 = CARTESIAN_POINT ( 'NONE',  ( 9.590625000614517504, -3.027376345333614438, 5.243569643749998122 ) ) ;
#41210 = CARTESIAN_POINT ( 'NONE',  ( -2.121784821874999949, 10.78437500061451715, -33.67503911421598417 ) ) ;
#41211 = CARTESIAN_POINT ( 'NONE',  ( 10.42500000122903536, -5.773502691896255534, -1.060575238724906372E-15 ) ) ;
#41212 = CARTESIAN_POINT ( 'NONE',  ( 24.62812500061451715, 6.421520780324663323E-16, -5.243569643749999010 ) ) ;
#41213 = CARTESIAN_POINT ( 'NONE',  ( -2.121784821874999949, 13.42812500061451786, -33.67503911421598417 ) ) ;
#41214 = CARTESIAN_POINT ( 'NONE',  ( 12.07500000122903216, 2.886751345948126879, 4.999999999999999112 ) ) ;
#41215 = CARTESIAN_POINT ( 'NONE',  ( 23.16562500061451502, -6.054752690667223547, -1.112240025338166033E-15 ) ) ;
#41216 = CARTESIAN_POINT ( 'NONE',  ( 11.73750000000000249, -2.886751345948125991, -5.000000000000000000 ) ) ;
#41217 = CARTESIAN_POINT ( 'NONE',  ( 19.75312500061451360, 4.541064518000418104, -2.621784821874998173 ) ) ;
#41218 = DIRECTION ( 'NONE',  ( 1.000000000000000000, 0.000000000000000000, -0.000000000000000000 ) ) ;
#41219 = CARTESIAN_POINT ( 'NONE',  ( 21.48750000000000071, -2.886751345948129988, 4.999999999999997335 ) ) ;
#41220 = CARTESIAN_POINT ( 'NONE',  ( 14.13750000122903394, 6.123233995736764310E-16, -4.999999999999998224 ) ) ;
#41221 = CARTESIAN_POINT ( 'NONE',  ( 9.815625000614518925, 3.027376345333613106, -5.243569643749998122 ) ) ;
#41222 = CARTESIAN_POINT ( 'NONE',  ( 16.79062500061451857, -3.027376345333614438, 5.243569643749998122 ) ) ;
#41223 = CARTESIAN_POINT ( 'NONE',  ( 24.63750000122903216, 4.330127018922191873, 2.499999999999999556 ) ) ;
#41224 = CARTESIAN_POINT ( 'NONE',  ( 20.29687500061451644, 6.054752690667223547, 3.707466751127219781E-16 ) ) ;
#41225 = CARTESIAN_POINT ( 'NONE',  ( 7.650000001229034119, -2.886751345948129988, 4.999999999999997335 ) ) ;
#41226 = CARTESIAN_POINT ( 'NONE',  ( 9.384375000614518569, 6.421520780324663323E-16, -5.243569643749999010 ) ) ;
#41227 = CARTESIAN_POINT ( 'NONE',  ( 24.60937500061451644, -4.541064518000417216, -2.621784821875001281 ) ) ;
#41228 = CARTESIAN_POINT ( 'NONE',  ( 2.896875000614518747, -3.027376345333614438, 5.243569643749998122 ) ) ;
#41229 = EDGE_CURVE ( 'NONE', #72689, #68632, #20904, .T. ) ;
#41230 = CARTESIAN_POINT ( 'NONE',  ( 21.92812500061451431, 6.421520780324663323E-16, -5.243569643749999010 ) ) ;
#41231 = CARTESIAN_POINT ( 'NONE',  ( 26.89687500061451431, -3.027376345333610441, -5.243569643749999898 ) ) ;
#41232 = CARTESIAN_POINT ( 'NONE',  ( 1.878215178125000495, 17.32812499938548356, 26.74683588394047007 ) ) ;
#41233 = CYLINDRICAL_SURFACE ( 'NONE', #72779, 4.999999999999998224 ) ;
#41234 = CARTESIAN_POINT ( 'NONE',  ( 8.296875000614516438, -3.027376345333614438, 5.243569643749998122 ) ) ;
#41235 = CARTESIAN_POINT ( 'NONE',  ( 16.26562500061451289, 3.027376345333611329, 5.243569643749999010 ) ) ;
#41236 = ORIENTED_EDGE ( 'NONE', *, *, #29224, .F. ) ;
#41237 = CARTESIAN_POINT ( 'NONE',  ( -3.999999999999997335, 12.83750000000000213, -27.69059892324149530 ) ) ;
#41238 = CARTESIAN_POINT ( 'NONE',  ( 26.80312500061451431, -4.541064518000417216, -2.621784821875001281 ) ) ;
#41239 = CARTESIAN_POINT ( 'NONE',  ( 4.621875000614516615, 3.027376345333611329, 5.243569643749999010 ) ) ;
#41240 = CARTESIAN_POINT ( 'NONE',  ( 28.08749999999999858, 5.773502691896255534, 3.535250795749688401E-16 ) ) ;
#41241 = CARTESIAN_POINT ( 'NONE',  ( -4.243569643749999898, 19.80312500061451786, -30.00000000000000000 ) ) ;
#41242 = CARTESIAN_POINT ( 'NONE',  ( 17.73750000000000071, 5.773502691896255534, 3.535250795749688894E-16 ) ) ;
#41243 = CARTESIAN_POINT ( 'NONE',  ( 21.32812500061451644, -4.541064518000419881, 2.621784821874995952 ) ) ;
#41244 = ORIENTED_EDGE ( 'NONE', *, *, #20037, .T. ) ;
#41245 = CARTESIAN_POINT ( 'NONE',  ( 24.75000000000000000, -4.330127018922190985, -2.500000000000001332 ) ) ;
#41246 = CARTESIAN_POINT ( 'NONE',  ( 25.65937500061451715, 4.541064518000418104, -2.621784821874998173 ) ) ;
#41247 = EDGE_CURVE ( 'NONE', #69279, #58357, #5707, .T. ) ;
#41248 = ORIENTED_EDGE ( 'NONE', *, *, #24697, .T. ) ;
#41249 = CARTESIAN_POINT ( 'NONE',  ( 12.70312500061451821, 0.000000000000000000, 5.243569643749999010 ) ) ;
#41250 = CARTESIAN_POINT ( 'NONE',  ( 6.403125000614517504, 0.000000000000000000, 5.243569643749999010 ) ) ;
#41251 = CARTESIAN_POINT ( 'NONE',  ( 17.74687500061451928, -4.119189519843965641, -2.378215178125001383 ) ) ;
#41252 = CARTESIAN_POINT ( 'NONE',  ( 29.09062500061451573, -3.027376345333610441, -5.243569643749999898 ) ) ;
#41253 = CARTESIAN_POINT ( 'NONE',  ( 15.93750000122903110, 6.123233995736764310E-16, -4.999999999999998224 ) ) ;
#41254 = CARTESIAN_POINT ( 'NONE',  ( 21.71249999999999858, 2.886751345948129099, -4.999999999999998224 ) ) ;
#41255 = CARTESIAN_POINT ( 'NONE',  ( 28.57499999999999929, 4.330127018922191873, 2.499999999999999556 ) ) ;
#41256 = CARTESIAN_POINT ( 'NONE',  ( 5.109375000614518214, 0.000000000000000000, 5.243569643749999010 ) ) ;
#41257 = CARTESIAN_POINT ( 'NONE',  ( 9.984375000614518214, 4.541064518000418104, 2.621784821874999949 ) ) ;
#41258 = CARTESIAN_POINT ( 'NONE',  ( 19.24687500061452283, -3.027376345333610441, -5.243569643749999898 ) ) ;
#41259 = CARTESIAN_POINT ( 'NONE',  ( -3.999999999999999112, 15.16250000122903252, -30.00000000000000000 ) ) ;
#41260 = ORIENTED_EDGE ( 'NONE', *, *, #43169, .F. ) ;
#41261 = CARTESIAN_POINT ( 'NONE',  ( 29.69062500061451715, 6.054752690667223547, 3.707466751127219781E-16 ) ) ;
#41262 = CARTESIAN_POINT ( 'NONE',  ( 29.52187500061451431, -6.054752690667223547, -1.112240025338166033E-15 ) ) ;
#41263 = CARTESIAN_POINT ( 'NONE',  ( 5.559375000614517504, 0.000000000000000000, 5.243569643749999010 ) ) ;
#41264 = CARTESIAN_POINT ( 'NONE',  ( 16.80000000000000071, 4.330127018922192761, -2.499999999999997780 ) ) ;
#41265 = CARTESIAN_POINT ( 'NONE',  ( 14.09062500061451750, -3.027376345333614438, 5.243569643749998122 ) ) ;
#41266 = CARTESIAN_POINT ( 'NONE',  ( 2.000000000000001332, 13.96250000122903323, 33.46410161513774995 ) ) ;
#41267 = CARTESIAN_POINT ( 'NONE',  ( 8.343750001229034652, 5.773502691896255534, 3.535250795749688401E-16 ) ) ;
#41268 = CARTESIAN_POINT ( 'NONE',  ( 20.32500000122903572, -5.773502691896255534, -1.060575238724906372E-15 ) ) ;
#41269 = LINE ( 'NONE', #63781, #60710 ) ;
#41270 = CARTESIAN_POINT ( 'NONE',  ( 19.24687500061452283, -2.746126346562642428, -4.756430356249999214 ) ) ;
#41271 = CARTESIAN_POINT ( 'NONE',  ( 6.628125000614517148, 6.421520780324663323E-16, -5.243569643749999010 ) ) ;
#41272 = CARTESIAN_POINT ( 'NONE',  ( 25.09687500061451715, -3.027376345333610441, -5.243569643749999898 ) ) ;
#41274 = CARTESIAN_POINT ( 'NONE',  ( 4.243569643749999010, 19.67187500061451644, 27.54997392385601174 ) ) ;
#41273 =( BOUNDED_CURVE ( )  B_SPLINE_CURVE ( 2, ( #28562, #22646, #72177, #4587, #45196, #33377, #21557 ),
 .UNSPECIFIED., .F., .F. ) 
 B_SPLINE_CURVE_WITH_KNOTS ( ( 3, 2, 2, 3 ),
 ( 0.1200000000000000788, 0.1233333333333334059, 0.1266666666666667329, 0.1300000000000000322 ),
 .UNSPECIFIED. ) 
 CURVE ( )  GEOMETRIC_REPRESENTATION_ITEM ( )  RATIONAL_B_SPLINE_CURVE ( ( 0.9999999999999966693, 0.8660254037844420383, 1.000000000000000000, 0.8660254037844387076, 1.000000000000000000, 0.8660254037844375974, 1.000000000000001110 ) ) 
 REPRESENTATION_ITEM ( '' )  );
#41275 = CARTESIAN_POINT ( 'NONE',  ( 25.95937500061451431, -4.541064518000417216, -2.621784821875001281 ) ) ;
#41276 = CARTESIAN_POINT ( 'NONE',  ( 8.625000000000000000, 6.123233995736764310E-16, -4.999999999999998224 ) ) ;
#41277 = CARTESIAN_POINT ( 'NONE',  ( 3.999999999999998668, 12.72500000122903430, 27.69059892324149175 ) ) ;
#41278 = CARTESIAN_POINT ( 'NONE',  ( 14.20312500061451644, -4.541064518000417216, -2.621784821875001281 ) ) ;
#41279 = CARTESIAN_POINT ( 'NONE',  ( 6.562500001229032875, 4.330127018922192761, -2.499999999999997780 ) ) ;
#41280 = CARTESIAN_POINT ( 'NONE',  ( 16.80937500061451573, 0.000000000000000000, 5.243569643749999010 ) ) ;
#41281 = CARTESIAN_POINT ( 'NONE',  ( 11.03437500061451715, -4.541064518000419881, 2.621784821874995952 ) ) ;
#41282 = DIRECTION ( 'NONE',  ( -1.000000000000000000, -0.000000000000000000, -0.000000000000000000 ) ) ;
#41283 = ORIENTED_EDGE ( 'NONE', *, *, #10973, .F. ) ;
#41284 = CARTESIAN_POINT ( 'NONE',  ( 12.85312500061451502, -4.541064518000417216, -2.621784821875001281 ) ) ;
#41285 = CARTESIAN_POINT ( 'NONE',  ( 28.98750000122903359, 6.123233995736764310E-16, -4.999999999999998224 ) ) ;
#41286 = CARTESIAN_POINT ( 'NONE',  ( 23.40000000122903145, -2.886751345948129988, 4.999999999999997335 ) ) ;
#41287 = CARTESIAN_POINT ( 'NONE',  ( 13.84687500061451537, -3.027376345333610441, -5.243569643749999898 ) ) ;
#41288 = CARTESIAN_POINT ( 'NONE',  ( 13.52812500061451750, 4.541064518000418104, 2.621784821874999949 ) ) ;
#41289 = CARTESIAN_POINT ( 'NONE',  ( 20.90625000122903288, 4.330127018922192761, -2.499999999999997780 ) ) ;
#41290 = CARTESIAN_POINT ( 'NONE',  ( 24.12187500061451217, -6.054752690667223547, -1.112240025338166033E-15 ) ) ;
#41291 = CARTESIAN_POINT ( 'NONE',  ( 3.999999999999998668, 15.87500000122903465, 27.69059892324149530 ) ) ;
#41292 = CARTESIAN_POINT ( 'NONE',  ( 45.00000000000000000, 0.000000000000000000, 0.000000000000000000 ) ) ;
#41293 = CARTESIAN_POINT ( 'NONE',  ( 1.592000809091587073E-14, 15.05000000122903714, 26.00000000000000000 ) ) ;
#41294 = CARTESIAN_POINT ( 'NONE',  ( 4.243569643749999898, 17.79687500061451999, -27.54997392385601529 ) ) ;
#41295 = CARTESIAN_POINT ( 'NONE',  ( 15.38437500061451679, 4.541064518000418104, 2.621784821874999949 ) ) ;
#41296 = CARTESIAN_POINT ( 'NONE',  ( 18.11250000122903359, -4.330127018922190985, -2.500000000000001332 ) ) ;
#41297 = CARTESIAN_POINT ( 'NONE',  ( 12.49687500061451573, -3.027376345333610441, -5.243569643749999898 ) ) ;
#41298 = CARTESIAN_POINT ( 'NONE',  ( 2.121784821874999061, 19.20312500061451644, -33.67503911421598417 ) ) ;
#41299 = CARTESIAN_POINT ( 'NONE',  ( 19.50000000122903288, -2.886751345948125991, -5.000000000000000000 ) ) ;
#41300 = CARTESIAN_POINT ( 'NONE',  ( 12.74062500061451786, -3.027376345333614438, 5.243569643749998122 ) ) ;
#41301 = ORIENTED_EDGE ( 'NONE', *, *, #16676, .T. ) ;
#41302 = ORIENTED_EDGE ( 'NONE', *, *, #9933, .T. ) ;
#41303 = CARTESIAN_POINT ( 'NONE',  ( 18.82500000000000284, -4.330127018922194537, 2.499999999999995559 ) ) ;
#41304 = CARTESIAN_POINT ( 'NONE',  ( 2.000000000000000444, 15.66874999877096464, 26.53589838486224650 ) ) ;
#41305 = CARTESIAN_POINT ( 'NONE',  ( 13.50937500061451679, 4.541064518000418104, -2.621784821874998173 ) ) ;
#41306 = CARTESIAN_POINT ( 'NONE',  ( 3.980152422927321521, 3.026382568917634242, 4.011453763075421008 ) ) ;
#41307 = CARTESIAN_POINT ( 'NONE',  ( 13.05000000122903536, -2.886751345948129988, 4.999999999999997335 ) ) ;
#41308 = CARTESIAN_POINT ( 'NONE',  ( 21.86250000122903003, 4.330127018922192761, -2.499999999999997780 ) ) ;
#41309 = CARTESIAN_POINT ( 'NONE',  ( 17.42812500061451786, 6.421520780324663323E-16, -5.243569643749999010 ) ) ;
#41310 = CARTESIAN_POINT ( 'NONE',  ( 24.14062500061451289, -3.027376345333610441, -5.243569643749999898 ) ) ;
#41311 = CARTESIAN_POINT ( 'NONE',  ( 29.47500000122903430, 2.886751345948129099, -4.999999999999998224 ) ) ;
#41312 = CARTESIAN_POINT ( 'NONE',  ( 28.38749999999999929, -2.886751345948125991, -5.000000000000000000 ) ) ;
#41313 = CARTESIAN_POINT ( 'NONE',  ( 28.03125000122903288, 6.123233995736764310E-16, -4.999999999999998224 ) ) ;
#41314 = CARTESIAN_POINT ( 'NONE',  ( 28.61249999999999716, 2.886751345948126879, 4.999999999999999112 ) ) ;
#41315 = CARTESIAN_POINT ( 'NONE',  ( 0.000000000000000000, 27.50000000000000000, 30.00000000000000000 ) ) ;
#41316 = CARTESIAN_POINT ( 'NONE',  ( 3.939080010846523372, -3.079553322829319928, -4.243980907203444453 ) ) ;
#41317 = CARTESIAN_POINT ( 'NONE',  ( 4.243569643749999898, 16.44687500061451857, -27.54997392385601529 ) ) ;
#41318 = LINE ( 'NONE', #2513, #63117 ) ;
#41319 = CARTESIAN_POINT ( 'NONE',  ( 5.962500000000002132, 2.886751345948129099, -4.999999999999998224 ) ) ;
#41320 =( BOUNDED_CURVE ( )  B_SPLINE_CURVE ( 2, ( #30037, #36674, #47038, #65114, #52577, #8239, #1984, #41493, #64015 ),
 .UNSPECIFIED., .F., .F. ) 
 B_SPLINE_CURVE_WITH_KNOTS ( ( 3, 2, 2, 2, 3 ),
 ( 0.8369565217391304879, 0.8405797101449274944, 0.8478260869565217295, 0.8550724637681159646, 0.8586956521739130821 ),
 .UNSPECIFIED. ) 
 CURVE ( )  GEOMETRIC_REPRESENTATION_ITEM ( )  RATIONAL_B_SPLINE_CURVE ( ( 0.9330127018922192983, 0.9330127018922202975, 1.000000000000000000, 0.8660254037844387076, 1.000000000000000000, 0.8660254037844387076, 1.000000000000000000, 0.9330127018922194093, 0.9330127018922194093 ) ) 
 REPRESENTATION_ITEM ( '' )  );
#41321 = CARTESIAN_POINT ( 'NONE',  ( 28.93125000122903145, 6.123233995736764310E-16, -4.999999999999998224 ) ) ;
#41322 = CARTESIAN_POINT ( 'NONE',  ( 10.50937500061451679, 0.000000000000000000, 5.243569643749999010 ) ) ;
#41323 = CARTESIAN_POINT ( 'NONE',  ( 27.36562500061451786, 3.027376345333613106, -5.243569643749998122 ) ) ;
#41324 = CARTESIAN_POINT ( 'NONE',  ( 15.46875000122903110, 2.886751345948129099, -4.999999999999997335 ) ) ;
#41325 = CARTESIAN_POINT ( 'NONE',  ( 3.697207292818405211, -3.366579844074466088, -3.697207292818405211 ) ) ;
#41326 = CARTESIAN_POINT ( 'NONE',  ( -3.137519842735245283E-14, 14.71250000000000213, 34.00000000000000000 ) ) ;
#41327 = EDGE_CURVE ( 'NONE', #12847, #45106, #42356, .T. ) ;
#41328 = CARTESIAN_POINT ( 'NONE',  ( 6.984375000614516438, -4.541064518000419881, 2.621784821874995952 ) ) ;
#41329 = CARTESIAN_POINT ( 'NONE',  ( 10.84687500061451892, 6.054752690667223547, 3.707466751127219781E-16 ) ) ;
#41330 = CARTESIAN_POINT ( 'NONE',  ( 5.887500000000000178, -2.886751345948125991, -5.000000000000000000 ) ) ;
#41331 = CARTESIAN_POINT ( 'NONE',  ( 4.243569643749999010, 15.11562500061459424, 27.54997392385601174 ) ) ;
#41332 = CARTESIAN_POINT ( 'NONE',  ( 4.000000000000000000, 17.93750000000000355, 32.30940107675849760 ) ) ;
#41333 = CARTESIAN_POINT ( 'NONE',  ( 5.512499999999999289, 2.886751345948129099, -4.999999999999998224 ) ) ;
#41334 = CARTESIAN_POINT ( 'NONE',  ( 15.94687500061451502, -4.119189519843965641, -2.378215178125001383 ) ) ;
#41335 = CARTESIAN_POINT ( 'NONE',  ( 19.94062500061451715, -3.027376345333614438, 5.243569643749998122 ) ) ;
#41336 = CARTESIAN_POINT ( 'NONE',  ( 12.96562500061451750, 3.027376345333613106, -5.243569643749998122 ) ) ;
#41337 = CARTESIAN_POINT ( 'NONE',  ( 25.28437500061451360, -2.746126346562646425, 4.756430356249996549 ) ) ;
#41338 = CARTESIAN_POINT ( 'NONE',  ( 8.371875000614515727, -6.054752690667223547, -1.112240025338166033E-15 ) ) ;
#41339 = CARTESIAN_POINT ( 'NONE',  ( 27.11249999999999716, 2.886751345948129099, -4.999999999999998224 ) ) ;
#41340 = CARTESIAN_POINT ( 'NONE',  ( 23.10000000122903074, -2.886751345948125991, -5.000000000000000000 ) ) ;
#41341 = CARTESIAN_POINT ( 'NONE',  ( -1.999999999999997113, 18.38750000122903572, -26.53589838486224295 ) ) ;
#41342 = CARTESIAN_POINT ( 'NONE',  ( 12.19687500061451679, 6.054752690667223547, 3.707466751127219781E-16 ) ) ;
#41343 = CARTESIAN_POINT ( 'NONE',  ( 26.52187500061451431, 3.027376345333613106, -5.243569643749998122 ) ) ;
#41344 = CARTESIAN_POINT ( 'NONE',  ( 28.21875000122902932, 2.886751345948148195, 4.999999999999962697 ) ) ;
#41345 = CARTESIAN_POINT ( 'NONE',  ( 3.999999999999999112, 13.58750000122903323, -30.00000000000000000 ) ) ;
#41346 = CARTESIAN_POINT ( 'NONE',  ( 20.59687500061451360, -3.027376345333610441, -5.243569643749999898 ) ) ;
#41347 = CARTESIAN_POINT ( 'NONE',  ( 12.98437500061451821, 6.421520780324663323E-16, -5.243569643749999010 ) ) ;
#41348 = CARTESIAN_POINT ( 'NONE',  ( 2.655984681222220721E-16, 17.81562499938548427, 25.66244784525396483 ) ) ;
#41349 = CARTESIAN_POINT ( 'NONE',  ( 26.96249999999999858, -5.773502691896255534, -1.060575238724906372E-15 ) ) ;
#41350 = CARTESIAN_POINT ( 'NONE',  ( -1.878215178124999163, 20.44062499938548072, 26.74683588394047007 ) ) ;
#41351 = CARTESIAN_POINT ( 'NONE',  ( -2.121784821874996840, 11.83437500061451786, -26.32496088578401583 ) ) ;
#41352 = CARTESIAN_POINT ( 'NONE',  ( 28.20937500061451786, -4.119189519843965641, -2.378215178125001383 ) ) ;
#41353 = CARTESIAN_POINT ( 'NONE',  ( 14.12812500061451715, -4.541064518000419881, 2.621784821874995952 ) ) ;
#41354 = CARTESIAN_POINT ( 'NONE',  ( 5.437500000000001776, -2.886751345948125991, -5.000000000000000000 ) ) ;
#41355 = CARTESIAN_POINT ( 'NONE',  ( 25.27499999999999858, 6.123233995736764310E-16, -4.999999999999998224 ) ) ;
#41356 = CYLINDRICAL_SURFACE ( 'NONE', #64641, 4.000000000000000000 ) ;
#41357 = CARTESIAN_POINT ( 'NONE',  ( 15.48749999999999893, 5.773502691896255534, 3.535250795749688894E-16 ) ) ;
#41358 = CARTESIAN_POINT ( 'NONE',  ( -4.243569643749999898, 10.31562500061451715, 27.54997392385601529 ) ) ;
#41359 = CARTESIAN_POINT ( 'NONE',  ( 15.15000000122903323, 5.773502691896255534, 3.535250795749688894E-16 ) ) ;
#41360 = CARTESIAN_POINT ( 'NONE',  ( 23.85937500061451644, 4.541064518000418104, -2.621784821874998173 ) ) ;
#41361 = ORIENTED_EDGE ( 'NONE', *, *, #64577, .T. ) ;
#41362 = CARTESIAN_POINT ( 'NONE',  ( 20.12812500061451715, 6.421520780324663323E-16, -5.243569643749999010 ) ) ;
#41363 = CARTESIAN_POINT ( 'NONE',  ( 4.190625000614518925, -3.027376345333614438, 5.243569643749998122 ) ) ;
#41364 = CARTESIAN_POINT ( 'NONE',  ( 19.39687500061451786, 6.054752690667223547, 3.707466751127219781E-16 ) ) ;
#41365 = CARTESIAN_POINT ( 'NONE',  ( 4.162499999999999645, 2.886751345948129099, -4.999999999999998224 ) ) ;
#41366 = CARTESIAN_POINT ( 'NONE',  ( 8.053125000614516082, 4.541064518000418104, -2.621784821874998173 ) ) ;
#41367 = CARTESIAN_POINT ( 'NONE',  ( 21.85312500061451502, -4.541064518000417216, -2.621784821875001281 ) ) ;
#41368 = CARTESIAN_POINT ( 'NONE',  ( 4.243569643749999010, 15.56562500061451715, 27.54997392385601174 ) ) ;
#41369 = CARTESIAN_POINT ( 'NONE',  ( 19.68750000122903288, 4.330127018922191873, 2.499999999999999556 ) ) ;
#41370 = CARTESIAN_POINT ( 'NONE',  ( 11.85937500061451644, 0.000000000000000000, 4.756430356249998326 ) ) ;
#41371 = CARTESIAN_POINT ( 'NONE',  ( 9.140625000614518214, -3.027376345333614438, 5.243569643749998122 ) ) ;
#41372 = CARTESIAN_POINT ( 'NONE',  ( 4.096875000614518925, 6.054752690667223547, 3.707466751127219781E-16 ) ) ;
#41373 = CARTESIAN_POINT ( 'NONE',  ( 28.45312500061451289, 0.000000000000000000, 5.243569643749999010 ) ) ;
#41374 = CARTESIAN_POINT ( 'NONE',  ( 24.30937500061451573, 4.541064518000418104, -2.621784821874998173 ) ) ;
#41375 = CARTESIAN_POINT ( 'NONE',  ( 15.66562500061451857, 3.027376345333613106, -5.243569643749998122 ) ) ;
#41376 = CARTESIAN_POINT ( 'NONE',  ( 24.37500000122903288, -5.773502691896255534, -1.060575238724906372E-15 ) ) ;
#41377 = CARTESIAN_POINT ( 'NONE',  ( 24.89062500061451644, -3.027376345333614438, 5.243569643749998122 ) ) ;
#41378 = CARTESIAN_POINT ( 'NONE',  ( 20.59687500061451360, -3.027376345333610441, -5.243569643749999898 ) ) ;
#41379 = CARTESIAN_POINT ( 'NONE',  ( 15.55312500061451608, -4.541064518000417216, -2.621784821875001281 ) ) ;
#41380 = CARTESIAN_POINT ( 'NONE',  ( 4.243569643749999010, 16.52187500061451786, 27.54997392385601174 ) ) ;
#41381 = CARTESIAN_POINT ( 'NONE',  ( 23.35312500061451857, 4.541064518000418104, -2.621784821874998173 ) ) ;
#41382 = CYLINDRICAL_SURFACE ( 'NONE', #70349, 4.999999999999998224 ) ;
#41383 = ORIENTED_EDGE ( 'NONE', *, *, #35460, .F. ) ;
#41384 = CARTESIAN_POINT ( 'NONE',  ( 26.51249999999999929, -5.773502691896255534, -1.060575238724906372E-15 ) ) ;
#41385 = CARTESIAN_POINT ( 'NONE',  ( -2.828200636599751609E-16, 10.43750000000000178, -34.61880215351700230 ) ) ;
#41386 = CARTESIAN_POINT ( 'NONE',  ( -1.878215178124999163, 20.55312499938548143, 26.74683588394047007 ) ) ;
#41387 = CARTESIAN_POINT ( 'NONE',  ( 28.64062500061451289, -3.027376345333610441, -5.243569643749999898 ) ) ;
#41388 = CARTESIAN_POINT ( 'NONE',  ( 6.778125000614518392, 4.541064518000418104, 2.621784821874999949 ) ) ;
#41389 = CARTESIAN_POINT ( 'NONE',  ( 23.13750000122903216, 6.123233995736764310E-16, -4.999999999999998224 ) ) ;
#41390 = CARTESIAN_POINT ( 'NONE',  ( 27.17812500061451786, -4.541064518000419881, 2.621784821874995952 ) ) ;
#41391 = CARTESIAN_POINT ( 'NONE',  ( 24.33749999999999858, -2.886751345948125991, -5.000000000000000000 ) ) ;
#41392 = CARTESIAN_POINT ( 'NONE',  ( -3.999999999999999112, 16.06250000122903288, -30.00000000000000000 ) ) ;
#41393 = FACE_OUTER_BOUND ( 'NONE', #71275, .T. ) ;
#41394 = CARTESIAN_POINT ( 'NONE',  ( 10.26562500061451644, 3.027376345333613106, -5.243569643749998122 ) ) ;
#41395 = VERTEX_POINT ( 'NONE', #65980 ) ;
#41396 = EDGE_CURVE ( 'NONE', #47145, #19210, #45845, .T. ) ;
#41397 = CARTESIAN_POINT ( 'NONE',  ( 25.00312500061451715, -4.541064518000417216, -2.621784821875001281 ) ) ;
#41398 = CARTESIAN_POINT ( 'NONE',  ( 7.153125000614518392, 4.541064518000418104, -2.621784821874998173 ) ) ;
#41399 = CARTESIAN_POINT ( 'NONE',  ( 4.340625000614515727, -3.027376345333610441, -5.243569643749999898 ) ) ;
#41400 = CARTESIAN_POINT ( 'NONE',  ( 15.49687500061451750, -2.746126346562646425, 4.756430356249996549 ) ) ;
#41401 = CARTESIAN_POINT ( 'NONE',  ( 17.88750000122903216, 4.330127018922191873, 2.499999999999999556 ) ) ;
#41402 = CARTESIAN_POINT ( 'NONE',  ( 13.27500000000000213, 4.330127018922191873, 2.499999999999999556 ) ) ;
#41403 = CARTESIAN_POINT ( 'NONE',  ( 12.60937500061451821, 4.541064518000418104, -2.621784821874998173 ) ) ;
#41404 = CARTESIAN_POINT ( 'NONE',  ( 8.887500001229033941, 4.330127018922191873, 2.499999999999999556 ) ) ;
#41405 = CARTESIAN_POINT ( 'NONE',  ( 16.17187500061451644, 3.027376345333613106, -5.243569643749998122 ) ) ;
#41406 = CARTESIAN_POINT ( 'NONE',  ( 18.52499999999999858, 6.123233995736764310E-16, -4.999999999999998224 ) ) ;
#41407 = CARTESIAN_POINT ( 'NONE',  ( 8.671875000614518214, 3.027376345333611329, 5.243569643749999010 ) ) ;
#41408 = CARTESIAN_POINT ( 'NONE',  ( 2.121784821875001281, 10.50312500061451715, -26.32496088578401938 ) ) ;
#41409 = CARTESIAN_POINT ( 'NONE',  ( -1.999999999999997113, 11.97500000000000142, -26.53589838486224295 ) ) ;
#41410 = CARTESIAN_POINT ( 'NONE',  ( 22.50937500061451502, 2.746126346562643317, 4.756430356249998326 ) ) ;
#41411 = CYLINDRICAL_SURFACE ( 'NONE', #14711, 4.999999999999998224 ) ;
#41412 = CARTESIAN_POINT ( 'NONE',  ( 24.47812500061451502, -4.541064518000419881, 2.621784821874995952 ) ) ;
#41413 = DIRECTION ( 'NONE',  ( -1.000000000000000000, -0.000000000000000000, -0.000000000000000000 ) ) ;
#41414 = CARTESIAN_POINT ( 'NONE',  ( 26.22187500061451715, 3.027376345333611329, 5.243569643749999010 ) ) ;
#41415 = CARTESIAN_POINT ( 'NONE',  ( 28.62187500061451573, -6.054752690667223547, -1.112240025338166033E-15 ) ) ;
#41416 = CARTESIAN_POINT ( 'NONE',  ( 22.76249999999999574, 2.886751345948126879, 4.999999999999999112 ) ) ;
#41417 = CARTESIAN_POINT ( 'NONE',  ( 7.003125000614518036, -4.541064518000417216, -2.621784821875001281 ) ) ;
#41418 = CARTESIAN_POINT ( 'NONE',  ( 25.39687500061451431, -4.119189519843965641, -2.378215178125001383 ) ) ;
#41419 = CARTESIAN_POINT ( 'NONE',  ( 16.20937500061451786, 4.541064518000418104, -2.621784821874998173 ) ) ;
#41420 = CARTESIAN_POINT ( 'NONE',  ( 7.884375000614516793, -2.746126346562641984, -4.756430356249999214 ) ) ;
#41421 = CARTESIAN_POINT ( 'NONE',  ( 3.740625000614516527, -3.027376345333614438, 5.243569643749998122 ) ) ;
#41422 = CARTESIAN_POINT ( 'NONE',  ( 8.896875000614517859, -3.027376345333610441, -5.243569643749999898 ) ) ;
#41423 = ORIENTED_EDGE ( 'NONE', *, *, #60032, .T. ) ;
#41424 = CARTESIAN_POINT ( 'NONE',  ( 18.45937500061451431, 4.541064518000418104, -2.621784821874998173 ) ) ;
#41425 = CARTESIAN_POINT ( 'NONE',  ( 9.956250001229033586, -4.330127018922190985, -2.500000000000001332 ) ) ;
#41426 = CARTESIAN_POINT ( 'NONE',  ( 26.47499999999999787, -4.330127018922194537, 2.499999999999995559 ) ) ;
#41428 = EDGE_CURVE ( 'NONE', #40447, #48472, #36075, .T. ) ;
#41427 = CARTESIAN_POINT ( 'NONE',  ( 3.750000000000000000, 4.330127018922192761, -2.499999999999997780 ) ) ;
#41429 = CARTESIAN_POINT ( 'NONE',  ( 29.77499999999999858, 6.123233995736764310E-16, -4.999999999999998224 ) ) ;
#41430 = ORIENTED_EDGE ( 'NONE', *, *, #58553, .F. ) ;
#41431 = CARTESIAN_POINT ( 'NONE',  ( 11.43750000000000000, 5.773502691896255534, 3.535250795749688894E-16 ) ) ;
#41432 = CARTESIAN_POINT ( 'NONE',  ( 11.70937500061451608, 2.746126346562643317, 4.756430356249998326 ) ) ;
#41433 = CARTESIAN_POINT ( 'NONE',  ( 21.96562500061451573, 3.027376345333613106, -5.243569643749998122 ) ) ;
#41434 = CARTESIAN_POINT ( 'NONE',  ( 11.55000000000000071, 0.000000000000000000, 4.999999999999998224 ) ) ;
#41435 = CARTESIAN_POINT ( 'NONE',  ( 7.725000001229034297, -5.773502691896255534, -1.060575238724906372E-15 ) ) ;
#41436 = CARTESIAN_POINT ( 'NONE',  ( 7.715625000614515727, 3.027376345333611329, 5.243569643749999010 ) ) ;
#41437 = CARTESIAN_POINT ( 'NONE',  ( 22.16250000000000142, 2.886751345948129099, -4.999999999999998224 ) ) ;
#41438 = CARTESIAN_POINT ( 'NONE',  ( 21.10312500061451502, 4.541064518000418104, -2.621784821874998173 ) ) ;
#41439 = CARTESIAN_POINT ( 'NONE',  ( 4.711411573247316298, 1.674097066322985938, -4.711411573247316298 ) ) ;
#41440 = CARTESIAN_POINT ( 'NONE',  ( 25.42500000122903359, 2.886751345948129099, -4.999999999999998224 ) ) ;
#41441 = CARTESIAN_POINT ( 'NONE',  ( -3.756430356249999214, 19.12812499938548427, 27.83122392262697176 ) ) ;
#41442 = CARTESIAN_POINT ( 'NONE',  ( 5.625000000000001776, 4.330127018922191873, 2.499999999999999556 ) ) ;
#41443 = ORIENTED_EDGE ( 'NONE', *, *, #7791, .T. ) ;
#41444 = CARTESIAN_POINT ( 'NONE',  ( 19.67812500061451786, 6.421520780324663323E-16, -5.243569643749999010 ) ) ;
#41445 = CARTESIAN_POINT ( 'NONE',  ( 27.40312500061451573, 4.541064518000418104, -2.621784821874998173 ) ) ;
#41446 = CARTESIAN_POINT ( 'NONE',  ( 26.93437500061451573, 6.421520780324663323E-16, -5.243569643749999010 ) ) ;
#41447 = CARTESIAN_POINT ( 'NONE',  ( 13.71562500061451750, -6.054752690667223547, -1.112240025338166033E-15 ) ) ;
#41448 = CARTESIAN_POINT ( 'NONE',  ( 11.32500000000000107, 6.123233995736764310E-16, -4.999999999999998224 ) ) ;
#41449 = CARTESIAN_POINT ( 'NONE',  ( 25.98750000122903003, 4.330127018922191873, 2.499999999999999556 ) ) ;
#41450 = CARTESIAN_POINT ( 'NONE',  ( 19.47187500061451360, 2.746126346562643317, 4.756430356249998326 ) ) ;
#41451 = CARTESIAN_POINT ( 'NONE',  ( 17.72812500061451502, -4.541064518000419881, 2.621784821874995952 ) ) ;
#41452 = DIRECTION ( 'NONE',  ( -1.000000000000000000, -0.000000000000000000, -0.000000000000000000 ) ) ;
#41453 = CARTESIAN_POINT ( 'NONE',  ( 28.92187500061451644, 3.027376345333611329, 5.243569643749999010 ) ) ;
#41454 = CARTESIAN_POINT ( 'NONE',  ( 10.20937500061451786, -4.541064518000417216, -2.621784821875001281 ) ) ;
#41455 = CARTESIAN_POINT ( 'NONE',  ( 8.484375000614518214, 6.421520780324663323E-16, -5.243569643749999010 ) ) ;
#41456 = CARTESIAN_POINT ( 'NONE',  ( 18.30937500061451928, -4.541064518000417216, -2.621784821875001281 ) ) ;
#41457 = ORIENTED_EDGE ( 'NONE', *, *, #14874, .T. ) ;
#41458 = CARTESIAN_POINT ( 'NONE',  ( 24.26250000122903216, 0.000000000000000000, 4.999999999999998224 ) ) ;
#41459 = CARTESIAN_POINT ( 'NONE',  ( 21.81562500061451004, -6.054752690667223547, -1.112240025338166033E-15 ) ) ;
#41460 = CARTESIAN_POINT ( 'NONE',  ( 19.35937500061451644, 4.541064518000418104, -2.621784821874998173 ) ) ;
#41461 = CARTESIAN_POINT ( 'NONE',  ( 22.45312500061451644, 4.541064518000418104, -2.621784821874998173 ) ) ;
#41462 = CARTESIAN_POINT ( 'NONE',  ( 3.999999999999998668, 13.96250000000000213, 27.69059892324149175 ) ) ;
#41463 = CARTESIAN_POINT ( 'NONE',  ( 3.571875000614517237, 3.027376345333613106, -5.243569643749998122 ) ) ;
#41464 = CARTESIAN_POINT ( 'NONE',  ( 9.975000001229034297, -5.773502691896255534, -1.060575238724906372E-15 ) ) ;
#41465 = ORIENTED_EDGE ( 'NONE', *, *, #61270, .F. ) ;
#41466 = CARTESIAN_POINT ( 'NONE',  ( 4.312500001229034652, 4.330127018922192761, -2.499999999999997780 ) ) ;
#41467 = CARTESIAN_POINT ( 'NONE',  ( 28.49999999999999645, 4.330127018922192761, -2.499999999999997780 ) ) ;
#41468 = CARTESIAN_POINT ( 'NONE',  ( 24.82500000122902861, -5.773502691896255534, -1.060575238724906372E-15 ) ) ;
#41469 = CARTESIAN_POINT ( 'NONE',  ( -0.7391736788420463222, 20.86739049229268161, 34.19204003105966905 ) ) ;
#41470 = CARTESIAN_POINT ( 'NONE',  ( 9.984375000614518214, 4.541064518000418104, 2.621784821874999949 ) ) ;
#41471 = CARTESIAN_POINT ( 'NONE',  ( 45.00000000000000000, 0.000000000000000000, 0.000000000000000000 ) ) ;
#41472 = CARTESIAN_POINT ( 'NONE',  ( 15.74062500061451608, 6.054752690667223547, 3.707466751127219781E-16 ) ) ;
#41473 = CARTESIAN_POINT ( 'NONE',  ( 10.32187500061451679, 3.027376345333613106, -5.243569643749998122 ) ) ;
#41474 = CARTESIAN_POINT ( 'NONE',  ( 29.32500000122903216, -5.773502691896255534, -1.060575238724906372E-15 ) ) ;
#41475 = CARTESIAN_POINT ( 'NONE',  ( 20.44687500061451857, -3.027376345333614438, 5.243569643749998122 ) ) ;
#41476 = CARTESIAN_POINT ( 'NONE',  ( 7.021875000614518747, -6.054752690667223547, -1.112240025338166033E-15 ) ) ;
#41477 = CARTESIAN_POINT ( 'NONE',  ( 1.999999999999998668, 16.36250000122903359, 26.53589838486224650 ) ) ;
#41478 =( BOUNDED_CURVE ( )  B_SPLINE_CURVE ( 2, ( #9394, #38187, #49288, #72181, #66641, #65536, #43007, #60712, #20827 ),
 .UNSPECIFIED., .F., .F. ) 
 B_SPLINE_CURVE_WITH_KNOTS ( ( 3, 2, 2, 2, 3 ),
 ( 0.3194444444444444753, 0.3240740740740740700, 0.3333333333333333148, 0.3425925925925926152, 0.3472222222222222654 ),
 .UNSPECIFIED. ) 
 CURVE ( )  GEOMETRIC_REPRESENTATION_ITEM ( )  RATIONAL_B_SPLINE_CURVE ( ( 0.9330127018922194093, 0.9330127018922197424, 1.000000000000000000, 0.8660254037844387076, 1.000000000000000000, 0.8660254037844387076, 1.000000000000000000, 0.9330127018922189652, 0.9330127018922194093 ) ) 
 REPRESENTATION_ITEM ( '' )  );
#41479 = CARTESIAN_POINT ( 'NONE',  ( 7.828125000614517326, -4.541064518000419881, 2.621784821874995952 ) ) ;
#41480 = CARTESIAN_POINT ( 'NONE',  ( 17.54062500061451502, 6.054752690667223547, 3.707466751127219781E-16 ) ) ;
#41481 = ORIENTED_EDGE ( 'NONE', *, *, #55095, .T. ) ;
#41482 = CARTESIAN_POINT ( 'NONE',  ( 15.81562500061451537, 3.027376345333611329, 5.243569643749999010 ) ) ;
#41483 = CARTESIAN_POINT ( 'NONE',  ( 11.42812500061451608, -4.541064518000419881, 2.621784821874995952 ) ) ;
#41484 = CARTESIAN_POINT ( 'NONE',  ( 24.38437500061451502, 4.119189519843966529, 2.378215178124999607 ) ) ;
#41485 = CARTESIAN_POINT ( 'NONE',  ( 11.70000000000000284, -4.330127018922190985, -2.500000000000001332 ) ) ;
#41486 = CARTESIAN_POINT ( 'NONE',  ( 6.600000001229032520, 5.773502691896255534, 3.535250795749688894E-16 ) ) ;
#41487 = EDGE_CURVE ( 'NONE', #57422, #60454, #53065, .T. ) ;
#41488 = CARTESIAN_POINT ( 'NONE',  ( 14.07187500061451679, 3.027376345333611329, 5.243569643749999010 ) ) ;
#41489 = CARTESIAN_POINT ( 'NONE',  ( 17.25000000122903288, -2.886751345948125991, -5.000000000000000000 ) ) ;
#41490 = CARTESIAN_POINT ( 'NONE',  ( 24.63749999999999574, -2.886751345948129988, 4.999999999999997335 ) ) ;
#41491 = CARTESIAN_POINT ( 'NONE',  ( -4.243569643749997233, 18.49062500061451431, -27.54997392385601174 ) ) ;
#41492 = CARTESIAN_POINT ( 'NONE',  ( 16.38750000122903216, 6.123233995736764310E-16, -4.999999999999998224 ) ) ;
#41493 = CARTESIAN_POINT ( 'NONE',  ( 1.071796769724491893, 10.79509619066136850, -26.00000000000000355 ) ) ;
#41494 = CARTESIAN_POINT ( 'NONE',  ( 3.965171583692859603, 3.045884815923804556, 3.965171583692790325 ) ) ;
#41495 = CARTESIAN_POINT ( 'NONE',  ( 17.25937500061451502, 0.000000000000000000, 5.243569643749999010 ) ) ;
#41496 = PRODUCT_DEFINITION_FORMATION_WITH_SPECIFIED_SOURCE ( 'ANY', '', #9598, .NOT_KNOWN. ) ;
#41497 = CARTESIAN_POINT ( 'NONE',  ( 29.81250000000000000, 2.886751345948129099, -4.999999999999998224 ) ) ;
#41498 = CARTESIAN_POINT ( 'NONE',  ( 13.34062500061451750, -3.027376345333610441, -5.243569643749999898 ) ) ;
#41499 = CARTESIAN_POINT ( 'NONE',  ( 10.59375000122903465, 5.773502691896255534, 3.535250795749688894E-16 ) ) ;
#41500 = CARTESIAN_POINT ( 'NONE',  ( 5.000000000000000000, 39.99999999999999289, 30.00000000000000000 ) ) ;
#41501 = CARTESIAN_POINT ( 'NONE',  ( 23.44687500061451502, 6.054752690667223547, 3.707466751127219781E-16 ) ) ;
#41502 = CARTESIAN_POINT ( 'NONE',  ( 15.23437500061451644, 5.492252693125287522, 3.363034840372157021E-16 ) ) ;
#41503 = CARTESIAN_POINT ( 'NONE',  ( 9.328125000614518214, 6.421520780324663323E-16, -5.243569643749999010 ) ) ;
#41504 = CARTESIAN_POINT ( 'NONE',  ( 15.00937500061451679, 0.000000000000000000, 5.243569643749999010 ) ) ;
#41505 = VERTEX_POINT ( 'NONE', #59319 ) ;
#41506 = CARTESIAN_POINT ( 'NONE',  ( 26.22187500061451715, 3.027376345333611329, 5.243569643749999010 ) ) ;
#41507 = CARTESIAN_POINT ( 'NONE',  ( 27.96562500061451928, 3.027376345333611329, 5.243569643749999010 ) ) ;
#41508 = CARTESIAN_POINT ( 'NONE',  ( 18.14062500061451644, -3.027376345333614438, 5.243569643749998122 ) ) ;
#41509 = DIRECTION ( 'NONE',  ( -1.000000000000000000, -0.000000000000000000, -0.000000000000000000 ) ) ;
#41510 = CARTESIAN_POINT ( 'NONE',  ( -3.137519842735245283E-14, 12.57500000122903572, -26.00000000000000711 ) ) ;
#41511 =( BOUNDED_CURVE ( )  B_SPLINE_CURVE ( 3, ( #10341, #4449, #15141, #50241 ),
 .UNSPECIFIED., .F., .F. ) 
 B_SPLINE_CURVE_WITH_KNOTS ( ( 4, 4 ),
 ( 2.315884994543730091, 2.347585424998526182 ),
 .UNSPECIFIED. ) 
 CURVE ( )  GEOMETRIC_REPRESENTATION_ITEM ( )  RATIONAL_B_SPLINE_CURVE ( ( 1.000000000000000000, 0.9999162586456273871, 0.9999162586456273871, 1.000000000000000000 ) ) 
 REPRESENTATION_ITEM ( '' )  );
#41512 = CARTESIAN_POINT ( 'NONE',  ( 8.775000000000002132, 4.330127018922191873, 2.499999999999999556 ) ) ;
#41513 = CARTESIAN_POINT ( 'NONE',  ( 19.23750000122903714, 4.330127018922191873, 2.499999999999999556 ) ) ;
#41514 = DIRECTION ( 'NONE',  ( -1.000000000000000000, 0.000000000000000000, 0.000000000000000000 ) ) ;
#41515 = CARTESIAN_POINT ( 'NONE',  ( 10.32187500061451679, 4.119189519843966529, 2.378215178124999607 ) ) ;
#41516 = ORIENTED_EDGE ( 'NONE', *, *, #48583, .T. ) ;
#41517 = CARTESIAN_POINT ( 'NONE',  ( 17.02499999999999858, -4.330127018922194537, 2.499999999999995559 ) ) ;
#41518 = CARTESIAN_POINT ( 'NONE',  ( 22.31250000000000000, 2.886751345948126879, 4.999999999999999112 ) ) ;
#41519 = CARTESIAN_POINT ( 'NONE',  ( 17.97187500061451715, 3.027376345333613106, -5.243569643749998122 ) ) ;
#41520 = CARTESIAN_POINT ( 'NONE',  ( 14.84062500061451750, 6.054752690667223547, 3.707466751127219781E-16 ) ) ;
#41521 = ORIENTED_EDGE ( 'NONE', *, *, #27951, .T. ) ;
#41522 = LINE ( 'NONE', #30437, #24209 ) ;
#41523 = CARTESIAN_POINT ( 'NONE',  ( 6.853125000614516793, 0.000000000000000000, 5.243569643749999010 ) ) ;
#41524 = CARTESIAN_POINT ( 'NONE',  ( 8.943750001229032520, -2.886751345948074920, 5.000000000000092371 ) ) ;
#41525 = CARTESIAN_POINT ( 'NONE',  ( 12.86250000000000071, 2.886751345948126879, 4.999999999999999112 ) ) ;
#41526 = CARTESIAN_POINT ( 'NONE',  ( 27.79687500061451289, 4.119189519843966529, -2.378215178124998275 ) ) ;
#41527 = CARTESIAN_POINT ( 'NONE',  ( -2.121784821874996840, 14.47812500061451679, 33.67503911421598417 ) ) ;
#41528 = CARTESIAN_POINT ( 'NONE',  ( 28.04062500061451502, -3.027376345333614438, 5.243569643749998122 ) ) ;
#41529 = CARTESIAN_POINT ( 'NONE',  ( 8.512499999999999289, -5.773502691896255534, -1.060575238724906372E-15 ) ) ;
#41530 = CARTESIAN_POINT ( 'NONE',  ( -1.878215178125001827, 17.89062499938548356, 33.25316411605952283 ) ) ;
#41531 = CARTESIAN_POINT ( 'NONE',  ( 23.74687500061451573, -3.027376345333610441, -5.243569643749999898 ) ) ;
#41532 = ORIENTED_EDGE ( 'NONE', *, *, #27801, .F. ) ;
#41533 = CARTESIAN_POINT ( 'NONE',  ( 21.92812500061451431, 6.421520780324663323E-16, -5.243569643749999010 ) ) ;
#41534 = CARTESIAN_POINT ( 'NONE',  ( 23.52187500061451786, 3.027376345333611329, 5.243569643749999010 ) ) ;
#41535 = EDGE_CURVE ( 'NONE', #45117, #67338, #8729, .T. ) ;
#41536 = CARTESIAN_POINT ( 'NONE',  ( 4.243569643749999898, 16.39062500061459460, -27.54997392385601529 ) ) ;
#41537 = CARTESIAN_POINT ( 'NONE',  ( 7.453125000614516438, -4.541064518000417216, -2.621784821875001281 ) ) ;
#41538 = CARTESIAN_POINT ( 'NONE',  ( 26.44687500061451502, -2.746126346562641984, -4.756430356249999214 ) ) ;
#41539 = CARTESIAN_POINT ( 'NONE',  ( 24.59062500061451573, -3.027376345333610441, -5.243569643749999898 ) ) ;
#41540 = CARTESIAN_POINT ( 'NONE',  ( 27.30937500061451217, 2.746126346562645981, -4.756430356249997438 ) ) ;
#41541 = CARTESIAN_POINT ( 'NONE',  ( 10.05937500061451750, 0.000000000000000000, 4.756430356249998326 ) ) ;
#41542 = CARTESIAN_POINT ( 'NONE',  ( 16.35937500061451644, 0.000000000000000000, 5.243569643749999010 ) ) ;
#41543 = CARTESIAN_POINT ( 'NONE',  ( 27.75937500061451502, -4.541064518000417216, -2.621784821875001281 ) ) ;
#41544 = CARTESIAN_POINT ( 'NONE',  ( -2.121784821874996840, 14.53437500061451715, 33.67503911421598417 ) ) ;
#41545 = CARTESIAN_POINT ( 'NONE',  ( 8.240625000614516082, -3.027376345333614438, 5.243569643749998122 ) ) ;
#41546 = CARTESIAN_POINT ( 'NONE',  ( 4.000000000000000000, 10.40000000122903323, -27.69059892324149885 ) ) ;
#41547 =( BOUNDED_CURVE ( )  B_SPLINE_CURVE ( 2, ( #23679, #40688, #44794, #56581, #34405, #68400, #57659, #35134, #68765 ),
 .UNSPECIFIED., .F., .F. ) 
 B_SPLINE_CURVE_WITH_KNOTS ( ( 3, 2, 2, 2, 3 ),
 ( 0.04166666666666667129, 0.04629629629629629373, 0.05555555555555555247, 0.06481481481481481122, 0.06944444444444444753 ),
 .UNSPECIFIED. ) 
 CURVE ( )  GEOMETRIC_REPRESENTATION_ITEM ( )  RATIONAL_B_SPLINE_CURVE ( ( 0.9330127018922192983, 0.9330127018922194093, 1.000000000000000000, 0.8660254037844387076, 1.000000000000000000, 0.8660254037844387076, 1.000000000000000000, 0.9330127018922191873, 0.9330127018922192983 ) ) 
 REPRESENTATION_ITEM ( '' )  );
#41548 = CARTESIAN_POINT ( 'NONE',  ( 4.134375000614517681, 4.541064518000418104, 2.621784821874999949 ) ) ;
#41549 = CARTESIAN_POINT ( 'NONE',  ( 4.000000000000000000, 17.48750000000000071, 27.69059892324149885 ) ) ;
#41550 = CARTESIAN_POINT ( 'NONE',  ( 5.278125000614516615, 6.421520780324663323E-16, -5.243569643749999010 ) ) ;
#41551 = CARTESIAN_POINT ( 'NONE',  ( 9.159375000614515372, 0.000000000000000000, 5.243569643749999010 ) ) ;
#41552 = CARTESIAN_POINT ( 'NONE',  ( 16.05000000122903359, 5.773502691896255534, 3.535250795749688894E-16 ) ) ;
#41553 = CARTESIAN_POINT ( 'NONE',  ( 29.76562500061451644, 3.027376345333611329, 5.243569643749999010 ) ) ;
#41554 = CARTESIAN_POINT ( 'NONE',  ( 7.190625000614518036, 6.054752690667223547, 3.707466751127219781E-16 ) ) ;
#41555 = CARTESIAN_POINT ( 'NONE',  ( -4.000000000000000888, 14.05624999877096570, 32.30940107675850470 ) ) ;
#41556 = CARTESIAN_POINT ( 'NONE',  ( 20.71875000122903288, -5.773502691896255534, -1.060575238724906372E-15 ) ) ;
#41557 = CARTESIAN_POINT ( 'NONE',  ( 16.62187500061451573, 3.027376345333613106, -5.243569643749998122 ) ) ;
#41558 = ORIENTED_EDGE ( 'NONE', *, *, #12308, .T. ) ;
#41559 = CARTESIAN_POINT ( 'NONE',  ( 25.00312500061451715, -4.541064518000417216, -2.621784821875001281 ) ) ;
#41560 = CARTESIAN_POINT ( 'NONE',  ( 10.41562500061451679, 3.027376345333611329, 5.243569643749999010 ) ) ;
#41561 = CARTESIAN_POINT ( 'NONE',  ( 26.07187500061451502, 3.027376345333612662, -5.243569643749998122 ) ) ;
#41562 = CARTESIAN_POINT ( 'NONE',  ( 8.990625000614516082, 6.054752690667223547, 3.707466751127219781E-16 ) ) ;
#41563 = CARTESIAN_POINT ( 'NONE',  ( 0.000000000000000000, 20.00000000000000000, 30.00000000000000000 ) ) ;
#41564 = CARTESIAN_POINT ( 'NONE',  ( 10.80000000122903536, -2.886751345948129988, 4.999999999999997335 ) ) ;
#41565 = CARTESIAN_POINT ( 'NONE',  ( 23.91562500061451502, 3.027376345333611329, 5.243569643749999010 ) ) ;
#41566 = VECTOR ( 'NONE', #71753, 1000.000000000000000 ) ;
#41567 = CARTESIAN_POINT ( 'NONE',  ( -4.243569643749999898, 11.21562500061451750, -32.45002607614398471 ) ) ;
#41568 = CARTESIAN_POINT ( 'NONE',  ( 12.48750000122903359, 4.330127018922191873, 2.499999999999999556 ) ) ;
#41569 = CARTESIAN_POINT ( 'NONE',  ( 21.92812500061451431, 6.421520780324663323E-16, -5.243569643749999010 ) ) ;
#41570 = CARTESIAN_POINT ( 'NONE',  ( 17.72812500061451502, -4.541064518000419881, 2.621784821874995952 ) ) ;
#41571 = CARTESIAN_POINT ( 'NONE',  ( 4.897546610576117843, 1.006994139586731674, -5.145967878999484491 ) ) ;
#41572 = CARTESIAN_POINT ( 'NONE',  ( 18.30000000000000071, 0.000000000000000000, 4.999999999999998224 ) ) ;
#41573 = CARTESIAN_POINT ( 'NONE',  ( 13.27500000122903323, 2.886751345948129099, -4.999999999999998224 ) ) ;
#41574 = CARTESIAN_POINT ( 'NONE',  ( 10.64062500061451644, -3.027376345333610441, -5.243569643749999898 ) ) ;
#41575 = EDGE_CURVE ( 'NONE', #34387, #7528, #58957, .T. ) ;
#41576 = CARTESIAN_POINT ( 'NONE',  ( 13.97812500061451679, 4.541064518000418104, 2.621784821874999949 ) ) ;
#41577 = CARTESIAN_POINT ( 'NONE',  ( 26.73750000122903003, 6.123233995736764310E-16, -4.999999999999998224 ) ) ;
#41578 = CARTESIAN_POINT ( 'NONE',  ( 21.19687500061451502, 6.054752690667223547, 3.707466751127219781E-16 ) ) ;
#41579 = CARTESIAN_POINT ( 'NONE',  ( 22.05937500061451573, 4.541064518000418104, -2.621784821874998173 ) ) ;
#41580 = CARTESIAN_POINT ( 'NONE',  ( 5.810221930991193690E-16, 13.96249999999999858, 26.00000000000000000 ) ) ;
#41581 = CARTESIAN_POINT ( 'NONE',  ( 7.987500001229032698, 4.330127018922191873, 2.499999999999999556 ) ) ;
#41582 = CARTESIAN_POINT ( 'NONE',  ( 5.521875000614517859, 3.027376345333611329, 5.243569643749999010 ) ) ;
#41583 = CARTESIAN_POINT ( 'NONE',  ( 25.73437500061451644, 4.541064518000418104, 2.621784821874999949 ) ) ;
#41584 = CARTESIAN_POINT ( 'NONE',  ( 15.26250000122903216, 0.000000000000000000, 4.999999999999998224 ) ) ;
#41585 = CARTESIAN_POINT ( 'NONE',  ( 21.02812500061451573, 6.421520780324663323E-16, -5.243569643749999010 ) ) ;
#41586 = CARTESIAN_POINT ( 'NONE',  ( 26.55937500061451573, 4.541064518000418104, -2.621784821874998173 ) ) ;
#41587 = CARTESIAN_POINT ( 'NONE',  ( 3.756430356250000102, 17.70312499938548356, 30.00000000000000000 ) ) ;
#41588 = CARTESIAN_POINT ( 'NONE',  ( 19.44375000122903430, -2.886751345948126435, -5.000000000000000000 ) ) ;
#41589 = CARTESIAN_POINT ( 'NONE',  ( 20.78732959644809952, 4.500000000000001776, 5.500000000000000000 ) ) ;
#41590 = CARTESIAN_POINT ( 'NONE',  ( 7.659375000614518036, 4.541064518000418104, -2.621784821874998173 ) ) ;
#41591 = CARTESIAN_POINT ( 'NONE',  ( 18.06562500061451715, 3.027376345333611329, 5.243569643749999010 ) ) ;
#41592 = VERTEX_POINT ( 'NONE', #3199 ) ;
#41593 = DIRECTION ( 'NONE',  ( 0.000000000000000000, 0.000000000000000000, 1.000000000000000000 ) ) ;
#41594 = CARTESIAN_POINT ( 'NONE',  ( 26.54062500061451146, 6.054752690667223547, 3.707466751127219781E-16 ) ) ;
#41595 = CARTESIAN_POINT ( 'NONE',  ( 3.946875000614517681, -3.027376345333610441, -5.243569643749999898 ) ) ;
#41596 = CARTESIAN_POINT ( 'NONE',  ( -2.000000000000000000, 15.87500000000000000, -33.46410161513775705 ) ) ;
#41597 = LINE ( 'NONE', #29782, #33560 ) ;
#41598 = CARTESIAN_POINT ( 'NONE',  ( 17.06250000000000000, -5.773502691896255534, -1.060575238724906372E-15 ) ) ;
#41599 = CARTESIAN_POINT ( 'NONE',  ( 20.35312500061451502, 0.000000000000000000, 5.243569643749999010 ) ) ;
#41600 = ORIENTED_EDGE ( 'NONE', *, *, #36421, .T. ) ;
#41601 = CARTESIAN_POINT ( 'NONE',  ( 24.33749999999999858, -2.886751345948125991, -5.000000000000000000 ) ) ;
#41602 = CARTESIAN_POINT ( 'NONE',  ( 25.47187500061451715, -6.054752690667223547, -1.112240025338166033E-15 ) ) ;
#41603 = VERTEX_POINT ( 'NONE', #65239 ) ;
#41604 = VECTOR ( 'NONE', #25933, 1000.000000000000000 ) ;
#41605 = CARTESIAN_POINT ( 'NONE',  ( 12.55312500061451786, 4.541064518000418104, -2.621784821874998173 ) ) ;
#41606 = CARTESIAN_POINT ( 'NONE',  ( 5.390625000614518214, 6.054752690667223547, 3.707466751127219781E-16 ) ) ;
#41607 = CARTESIAN_POINT ( 'NONE',  ( 15.87187500061451573, -4.119189519843968306, 2.378215178124996054 ) ) ;
#41608 = CARTESIAN_POINT ( 'NONE',  ( 29.27812500061451573, 4.541064518000418104, 2.621784821874999949 ) ) ;
#41609 = CARTESIAN_POINT ( 'NONE',  ( 15.86250000122903181, -4.330127018922190985, -2.500000000000001332 ) ) ;
#41610 = CARTESIAN_POINT ( 'NONE',  ( 19.50000000000000000, 4.330127018922192761, -2.499999999999997780 ) ) ;
#41611 = CARTESIAN_POINT ( 'NONE',  ( 25.64999999999999858, -4.330127018922190985, -2.500000000000001332 ) ) ;
#41612 = CARTESIAN_POINT ( 'NONE',  ( 1.071796769724491893, 10.68259618943233313, -26.00000000000000355 ) ) ;
#41613 = CARTESIAN_POINT ( 'NONE',  ( 9.909375000614517148, 4.541064518000418104, -2.621784821874998173 ) ) ;
#41614 = CARTESIAN_POINT ( 'NONE',  ( 18.98437500061451644, 4.541064518000418104, 2.621784821874999949 ) ) ;
#41615 = CARTESIAN_POINT ( 'NONE',  ( 25.94999999999999929, 0.000000000000000000, 4.999999999999998224 ) ) ;
#41616 = ORIENTED_EDGE ( 'NONE', *, *, #18934, .F. ) ;
#41617 = CARTESIAN_POINT ( 'NONE',  ( 28.64062500061451289, -3.027376345333610441, -5.243569643749999898 ) ) ;
#41618 = CARTESIAN_POINT ( 'NONE',  ( 29.07187500061451502, -6.054752690667223547, -1.112240025338166033E-15 ) ) ;
#41619 = CARTESIAN_POINT ( 'NONE',  ( 5.784375000614517148, 6.421520780324663323E-16, -5.243569643749999010 ) ) ;
#41620 = CARTESIAN_POINT ( 'NONE',  ( 16.61250000000000426, -5.773502691896255534, -1.060575238724906372E-15 ) ) ;
#41621 = CARTESIAN_POINT ( 'NONE',  ( 13.86562500061451431, 3.027376345333613106, -5.243569643749998122 ) ) ;
#41622 = CARTESIAN_POINT ( 'NONE',  ( 3.999999999999998668, 18.76250000000000284, 32.30940107675850470 ) ) ;
#41623 = CYLINDRICAL_SURFACE ( 'NONE', #56384, 4.999999999999998224 ) ;
#41624 = CARTESIAN_POINT ( 'NONE',  ( 18.71250000122903145, 4.330127018922192761, -2.499999999999997780 ) ) ;
#41625 = CARTESIAN_POINT ( 'NONE',  ( 18.12187500061451573, 2.746126346562643317, 4.756430356249998326 ) ) ;
#41626 = CARTESIAN_POINT ( 'NONE',  ( 8.540625000614518569, 6.054752690667223547, 3.707466751127219781E-16 ) ) ;
#41627 = CARTESIAN_POINT ( 'NONE',  ( 24.30937500061451573, 4.541064518000418104, -2.621784821874998173 ) ) ;
#41628 = CARTESIAN_POINT ( 'NONE',  ( 27.03750000122903430, -4.330127018922194537, 2.499999999999995559 ) ) ;
#41629 = EDGE_CURVE ( 'NONE', #58973, #54880, #14628, .T. ) ;
#41630 = CARTESIAN_POINT ( 'NONE',  ( 23.48437500061451644, 4.541064518000418104, 2.621784821874999949 ) ) ;
#41631 = CARTESIAN_POINT ( 'NONE',  ( 6.937499999999999112, 5.773502691896255534, 3.535250795749688894E-16 ) ) ;
#41632 = CARTESIAN_POINT ( 'NONE',  ( -3.999999999999997335, 12.95000000122903572, 32.30940107675850470 ) ) ;
#41633 = CARTESIAN_POINT ( 'NONE',  ( 15.10312500061451502, -4.541064518000417216, -2.621784821875001281 ) ) ;
#41634 = CARTESIAN_POINT ( 'NONE',  ( 7.612500001229035362, 0.000000000000000000, 4.999999999999998224 ) ) ;
#41635 = CARTESIAN_POINT ( 'NONE',  ( 10.88437500061451679, 4.541064518000418104, 2.621784821874999949 ) ) ;
#41636 = DIRECTION ( 'NONE',  ( -1.000000000000000000, -0.000000000000000000, -0.000000000000000000 ) ) ;
#41637 = ORIENTED_EDGE ( 'NONE', *, *, #26513, .F. ) ;
#41638 = CARTESIAN_POINT ( 'NONE',  ( 13.45312500061451466, 4.541064518000418104, -2.621784821874998173 ) ) ;
#41639 = CARTESIAN_POINT ( 'NONE',  ( 2.000000000000000444, 19.71874999877096712, 26.53589838486224650 ) ) ;
#41640 = CARTESIAN_POINT ( 'NONE',  ( 22.91250000122903430, 0.000000000000000000, 4.999999999999998224 ) ) ;
#41641 = CARTESIAN_POINT ( 'NONE',  ( 12.08437500061451608, 6.421520780324663323E-16, -5.243569643749999010 ) ) ;
#41642 = CARTESIAN_POINT ( 'NONE',  ( 14.50312500061451537, 0.000000000000000000, 5.243569643749999010 ) ) ;
#41643 = CARTESIAN_POINT ( 'NONE',  ( 27.50625000122903074, -4.330127018922190985, -2.500000000000001332 ) ) ;
#41644 = CARTESIAN_POINT ( 'NONE',  ( 23.37187500061451573, 3.027376345333613106, -5.243569643749998122 ) ) ;
#41645 = CYLINDRICAL_SURFACE ( 'NONE', #43144, 4.999999999999998224 ) ;
#41646 = CARTESIAN_POINT ( 'NONE',  ( 23.77499999999999858, -4.330127018922194537, 2.499999999999995559 ) ) ;
#41647 = CARTESIAN_POINT ( 'NONE',  ( 14.92500000000000071, 6.123233995736764310E-16, -4.999999999999998224 ) ) ;
#41648 = CARTESIAN_POINT ( 'NONE',  ( -4.243569643749999898, 15.35937500061451644, -30.00000000000000000 ) ) ;
#41649 = CARTESIAN_POINT ( 'NONE',  ( 16.39687500061451786, -3.027376345333614438, 5.243569643749998122 ) ) ;
#41650 = CARTESIAN_POINT ( 'NONE',  ( 17.02500000122903145, 2.886751345948126879, 4.999999999999999112 ) ) ;
#41651 = CARTESIAN_POINT ( 'NONE',  ( 13.09687500061451892, 6.054752690667223547, 3.707466751127219781E-16 ) ) ;
#41652 = CARTESIAN_POINT ( 'NONE',  ( 4.243569643749999898, 11.04687500061451999, 32.45002607614398471 ) ) ;
#41653 = CARTESIAN_POINT ( 'NONE',  ( 19.12500000122903288, 2.886751345948129099, -4.999999999999998224 ) ) ;
#41654 = CARTESIAN_POINT ( 'NONE',  ( 12.85312500061451502, -4.541064518000417216, -2.621784821875001281 ) ) ;
#41655 = ORIENTED_EDGE ( 'NONE', *, *, #41965, .T. ) ;
#41656 = ORIENTED_EDGE ( 'NONE', *, *, #56762, .F. ) ;
#41657 = CARTESIAN_POINT ( 'NONE',  ( 17.02499999999999858, -4.330127018922194537, 2.499999999999995559 ) ) ;
#41658 = CARTESIAN_POINT ( 'NONE',  ( 9.999999999999992895, 5.857864376269048101, -9.999999999999992895 ) ) ;
#41659 = CARTESIAN_POINT ( 'NONE',  ( 11.70937500061451608, 4.541064518000418104, -2.621784821874998173 ) ) ;
#41660 = DIRECTION ( 'NONE',  ( 0.000000000000000000, 0.000000000000000000, -1.000000000000000000 ) ) ;
#41661 = CARTESIAN_POINT ( 'NONE',  ( 12.86250000122903359, 4.330127018922192761, -2.499999999999997780 ) ) ;
#41662 = CARTESIAN_POINT ( 'NONE',  ( 20.66250000122903074, 0.000000000000000000, 4.999999999999998224 ) ) ;
#41663 = CARTESIAN_POINT ( 'NONE',  ( 18.17812500061451786, -4.541064518000419881, 2.621784821874995952 ) ) ;
#41664 = CARTESIAN_POINT ( 'NONE',  ( 21.25312500061451715, 0.000000000000000000, 5.243569643749999010 ) ) ;
#41665 = CARTESIAN_POINT ( 'NONE',  ( 3.440625000614518036, -3.027376345333610441, -5.243569643749999898 ) ) ;
#41666 = ADVANCED_FACE ( 'NONE', ( #49729 ), #16817, .T. ) ;
#41667 = CARTESIAN_POINT ( 'NONE',  ( 26.88749999999999574, -2.886751345948129988, 4.999999999999997335 ) ) ;
#41668 = CARTESIAN_POINT ( 'NONE',  ( 7.546875000614517326, -2.746126346562642428, -4.756430356249999214 ) ) ;
#41669 = CARTESIAN_POINT ( 'NONE',  ( 28.09687500061451360, -3.027376345333614438, 5.243569643749998122 ) ) ;
#41670 = CARTESIAN_POINT ( 'NONE',  ( 13.01250000122903394, 0.000000000000000000, 4.999999999999998224 ) ) ;
#41671 = CARTESIAN_POINT ( 'NONE',  ( -2.121784821874999949, 16.63437500061451857, -33.67503911421598417 ) ) ;
#41672 = CARTESIAN_POINT ( 'NONE',  ( 4.875000001229034652, 2.886751345948126879, 4.999999999999999112 ) ) ;
#41673 = CARTESIAN_POINT ( 'NONE',  ( 6.262500000000000178, -5.773502691896255534, -1.060575238724906372E-15 ) ) ;
#41674 = CARTESIAN_POINT ( 'NONE',  ( 28.70625000122903003, 0.000000000000000000, 4.999999999999998224 ) ) ;
#41675 = CARTESIAN_POINT ( 'NONE',  ( 10.43437500061451750, 4.541064518000418104, 2.621784821874999949 ) ) ;
#41676 = CARTESIAN_POINT ( 'NONE',  ( 28.49062500061451431, -3.027376345333614438, 5.243569643749998122 ) ) ;
#41677 = CARTESIAN_POINT ( 'NONE',  ( 2.000000000000001332, 10.70000000000000107, 33.46410161513774995 ) ) ;
#41678 = CARTESIAN_POINT ( 'NONE',  ( -5.672756003115389412, 8.235591643417164320, -28.03551386504724618 ) ) ;
#41679 = CARTESIAN_POINT ( 'NONE',  ( 1.999999999999998668, 17.71250000122903501, -33.46410161513775705 ) ) ;
#41680 = CARTESIAN_POINT ( 'NONE',  ( 7.659375000614518036, 4.541064518000418104, -2.621784821874998173 ) ) ;
#41681 = CARTESIAN_POINT ( 'NONE',  ( 10.92187500061451644, 3.027376345333611329, 5.243569643749999010 ) ) ;
#41682 = CARTESIAN_POINT ( 'NONE',  ( 5.025000000000002132, 6.123233995736764310E-16, -4.999999999999998224 ) ) ;
#41683 = CARTESIAN_POINT ( 'NONE',  ( -2.121784821874996840, 14.02812500061459566, 33.67503911421598417 ) ) ;
#41684 = CARTESIAN_POINT ( 'NONE',  ( 4.987500000000004263, -2.886751345948059377, -5.000000000000114575 ) ) ;
#41685 = CARTESIAN_POINT ( 'NONE',  ( 6.750000000000002665, -4.330127018922190985, -2.500000000000001332 ) ) ;
#41686 = CARTESIAN_POINT ( 'NONE',  ( 14.93437500061451573, -2.746126346562646425, 4.756430356249996549 ) ) ;
#41687 = CARTESIAN_POINT ( 'NONE',  ( 20.31562500061451715, 3.027376345333611329, 5.243569643749999010 ) ) ;
#41688 = CARTESIAN_POINT ( 'NONE',  ( 13.97812500061451679, 4.541064518000418104, 2.621784821874999949 ) ) ;
#41689 = CARTESIAN_POINT ( 'NONE',  ( 22.77187500061451431, 5.824947211148865298E-16, -4.756430356249998326 ) ) ;
#41690 = CARTESIAN_POINT ( 'NONE',  ( 10.02187500061451964, 3.027376345333611329, 5.243569643749999010 ) ) ;
#41691 = CARTESIAN_POINT ( 'NONE',  ( 26.17500000000000071, 6.123233995736764310E-16, -4.999999999999998224 ) ) ;
#41692 = CARTESIAN_POINT ( 'NONE',  ( 23.51250000122903216, -4.330127018922190985, -2.500000000000001332 ) ) ;
#41693 = CARTESIAN_POINT ( 'NONE',  ( 11.25000000122903288, -2.886751345948130876, 4.999999999999996447 ) ) ;
#41694 = CARTESIAN_POINT ( 'NONE',  ( 10.92187500061451644, 3.027376345333611329, 5.243569643749999010 ) ) ;
#41695 = CARTESIAN_POINT ( 'NONE',  ( 25.54687500061451644, -3.027376345333610441, -5.243569643749999898 ) ) ;
#41696 = CARTESIAN_POINT ( 'NONE',  ( 4.021875000614516082, 3.027376345333613106, -5.243569643749998122 ) ) ;
#41697 = LINE ( 'NONE', #64221, #56090 ) ;
#41698 = CARTESIAN_POINT ( 'NONE',  ( 19.65937500061451360, -4.541064518000417216, -2.621784821875001281 ) ) ;
#41699 = CARTESIAN_POINT ( 'NONE',  ( 11.14687500061451608, -3.027376345333610441, -5.243569643749999898 ) ) ;
#41700 = CARTESIAN_POINT ( 'NONE',  ( 3.756430356249998770, 18.11562499938547788, 32.16877607737302469 ) ) ;
#41701 = CARTESIAN_POINT ( 'NONE',  ( 24.33749999999999858, -2.886751345948125991, -5.000000000000000000 ) ) ;
#41702 = CARTESIAN_POINT ( 'NONE',  ( 3.999999999999998668, 12.91249999999999964, 32.30940107675850470 ) ) ;
#41703 = CARTESIAN_POINT ( 'NONE',  ( -3.000416591977282496E-16, 11.64687500061451786, -34.90005215228797653 ) ) ;
#41704 = CARTESIAN_POINT ( 'NONE',  ( 24.04687500061451644, -2.746126346562646425, 4.756430356249996549 ) ) ;
#41705 = CARTESIAN_POINT ( 'NONE',  ( 16.00312500061451715, -4.541064518000417216, -2.621784821875001281 ) ) ;
#41706 = CARTESIAN_POINT ( 'NONE',  ( 4.237500000000001599, 5.773502691896255534, 3.535250795749688894E-16 ) ) ;
#41707 = CARTESIAN_POINT ( 'NONE',  ( -3.999999999999999112, 18.08749999999999858, 27.69059892324149530 ) ) ;
#41708 = CARTESIAN_POINT ( 'NONE',  ( 18.89999999999999858, -4.330127018922190985, -2.500000000000001332 ) ) ;
#41709 = CARTESIAN_POINT ( 'NONE',  ( 15.52500000000000036, 4.330127018922191873, 2.499999999999999556 ) ) ;
#41710 = CARTESIAN_POINT ( 'NONE',  ( -4.243569643749999898, 10.80312500061451786, 30.00000000000000000 ) ) ;
#41711 = CARTESIAN_POINT ( 'NONE',  ( 14.28750000122903430, 4.330127018922191873, 2.499999999999999556 ) ) ;
#41712 = CARTESIAN_POINT ( 'NONE',  ( 24.75937500061451502, 4.541064518000418104, -2.621784821874998173 ) ) ;
#41713 = DIRECTION ( 'NONE',  ( 0.000000000000000000, 0.000000000000000000, 1.000000000000000000 ) ) ;
#41714 = EDGE_LOOP ( 'NONE', ( #24879, #27626, #52871, #10906 ) ) ;
#41715 = CARTESIAN_POINT ( 'NONE',  ( 20.69062500061451715, 6.054752690667223547, 3.707466751127219781E-16 ) ) ;
#41716 = CARTESIAN_POINT ( 'NONE',  ( 3.478125000614517237, 6.421520780324663323E-16, -5.243569643749999010 ) ) ;
#41717 = CARTESIAN_POINT ( 'NONE',  ( 19.62187500061451573, -6.054752690667223547, -1.112240025338166033E-15 ) ) ;
#41718 = CARTESIAN_POINT ( 'NONE',  ( 28.99687500061451573, -3.027376345333614438, 5.243569643749998122 ) ) ;
#41719 = CARTESIAN_POINT ( 'NONE',  ( 7.265625000614516438, 3.027376345333611329, 5.243569643749999010 ) ) ;
#41720 = CARTESIAN_POINT ( 'NONE',  ( 21.40312500061451573, -4.541064518000417216, -2.621784821875001281 ) ) ;
#41721 = CARTESIAN_POINT ( 'NONE',  ( 4.243569643749999898, 15.07812500061451644, 30.00000000000000000 ) ) ;
#41722 = CARTESIAN_POINT ( 'NONE',  ( 18.41250000122903430, 0.000000000000000000, 4.999999999999998224 ) ) ;
#41723 = CARTESIAN_POINT ( 'NONE',  ( 13.47187500061451537, 2.746126346562645981, -4.756430356249997438 ) ) ;
#41724 = CARTESIAN_POINT ( 'NONE',  ( 9.365625000614519635, 3.027376345333612662, -5.243569643749998122 ) ) ;
#41725 = CARTESIAN_POINT ( 'NONE',  ( 13.76250000000000107, 2.886751345948126879, 4.999999999999998224 ) ) ;
#41726 = CARTESIAN_POINT ( 'NONE',  ( 3.309375000614518836, 0.000000000000000000, 5.243569643749999010 ) ) ;
#41727 = CARTESIAN_POINT ( 'NONE',  ( 23.37187500061451573, 3.027376345333613106, -5.243569643749998122 ) ) ;
#41728 = CARTESIAN_POINT ( 'NONE',  ( 14.54062500061451679, -3.027376345333614438, 5.243569643749998122 ) ) ;
#41729 = CARTESIAN_POINT ( 'NONE',  ( 24.90000000122903145, -2.886751345948125991, -5.000000000000000000 ) ) ;
#41730 = CARTESIAN_POINT ( 'NONE',  ( 26.27812500061451573, -4.541064518000419881, 2.621784821874995952 ) ) ;
#41731 = CARTESIAN_POINT ( 'NONE',  ( 20.44687500061451857, -3.027376345333614438, 5.243569643749998122 ) ) ;
#41732 = CARTESIAN_POINT ( 'NONE',  ( 15.02812500061451750, -4.541064518000419881, 2.621784821874995952 ) ) ;
#41733 = CARTESIAN_POINT ( 'NONE',  ( 2.121784821875001281, 15.95937500061451608, 33.67503911421598417 ) ) ;
#41734 = CARTESIAN_POINT ( 'NONE',  ( 19.22812500061451502, 6.421520780324663323E-16, -5.243569643749999010 ) ) ;
#41735 = CARTESIAN_POINT ( 'NONE',  ( 29.39062500061451289, -3.027376345333614438, 5.243569643749998122 ) ) ;
#41736 = VERTEX_POINT ( 'NONE', #37902 ) ;
#41737 = CARTESIAN_POINT ( 'NONE',  ( 24.37500000000000000, 6.123233995736764310E-16, -4.999999999999998224 ) ) ;
#41738 = CARTESIAN_POINT ( 'NONE',  ( -2.121784821874996840, 19.48437500061451644, -26.32496088578401583 ) ) ;
#41739 = CARTESIAN_POINT ( 'NONE',  ( -3.756430356249999214, 20.59062499938548640, 27.83122392262697531 ) ) ;
#41740 = CARTESIAN_POINT ( 'NONE',  ( 28.07812500061451289, -4.541064518000419881, 2.621784821874995952 ) ) ;
#41741 = CARTESIAN_POINT ( 'NONE',  ( 7.753125000614518036, 0.000000000000000000, 5.243569643749999010 ) ) ;
#41742 = CARTESIAN_POINT ( 'NONE',  ( 19.98750000122903359, 6.123233995736764310E-16, -4.999999999999998224 ) ) ;
#41743 = CARTESIAN_POINT ( 'NONE',  ( 25.22812500061451502, 4.541064518000418104, 2.621784821874999949 ) ) ;
#41744 = CARTESIAN_POINT ( 'NONE',  ( 25.68750000000000000, -2.886751345948125991, -5.000000000000000000 ) ) ;
#41745 = CARTESIAN_POINT ( 'NONE',  ( 4.000000000000000000, 16.25000000122903643, -27.69059892324149530 ) ) ;
#41746 = CARTESIAN_POINT ( 'NONE',  ( 28.19062500061451715, -3.027376345333610441, -5.243569643749999898 ) ) ;
#41747 = CARTESIAN_POINT ( 'NONE',  ( 10.34062500061451750, 6.054752690667223547, 3.707466751127219781E-16 ) ) ;
#41748 =( BOUNDED_CURVE ( )  B_SPLINE_CURVE ( 2, ( #47584, #63834, #19489, #36496, #13226, #29505, #41677, #19123, #30230 ),
 .UNSPECIFIED., .F., .F. ) 
 B_SPLINE_CURVE_WITH_KNOTS ( ( 3, 2, 2, 2, 3 ),
 ( 0.8804347826086956763, 0.8840579710144927938, 0.8913043478260869179, 0.8985507246376811530, 0.9021739130434782705 ),
 .UNSPECIFIED. ) 
 CURVE ( )  GEOMETRIC_REPRESENTATION_ITEM ( )  RATIONAL_B_SPLINE_CURVE ( ( 0.9330127018922194093, 0.9330127018922194093, 1.000000000000000000, 0.8660254037844387076, 1.000000000000000000, 0.8660254037844387076, 1.000000000000000000, 0.9330127018922194093, 0.9330127018922194093 ) ) 
 REPRESENTATION_ITEM ( '' )  );
#41749 = ORIENTED_EDGE ( 'NONE', *, *, #22231, .F. ) ;
#41750 = EDGE_CURVE ( 'NONE', #7096, #19771, #51024, .T. ) ;
#41751 = CARTESIAN_POINT ( 'NONE',  ( 24.70312500061451644, 4.541064518000418104, -2.621784821874998173 ) ) ;
#41752 = CARTESIAN_POINT ( 'NONE',  ( 4.678125000614516971, -4.541064518000419881, 2.621784821874995952 ) ) ;
#41753 = CARTESIAN_POINT ( 'NONE',  ( 13.54687500061451999, 5.492252693125287522, 3.363034840372157021E-16 ) ) ;
#41754 = DIRECTION ( 'NONE',  ( 0.000000000000000000, 0.000000000000000000, 1.000000000000000000 ) ) ;
#41755 = CARTESIAN_POINT ( 'NONE',  ( 12.33750000000000036, 5.773502691896255534, 3.535250795749688894E-16 ) ) ;
#41756 = CARTESIAN_POINT ( 'NONE',  ( 14.07187500061451679, 3.027376345333611329, 5.243569643749999010 ) ) ;
#41757 = CARTESIAN_POINT ( 'NONE',  ( 7.875000001229034652, 2.886751345948129099, -4.999999999999998224 ) ) ;
#41758 = CARTESIAN_POINT ( 'NONE',  ( 16.88437500061451502, -4.541064518000419881, 2.621784821874995952 ) ) ;
#41759 = CARTESIAN_POINT ( 'NONE',  ( 14.92500000000000071, 6.123233995736764310E-16, -4.999999999999998224 ) ) ;
#41760 = CARTESIAN_POINT ( 'NONE',  ( 8.634375000614518569, 4.541064518000418104, 2.621784821874999949 ) ) ;
#41761 = CARTESIAN_POINT ( 'NONE',  ( 4.243569643749999898, 12.34062500061451750, -27.54997392385601529 ) ) ;
#41762 = AXIS2_PLACEMENT_3D ( 'NONE', #32412, #9516, #54219 ) ;
#41763 = CARTESIAN_POINT ( 'NONE',  ( 20.92500000122903359, 2.886751345948129099, -4.999999999999997335 ) ) ;
#41764 = CARTESIAN_POINT ( 'NONE',  ( 22.17187500061451644, -4.119189519843968306, 2.378215178124996054 ) ) ;
#41765 = ORIENTED_EDGE ( 'NONE', *, *, #17437, .F. ) ;
#41766 = CARTESIAN_POINT ( 'NONE',  ( 25.64062500061451644, 6.054752690667223547, 3.707466751127219781E-16 ) ) ;
#41767 = CARTESIAN_POINT ( 'NONE',  ( 7.320879633048903241E-15, 18.08749999999999858, -34.00000000000000000 ) ) ;
#41768 = CARTESIAN_POINT ( 'NONE',  ( 25.50937500061451502, -4.541064518000417216, -2.621784821875001281 ) ) ;
#41769 = CARTESIAN_POINT ( 'NONE',  ( 28.77187500061451431, 3.027376345333613106, -5.243569643749998122 ) ) ;
#41770 = CARTESIAN_POINT ( 'NONE',  ( 20.81250000000000000, 2.886751345948129099, -4.999999999999998224 ) ) ;
#41771 = CARTESIAN_POINT ( 'NONE',  ( 3.703125000614516882, 0.000000000000000000, 5.243569643749999010 ) ) ;
#41772 = CARTESIAN_POINT ( 'NONE',  ( 21.49687500061451573, 4.119189519843966529, -2.378215178124998275 ) ) ;
#41773 = CARTESIAN_POINT ( 'NONE',  ( 17.85937500061451999, -4.541064518000417216, -2.621784821875001281 ) ) ;
#41774 = CARTESIAN_POINT ( 'NONE',  ( 7.621875000614515727, 4.119189519843966529, 2.378215178124999607 ) ) ;
#41775 = CARTESIAN_POINT ( 'NONE',  ( 28.91250000122903074, -4.330127018922190985, -2.500000000000001332 ) ) ;
#41776 = CARTESIAN_POINT ( 'NONE',  ( 9.496875000614517504, 6.054752690667223547, 3.707466751127219781E-16 ) ) ;
#41777 = CARTESIAN_POINT ( 'NONE',  ( 18.38437500061451857, 6.421520780324663323E-16, -5.243569643749999010 ) ) ;
#41778 = CARTESIAN_POINT ( 'NONE',  ( -2.008609180075752842, 25.40587078878261096, 33.46894003088245029 ) ) ;
#41779 = CARTESIAN_POINT ( 'NONE',  ( 25.98750000000000071, -2.886751345948129988, 4.999999999999997335 ) ) ;
#41780 = CARTESIAN_POINT ( 'NONE',  ( 26.85937500061451644, -4.541064518000417216, -2.621784821875001281 ) ) ;
#41781 = FACE_OUTER_BOUND ( 'NONE', #47789, .T. ) ;
#41782 = EDGE_LOOP ( 'NONE', ( #20793, #46436, #57124, #1364 ) ) ;
#41783 = CARTESIAN_POINT ( 'NONE',  ( 7.462500000000001243, 2.886751345948126879, 4.999999999999999112 ) ) ;
#41784 = CARTESIAN_POINT ( 'NONE',  ( 11.10937500061451821, 2.746126346562645981, -4.756430356249997438 ) ) ;
#41785 = CARTESIAN_POINT ( 'NONE',  ( 21.02812500061451573, 6.421520780324663323E-16, -5.243569643749999010 ) ) ;
#41786 = CARTESIAN_POINT ( 'NONE',  ( 11.66249999999999964, -5.773502691896255534, -1.060575238724906372E-15 ) ) ;
#41787 = CARTESIAN_POINT ( 'NONE',  ( 7.575000001229033053, 2.886751345948126879, 4.999999999999999112 ) ) ;
#41788 = CARTESIAN_POINT ( 'NONE',  ( 7.378125000614518036, -4.541064518000419881, 2.621784821874995952 ) ) ;
#41789 = CARTESIAN_POINT ( 'NONE',  ( 21.52499999999999858, -4.330127018922194537, 2.499999999999995559 ) ) ;
#41790 = EDGE_CURVE ( 'NONE', #18509, #15804, #58540, .T. ) ;
#41791 = CARTESIAN_POINT ( 'NONE',  ( 21.47812500061451502, 6.421520780324663323E-16, -5.243569643749999010 ) ) ;
#41792 = CARTESIAN_POINT ( 'NONE',  ( 23.62500000000000000, 4.330127018922191873, 2.499999999999999556 ) ) ;
#41793 = CARTESIAN_POINT ( 'NONE',  ( 25.68750000122903288, -4.330127018922194537, 2.499999999999995559 ) ) ;
#41794 = CARTESIAN_POINT ( 'NONE',  ( -1.878215178124999163, 20.44062499938548072, 26.74683588394047007 ) ) ;
#41795 = CARTESIAN_POINT ( 'NONE',  ( 5.212500000000002132, 2.886751345948126879, 4.999999999999999112 ) ) ;
#41796 = ORIENTED_EDGE ( 'NONE', *, *, #2338, .F. ) ;
#41797 = CARTESIAN_POINT ( 'NONE',  ( 18.32812500061451644, 6.421520780324663323E-16, -5.243569643749999010 ) ) ;
#41798 = CARTESIAN_POINT ( 'NONE',  ( 25.90312500061451573, -4.541064518000417216, -2.621784821875001281 ) ) ;
#41799 = CARTESIAN_POINT ( 'NONE',  ( 26.14687500061451431, 6.054752690667223547, 3.707466751127219781E-16 ) ) ;
#41800 = CARTESIAN_POINT ( 'NONE',  ( 14.72812500061451679, 6.421520780324663323E-16, -5.243569643749999010 ) ) ;
#41801 = CARTESIAN_POINT ( 'NONE',  ( 29.39062500061451289, -3.027376345333614438, 5.243569643749998122 ) ) ;
#41802 = CARTESIAN_POINT ( 'NONE',  ( 8.615625000614517859, 3.027376345333611329, 5.243569643749999010 ) ) ;
#41803 = DIRECTION ( 'NONE',  ( 0.000000000000000000, 0.000000000000000000, 1.000000000000000000 ) ) ;
#41804 = CARTESIAN_POINT ( 'NONE',  ( 27.15000000122902790, -2.886751345948125991, -5.000000000000000000 ) ) ;
#41805 = CARTESIAN_POINT ( 'NONE',  ( 19.69687500061451857, -2.746126346562641984, -4.756430356249999214 ) ) ;
#41806 = CARTESIAN_POINT ( 'NONE',  ( 16.26562500061451289, 3.027376345333611329, 5.243569643749999010 ) ) ;
#41807 = CARTESIAN_POINT ( 'NONE',  ( 1.626862140677534273E-15, 12.12500000122903465, -26.00000000000000355 ) ) ;
#41808 = CARTESIAN_POINT ( 'NONE',  ( 28.62187500061451573, -6.054752690667223547, -1.112240025338166033E-15 ) ) ;
#41809 = CARTESIAN_POINT ( 'NONE',  ( 9.459375000614517859, 4.541064518000418104, -2.621784821874998173 ) ) ;
#41810 = CARTESIAN_POINT ( 'NONE',  ( 9.309375000614517504, -4.541064518000417216, -2.621784821875001281 ) ) ;
#41811 = CARTESIAN_POINT ( 'NONE',  ( 18.15937500061451715, 0.000000000000000000, 5.243569643749999010 ) ) ;
#41812 = EDGE_LOOP ( 'NONE', ( #15932, #5448, #13404, #35689 ) ) ;
#41813 = CARTESIAN_POINT ( 'NONE',  ( 29.85937500061451644, 0.000000000000000000, 5.243569643749999010 ) ) ;
#41814 = CARTESIAN_POINT ( 'NONE',  ( 22.60312500061451857, 0.000000000000000000, 5.243569643749999010 ) ) ;
#41815 = CARTESIAN_POINT ( 'NONE',  ( 15.45937500061451608, 0.000000000000000000, 5.243569643749999010 ) ) ;
#41816 = CARTESIAN_POINT ( 'NONE',  ( 21.66562500061451502, 3.027376345333611329, 5.243569643749999010 ) ) ;
#41817 = CARTESIAN_POINT ( 'NONE',  ( -3.999999999999999556, 15.01250000000000107, 27.69059892324149530 ) ) ;
#41818 = CARTESIAN_POINT ( 'NONE',  ( 28.15312500061451573, -4.541064518000417216, -2.621784821875001281 ) ) ;
#41819 = CARTESIAN_POINT ( 'NONE',  ( 9.937500001229032875, -4.330127018922194537, 2.499999999999995559 ) ) ;
#41820 = VERTEX_POINT ( 'NONE', #61167 ) ;
#41821 = CARTESIAN_POINT ( 'NONE',  ( 5.025000001229035895, -5.773502691896255534, -1.060575238724906372E-15 ) ) ;
#41822 = CARTESIAN_POINT ( 'NONE',  ( -3.999999999999999556, 16.81250000000000000, -32.30940107675850470 ) ) ;
#41823 = CARTESIAN_POINT ( 'NONE',  ( 23.77500000122903145, 2.886751345948126879, 4.999999999999999112 ) ) ;
#41824 = CARTESIAN_POINT ( 'NONE',  ( -1.999999999999999112, 20.69374999877096499, 26.53589838486224650 ) ) ;
#41825 = EDGE_CURVE ( 'NONE', #44291, #3324, #48213, .T. ) ;
#41826 = CARTESIAN_POINT ( 'NONE',  ( 6.084375000614518747, -4.541064518000419881, 2.621784821874995952 ) ) ;
#41827 = CARTESIAN_POINT ( 'NONE',  ( 17.73750000000000071, 5.773502691896255534, 3.535250795749688401E-16 ) ) ;
#41828 = CARTESIAN_POINT ( 'NONE',  ( 15.81562500061451537, 3.027376345333611329, 5.243569643749999010 ) ) ;
#41829 = CARTESIAN_POINT ( 'NONE',  ( 11.55937500061451928, -4.541064518000417216, -2.621784821875001281 ) ) ;
#41830 = CARTESIAN_POINT ( 'NONE',  ( 27.78750000122903074, 4.330127018922191873, 2.499999999999999556 ) ) ;
#41831 = CARTESIAN_POINT ( 'NONE',  ( 17.55937500061451573, 4.541064518000418104, -2.621784821874998173 ) ) ;
#41832 = CARTESIAN_POINT ( 'NONE',  ( 5.634375000614519458, -4.541064518000419881, 2.621784821874995952 ) ) ;
#41833 = DIRECTION ( 'NONE',  ( -1.000000000000000000, -0.000000000000000000, -0.000000000000000000 ) ) ;
#41834 = CARTESIAN_POINT ( 'NONE',  ( 6.703125000614516438, 4.541064518000418104, -2.621784821874998173 ) ) ;
#41835 = CARTESIAN_POINT ( 'NONE',  ( 17.31562500061451715, -6.054752690667223547, -1.112240025338166033E-15 ) ) ;
#41836 = EDGE_LOOP ( 'NONE', ( #3403, #3180, #38744, #29270 ) ) ;
#41837 = VECTOR ( 'NONE', #36343, 1000.000000000000000 ) ;
#41838 = CARTESIAN_POINT ( 'NONE',  ( 16.07812500061451289, 6.421520780324663323E-16, -5.243569643749999010 ) ) ;
#41839 = CARTESIAN_POINT ( 'NONE',  ( 8.850000001229034297, 5.773502691896255534, 3.535250795749688894E-16 ) ) ;
#41840 = AXIS2_PLACEMENT_3D ( 'NONE', #7695, #1810, #69406 ) ;
#41841 = CARTESIAN_POINT ( 'NONE',  ( 10.19062500061451892, -3.027376345333610441, -5.243569643749999898 ) ) ;
#41842 = CARTESIAN_POINT ( 'NONE',  ( 20.40937500061451715, 0.000000000000000000, 4.756430356249998326 ) ) ;
#41843 = CARTESIAN_POINT ( 'NONE',  ( 10.42500000000000071, 6.123233995736764310E-16, -4.999999999999998224 ) ) ;
#41844 = CARTESIAN_POINT ( 'NONE',  ( 6.562500001229032875, 4.330127018922192761, -2.499999999999997780 ) ) ;
#41845 = EDGE_CURVE ( 'NONE', #6203, #69560, #4306, .T. ) ;
#41846 = CARTESIAN_POINT ( 'NONE',  ( 14.44687500061451679, 6.054752690667223547, 3.707466751127219781E-16 ) ) ;
#41847 = B_SPLINE_CURVE_WITH_KNOTS ( 'NONE', 3,
 ( #23533, #67178, #6559, #29091, #11010, #46083, #73068, #16539, #39453, #61609 ),
 .UNSPECIFIED., .F., .F.,
 ( 4, 3, 3, 4 ),
 ( 4.336808689942017736E-19, 7.861678629069894031E-05, 0.0001572339239830308245, 0.0003065732708899783433 ),
 .UNSPECIFIED. ) ;
#41848 = CARTESIAN_POINT ( 'NONE',  ( 16.53750000122903430, 4.330127018922191873, 2.499999999999999556 ) ) ;
#41849 = CARTESIAN_POINT ( 'NONE',  ( 25.23749999999999716, -2.886751345948125991, -5.000000000000000000 ) ) ;
#41850 = CARTESIAN_POINT ( 'NONE',  ( -4.243569643749999898, 19.76562500061451644, -32.45002607614398471 ) ) ;
#41851 = LINE ( 'NONE', #20030, #50233 ) ;
#41852 = CARTESIAN_POINT ( 'NONE',  ( 23.36250000122903359, 0.000000000000000000, 4.999999999999998224 ) ) ;
#41853 = CARTESIAN_POINT ( 'NONE',  ( 11.83125000122903181, 6.123233995736764310E-16, -4.999999999999998224 ) ) ;
#41854 = CARTESIAN_POINT ( 'NONE',  ( 3.901908842376271558, -3.126527325029728299, -4.209502533745343555 ) ) ;
#41855 = CARTESIAN_POINT ( 'NONE',  ( 16.95937500061451786, -4.541064518000417216, -2.621784821875001281 ) ) ;
#41856 = CARTESIAN_POINT ( 'NONE',  ( 18.16875000122903216, 2.886751345948129099, -4.999999999999997335 ) ) ;
#41857 = CARTESIAN_POINT ( 'NONE',  ( 13.37812500061451715, 6.421520780324663323E-16, -5.243569643749999010 ) ) ;
#41858 = CARTESIAN_POINT ( 'NONE',  ( 7.743750001229034119, -2.886751345948125991, -5.000000000000000000 ) ) ;
#41859 = CARTESIAN_POINT ( 'NONE',  ( 24.00937500061451502, 0.000000000000000000, 5.243569643749999010 ) ) ;
#41860 = CARTESIAN_POINT ( 'NONE',  ( 15.72187500061451537, 4.119189519843966529, 2.378215178124999607 ) ) ;
#41861 = CARTESIAN_POINT ( 'NONE',  ( 11.01562500061451821, -6.054752690667223547, -1.112240025338166033E-15 ) ) ;
#41862 = CARTESIAN_POINT ( 'NONE',  ( 15.64687500061451608, -3.027376345333610441, -5.243569643749999898 ) ) ;
#41863 = ORIENTED_EDGE ( 'NONE', *, *, #48670, .T. ) ;
#41864 = CARTESIAN_POINT ( 'NONE',  ( 27.34687500061451360, -3.027376345333610441, -5.243569643749999898 ) ) ;
#41865 = CARTESIAN_POINT ( 'NONE',  ( 27.85312500061451502, 4.541064518000418104, -2.621784821874998173 ) ) ;
#41866 = CARTESIAN_POINT ( 'NONE',  ( 19.11562500061451431, -6.054752690667223547, -1.112240025338166033E-15 ) ) ;
#41867 = CARTESIAN_POINT ( 'NONE',  ( 30.00000000000000000, 0.000000000000000000, 0.000000000000000000 ) ) ;
#41868 = CARTESIAN_POINT ( 'NONE',  ( 4.000000000000000000, 14.78750000000000142, 32.30940107675849760 ) ) ;
#41869 = AXIS2_PLACEMENT_3D ( 'NONE', #38133, #54406, #61034 ) ;
#41870 = CARTESIAN_POINT ( 'NONE',  ( 6.862500000000002487, 2.886751345948129099, -4.999999999999998224 ) ) ;
#41871 = CARTESIAN_POINT ( 'NONE',  ( 19.38750000122903216, -4.330127018922194537, 2.499999999999995559 ) ) ;
#41872 = CARTESIAN_POINT ( 'NONE',  ( 23.17500000122903359, 2.886751345948112668, -5.000000000000024869 ) ) ;
#41873 = CARTESIAN_POINT ( 'NONE',  ( 10.39687500061451608, 0.000000000000000000, 4.756430356249998326 ) ) ;
#41874 = ORIENTED_EDGE ( 'NONE', *, *, #57289, .T. ) ;
#41875 = CARTESIAN_POINT ( 'NONE',  ( 18.45000000000000284, -4.330127018922190985, -2.500000000000001332 ) ) ;
#41876 = CARTESIAN_POINT ( 'NONE',  ( 18.67500000000000071, 4.330127018922191873, 2.499999999999999556 ) ) ;
#41877 = CARTESIAN_POINT ( 'NONE',  ( 18.45937500061451431, 4.541064518000418104, -2.621784821874998173 ) ) ;
#41878 = CARTESIAN_POINT ( 'NONE',  ( 13.82812500061451466, 6.421520780324663323E-16, -5.243569643749999010 ) ) ;
#41880 = ORIENTED_EDGE ( 'NONE', *, *, #17845, .F. ) ;
#41879 = VECTOR ( 'NONE', #10638, 1000.000000000000227 ) ;
#41881 = CARTESIAN_POINT ( 'NONE',  ( 1.071796769724491893, 18.44509619066136707, -26.00000000000000355 ) ) ;
#41882 = CARTESIAN_POINT ( 'NONE',  ( 5.090625000614516615, -3.027376345333614438, 5.243569643749998122 ) ) ;
#41883 = CARTESIAN_POINT ( 'NONE',  ( 2.655984681222220721E-16, 12.75312499938548427, 25.66244784525396483 ) ) ;
#41884 = CARTESIAN_POINT ( 'NONE',  ( 12.41249999999999964, 2.886751345948126879, 4.999999999999999112 ) ) ;
#41885 = CARTESIAN_POINT ( 'NONE',  ( 29.55937500061451217, 2.746126346562645981, -4.756430356249997438 ) ) ;
#41886 = CARTESIAN_POINT ( 'NONE',  ( 4.243569643749999898, 15.52812500061451750, 30.00000000000000000 ) ) ;
#41887 = CARTESIAN_POINT ( 'NONE',  ( 26.80312500061451431, -4.541064518000417216, -2.621784821875001281 ) ) ;
#41888 = CARTESIAN_POINT ( 'NONE',  ( 8.400000000000000355, 0.000000000000000000, 4.999999999999998224 ) ) ;
#41889 = AXIS2_PLACEMENT_3D ( 'NONE', #7604, #69669, #41593 ) ;
#41890 = CARTESIAN_POINT ( 'NONE',  ( -3.756430356249999214, 16.42812499938548143, 27.83122392262697531 ) ) ;
#41891 = CARTESIAN_POINT ( 'NONE',  ( 23.93437500061451573, 4.541064518000418104, 2.621784821874999949 ) ) ;
#41892 = ORIENTED_EDGE ( 'NONE', *, *, #45595, .F. ) ;
#41893 = CARTESIAN_POINT ( 'NONE',  ( 21.55312500061451431, 4.541064518000418104, -2.621784821874998173 ) ) ;
#41894 = CARTESIAN_POINT ( 'NONE',  ( 24.08437500061451786, -4.541064518000419881, 2.621784821874995952 ) ) ;
#41895 = CARTESIAN_POINT ( 'NONE',  ( 4.243569643749999898, 16.84062500061459389, -27.54997392385601529 ) ) ;
#41896 = CARTESIAN_POINT ( 'NONE',  ( 7.228125000614517681, 4.541064518000418104, 2.621784821874999949 ) ) ;
#41897 = CARTESIAN_POINT ( 'NONE',  ( 25.77187500061451431, 2.746126346562643317, 4.756430356249998326 ) ) ;
#41898 = CARTESIAN_POINT ( 'NONE',  ( 23.76562500061451289, 3.027376345333612662, -5.243569643749998122 ) ) ;
#41899 = CARTESIAN_POINT ( 'NONE',  ( 10.88437500061451679, 4.119189519843966529, 2.378215178124999607 ) ) ;
#41900 = CARTESIAN_POINT ( 'NONE',  ( 3.756430356250000102, 15.34062499938548285, 30.00000000000000000 ) ) ;
#41901 =( BOUNDED_CURVE ( )  B_SPLINE_CURVE ( 2, ( #65831, #21852, #71008, #66564, #20753, #44041, #15944, #72467, #26310 ),
 .UNSPECIFIED., .F., .F. ) 
 B_SPLINE_CURVE_WITH_KNOTS ( ( 3, 2, 2, 2, 3 ),
 ( 0.8586956521739130821, 0.8623188405797101996, 0.8695652173913043237, 0.8768115942028985588, 0.8804347826086956763 ),
 .UNSPECIFIED. ) 
 CURVE ( )  GEOMETRIC_REPRESENTATION_ITEM ( )  RATIONAL_B_SPLINE_CURVE ( ( 0.9330127018922194093, 0.9330127018922194093, 1.000000000000000000, 0.8660254037844387076, 1.000000000000000000, 0.8660254037844387076, 1.000000000000000000, 0.9330127018922194093, 0.9330127018922194093 ) ) 
 REPRESENTATION_ITEM ( '' )  );
#41902 = EDGE_CURVE ( 'NONE', #27313, #65915, #46689, .T. ) ;
#41903 = CARTESIAN_POINT ( 'NONE',  ( 17.14687500061451786, 6.054752690667223547, 3.707466751127219781E-16 ) ) ;
#41904 = CARTESIAN_POINT ( 'NONE',  ( 25.54687500061451644, -3.027376345333610441, -5.243569643749999898 ) ) ;
#41905 = CARTESIAN_POINT ( 'NONE',  ( -4.243569643749999898, 14.90937500061451715, 30.00000000000000000 ) ) ;
#41906 = CARTESIAN_POINT ( 'NONE',  ( 5.053125000614517859, 0.000000000000000000, 5.243569643749999010 ) ) ;
#41907 = CARTESIAN_POINT ( 'NONE',  ( 29.31562500061451715, 3.027376345333611329, 5.243569643749999010 ) ) ;
#41908 = CARTESIAN_POINT ( 'NONE',  ( 28.56562500061451715, -6.054752690667223547, -1.112240025338166033E-15 ) ) ;
#41909 = CARTESIAN_POINT ( 'NONE',  ( 4.237500000000001599, 5.773502691896255534, 3.535250795749688401E-16 ) ) ;
#41910 = CARTESIAN_POINT ( 'NONE',  ( 5.653125000614517504, -4.541064518000417216, -2.621784821875001281 ) ) ;
#41911 = CARTESIAN_POINT ( 'NONE',  ( 10.13437500061451679, -4.541064518000419881, 2.621784821874995952 ) ) ;
#41912 =( NAMED_UNIT ( * ) PLANE_ANGLE_UNIT ( ) SI_UNIT ( $, .RADIAN. ) );
#41913 = CARTESIAN_POINT ( 'NONE',  ( 17.25000000122903288, -2.886751345948125991, -5.000000000000000000 ) ) ;
#41914 = CARTESIAN_POINT ( 'NONE',  ( 29.69062500061451715, 6.054752690667223547, 3.707466751127219781E-16 ) ) ;
#41915 = CARTESIAN_POINT ( 'NONE',  ( 6.103125000614515905, -4.541064518000417216, -2.621784821875001281 ) ) ;
#41916 = CARTESIAN_POINT ( 'NONE',  ( 2.828200636599751609E-16, 14.80624999877096570, 25.38119784648299415 ) ) ;
#41917 = CARTESIAN_POINT ( 'NONE',  ( 21.31875000122903430, 2.886751345948129099, -4.999999999999998224 ) ) ;
#41918 = CARTESIAN_POINT ( 'NONE',  ( 14.48437500061451821, 4.541064518000418104, 2.621784821874999949 ) ) ;
#41919 = CARTESIAN_POINT ( 'NONE',  ( 7.320879633048903241E-15, 17.75000000122903288, 26.00000000000000355 ) ) ;
#41920 = VERTEX_POINT ( 'NONE', #55993 ) ;
#41921 = CARTESIAN_POINT ( 'NONE',  ( 21.10312500061451502, 4.541064518000418104, -2.621784821874998173 ) ) ;
#41922 = CARTESIAN_POINT ( 'NONE',  ( 9.028125000614517504, 4.541064518000418104, 2.621784821874999949 ) ) ;
#41923 = CARTESIAN_POINT ( 'NONE',  ( 24.87187500061451573, 3.027376345333611329, 5.243569643749999010 ) ) ;
#41924 = CARTESIAN_POINT ( 'NONE',  ( 6.703125000614516438, 4.541064518000418104, -2.621784821874998173 ) ) ;
#41925 = DIRECTION ( 'NONE',  ( -1.000000000000000000, -0.000000000000000000, -0.000000000000000000 ) ) ;
#41926 = CARTESIAN_POINT ( 'NONE',  ( 11.40000000122903501, -2.886751345948125991, -5.000000000000000000 ) ) ;
#41927 = CARTESIAN_POINT ( 'NONE',  ( 25.90312500061451573, -4.541064518000417216, -2.621784821875001281 ) ) ;
#41928 = CARTESIAN_POINT ( 'NONE',  ( -2.121784821874996840, 9.978125000614518569, -26.32496088578401583 ) ) ;
#41929 = CARTESIAN_POINT ( 'NONE',  ( 11.43750000122903465, 6.123233995736764310E-16, -4.999999999999998224 ) ) ;
#41930 = CARTESIAN_POINT ( 'NONE',  ( 21.36562500061451431, -6.054752690667223547, -1.112240025338166033E-15 ) ) ;
#41931 = CARTESIAN_POINT ( 'NONE',  ( 17.05312500061451786, 4.541064518000418104, -2.621784821874998173 ) ) ;
#41932 = CARTESIAN_POINT ( 'NONE',  ( 29.67187500061451644, 2.746126346562645981, -4.756430356249997438 ) ) ;
#41933 = CARTESIAN_POINT ( 'NONE',  ( 18.22499999999999787, 4.330127018922191873, 2.499999999999999556 ) ) ;
#41934 = CARTESIAN_POINT ( 'NONE',  ( 14.81250000122903288, 0.000000000000000000, 4.999999999999998224 ) ) ;
#41935 = EDGE_CURVE ( 'NONE', #58014, #63961, #30720, .T. ) ;
#41936 = CARTESIAN_POINT ( 'NONE',  ( 11.39062500061451644, -3.027376345333614438, 5.243569643749998122 ) ) ;
#41937 = CARTESIAN_POINT ( 'NONE',  ( 13.22812500061451502, -4.541064518000419881, 2.621784821874995952 ) ) ;
#41938 = AXIS2_PLACEMENT_3D ( 'NONE', #18656, #24930, #41218 ) ;
#41939 = CARTESIAN_POINT ( 'NONE',  ( 23.77500000122903145, 2.886751345948126879, 4.999999999999999112 ) ) ;
#41940 = VECTOR ( 'NONE', #25980, 1000.000000000000000 ) ;
#41941 = CARTESIAN_POINT ( 'NONE',  ( 22.20937500061451431, 0.000000000000000000, 5.243569643749999010 ) ) ;
#41942 = CARTESIAN_POINT ( 'NONE',  ( 20.89687500061452141, -3.027376345333614438, 5.243569643749998122 ) ) ;
#41943 = DIRECTION ( 'NONE',  ( 0.000000000000000000, 0.000000000000000000, 1.000000000000000000 ) ) ;
#41944 = EDGE_CURVE ( 'NONE', #53042, #26808, #7630, .T. ) ;
#41945 = CARTESIAN_POINT ( 'NONE',  ( 7.912500001229033408, 4.330127018922192761, -2.499999999999997780 ) ) ;
#41946 =( BOUNDED_CURVE ( )  B_SPLINE_CURVE ( 2, ( #6335, #24403, #45864, #17048, #28866, #62126, #69130 ),
 .UNSPECIFIED., .F., .F. ) 
 B_SPLINE_CURVE_WITH_KNOTS ( ( 3, 2, 2, 3 ),
 ( 0.8333333333333334814, 0.8361111111111112493, 0.8388888888888890172, 0.8416666666666667851 ),
 .UNSPECIFIED. ) 
 CURVE ( )  GEOMETRIC_REPRESENTATION_ITEM ( )  RATIONAL_B_SPLINE_CURVE ( ( 0.9999999999999946709, 0.8660254037844440367, 1.000000000000000000, 0.8660254037844387076, 1.000000000000000000, 0.8660254037844333785, 1.000000000000005329 ) ) 
 REPRESENTATION_ITEM ( '' )  );
#41947 = CARTESIAN_POINT ( 'NONE',  ( 6.496875000614517504, -3.027376345333614438, 5.243569643749998122 ) ) ;
#41948 = CARTESIAN_POINT ( 'NONE',  ( 26.29687500061451644, -3.027376345333614438, 5.243569643749998122 ) ) ;
#41949 =( BOUNDED_CURVE ( )  B_SPLINE_CURVE ( 2, ( #39348, #10896, #5361, #22697, #17156, #67428, #39714, #62232, #51150 ),
 .UNSPECIFIED., .F., .F. ) 
 B_SPLINE_CURVE_WITH_KNOTS ( ( 3, 2, 2, 2, 3 ),
 ( 0.6413043478260869179, 0.6449275362318840354, 0.6521739130434782705, 0.6594202898550725056, 0.6630434782608696231 ),
 .UNSPECIFIED. ) 
 CURVE ( )  GEOMETRIC_REPRESENTATION_ITEM ( )  RATIONAL_B_SPLINE_CURVE ( ( 0.9330127018922194093, 0.9330127018922194093, 1.000000000000000000, 0.8660254037844387076, 1.000000000000000000, 0.8660254037844387076, 1.000000000000000000, 0.9330127018922182991, 0.9330127018922192983 ) ) 
 REPRESENTATION_ITEM ( '' )  );
#41950 = CARTESIAN_POINT ( 'NONE',  ( 4.256295036913345875, -2.623882848654998323, -4.373091964381822017 ) ) ;
#41951 = CARTESIAN_POINT ( 'NONE',  ( 20.42812500061451431, -4.541064518000419881, 2.621784821874995952 ) ) ;
#41952 = CARTESIAN_POINT ( 'NONE',  ( 23.55937500061451573, 0.000000000000000000, 5.243569643749999010 ) ) ;
#41953 = CARTESIAN_POINT ( 'NONE',  ( 2.655984681222220721E-16, 16.46562499938548285, 25.66244784525396483 ) ) ;
#41954 = CARTESIAN_POINT ( 'NONE',  ( 3.242103837493086330E-14, 13.13749999999999929, 26.00000000000000711 ) ) ;
#41955 = CARTESIAN_POINT ( 'NONE',  ( 3.999999999999998668, 15.76250000000000107, 27.69059892324149530 ) ) ;
#41956 = CARTESIAN_POINT ( 'NONE',  ( 5.446875000614518569, 6.054752690667223547, 3.707466751127219781E-16 ) ) ;
#41957 = CARTESIAN_POINT ( 'NONE',  ( 17.27812500061451217, -4.541064518000419881, 2.621784821874995952 ) ) ;
#41958 = ORIENTED_EDGE ( 'NONE', *, *, #26495, .F. ) ;
#41959 = CARTESIAN_POINT ( 'NONE',  ( 25.90312500061451573, -4.541064518000417216, -2.621784821875001281 ) ) ;
#41960 = CARTESIAN_POINT ( 'NONE',  ( 2.934375000614518392, -4.541064518000419881, 2.621784821874995952 ) ) ;
#41961 = CARTESIAN_POINT ( 'NONE',  ( 4.704389487731190478, 1.694379531550751272, 4.836684215720605806 ) ) ;
#41962 = DIRECTION ( 'NONE',  ( -0.000000000000000000, -1.000000000000000000, -0.000000000000000000 ) ) ;
#41963 = CARTESIAN_POINT ( 'NONE',  ( 14.55000000000000071, 4.330127018922192761, -2.499999999999997780 ) ) ;
#41964 = CARTESIAN_POINT ( 'NONE',  ( 21.06562500061451715, 3.027376345333613106, -5.243569643749998122 ) ) ;
#41965 = EDGE_CURVE ( 'NONE', #66756, #67375, #53381, .T. ) ;
#41966 = ORIENTED_EDGE ( 'NONE', *, *, #69513, .T. ) ;
#41967 = CARTESIAN_POINT ( 'NONE',  ( 24.56250000000000000, 2.886751345948126879, 4.999999999999999112 ) ) ;
#41968 = CARTESIAN_POINT ( 'NONE',  ( 25.99687500061451928, -3.027376345333610441, -5.243569643749999898 ) ) ;
#41969 =( BOUNDED_CURVE ( )  B_SPLINE_CURVE ( 2, ( #60655, #33327, #20772, #72123, #66961, #55139, #16327 ),
 .UNSPECIFIED., .F., .T. ) 
 B_SPLINE_CURVE_WITH_KNOTS ( ( 3, 2, 2, 3 ),
 ( 0.4700000000000001399, 0.4733333333333334392, 0.4766666666666666829, 0.4799999999999999267 ),
 .UNSPECIFIED. ) 
 CURVE ( )  GEOMETRIC_REPRESENTATION_ITEM ( )  RATIONAL_B_SPLINE_CURVE ( ( 0.9999999999999933387, 0.8660254037844453689, 1.000000000000000000, 0.8660254037844387076, 1.000000000000000000, 0.8660254037844409281, 0.9999999999999977796 ) ) 
 REPRESENTATION_ITEM ( '' )  );
#41970 = VERTEX_POINT ( 'NONE', #32361 ) ;
#41971 = CARTESIAN_POINT ( 'NONE',  ( 25.83749999999999503, 5.773502691896255534, 3.535250795749688401E-16 ) ) ;
#41972 = CARTESIAN_POINT ( 'NONE',  ( 14.09062500061451750, -3.027376345333614438, 5.243569643749998122 ) ) ;
#41973 = CARTESIAN_POINT ( 'NONE',  ( 25.12500000122902932, 2.886751345948143754, 4.999999999999969802 ) ) ;
#41974 = CARTESIAN_POINT ( 'NONE',  ( 16.58437500061451431, 5.492252693125287522, 3.363034840372157021E-16 ) ) ;
#41975 = CARTESIAN_POINT ( 'NONE',  ( 3.121875000614518836, 3.027376345333613106, -5.243569643749998122 ) ) ;
#41976 = CARTESIAN_POINT ( 'NONE',  ( 12.07500000122903216, 2.886751345948126879, 4.999999999999999112 ) ) ;
#41977 = CARTESIAN_POINT ( 'NONE',  ( 18.75000000000000000, 0.000000000000000000, 4.999999999999998224 ) ) ;
#41978 = CARTESIAN_POINT ( 'NONE',  ( 27.00000000000000000, -4.330127018922190985, -2.500000000000001332 ) ) ;
#41979 = CARTESIAN_POINT ( 'NONE',  ( 3.187500001229033764, -4.330127018922194537, 2.499999999999995559 ) ) ;
#41980 = CARTESIAN_POINT ( 'NONE',  ( 7.509375000614517681, -4.541064518000417216, -2.621784821875001281 ) ) ;
#41981 = CARTESIAN_POINT ( 'NONE',  ( 19.80937500061451573, 4.541064518000418104, -2.621784821874998173 ) ) ;
#41982 = CARTESIAN_POINT ( 'NONE',  ( 19.98750000122903359, 6.123233995736764310E-16, -4.999999999999998224 ) ) ;
#41983 = ORIENTED_EDGE ( 'NONE', *, *, #40580, .T. ) ;
#41984 = CARTESIAN_POINT ( 'NONE',  ( 27.81562500061452070, 3.027376345333613106, -5.243569643749998122 ) ) ;
#41985 = CARTESIAN_POINT ( 'NONE',  ( 4.162499999999999645, 2.886751345948129099, -4.999999999999998224 ) ) ;
#41986 = EDGE_CURVE ( 'NONE', #33272, #27910, #70853, .T. ) ;
#41987 = CARTESIAN_POINT ( 'NONE',  ( 4.396875000614516971, -3.027376345333610441, -5.243569643749999898 ) ) ;
#41988 = CARTESIAN_POINT ( 'NONE',  ( 15.15000000000000036, 0.000000000000000000, 4.999999999999998224 ) ) ;
#41989 = CARTESIAN_POINT ( 'NONE',  ( 13.82812500061451466, 6.421520780324663323E-16, -5.243569643749999010 ) ) ;
#41990 = CARTESIAN_POINT ( 'NONE',  ( 25.96875000122903998, 2.886751345948113556, 5.000000000000023093 ) ) ;
#41991 = CARTESIAN_POINT ( 'NONE',  ( -3.999999999999999112, 18.03124999877096712, 27.69059892324149530 ) ) ;
#41992 = CARTESIAN_POINT ( 'NONE',  ( 45.00000000000000000, 6.123233995736764310E-16, -4.999999999999998224 ) ) ;
#41993 = CARTESIAN_POINT ( 'NONE',  ( 17.85000000122903430, 5.773502691896255534, 3.535250795749688894E-16 ) ) ;
#41994 = CARTESIAN_POINT ( 'NONE',  ( -4.000000000000000888, 19.45624999877097139, 32.30940107675850470 ) ) ;
#41995 = CARTESIAN_POINT ( 'NONE',  ( 16.65937500061452070, 4.119189519843966529, -2.378215178124998275 ) ) ;
#41996 = CARTESIAN_POINT ( 'NONE',  ( 7.528125000614515727, 6.421520780324663323E-16, -5.243569643749999010 ) ) ;
#41997 = CARTESIAN_POINT ( 'NONE',  ( 24.08437500061451786, -4.541064518000419881, 2.621784821874995952 ) ) ;
#41998 = CARTESIAN_POINT ( 'NONE',  ( 27.00000000122903288, -2.886751345948096681, 5.000000000000054179 ) ) ;
#41999 = CARTESIAN_POINT ( 'NONE',  ( 24.00937500061451502, 0.000000000000000000, 5.243569643749999010 ) ) ;
#42000 = CARTESIAN_POINT ( 'NONE',  ( 6.150000000000003020, 0.000000000000000000, 4.999999999999998224 ) ) ;
#42001 = CARTESIAN_POINT ( 'NONE',  ( -3.999999999999999556, 10.62500000122903643, 27.69059892324149530 ) ) ;
#42002 = CARTESIAN_POINT ( 'NONE',  ( 15.62812500061451537, 6.421520780324663323E-16, -5.243569643749999010 ) ) ;
#42003 = CARTESIAN_POINT ( 'NONE',  ( 4.387500001229033053, 4.330127018922191873, 2.499999999999999556 ) ) ;
#42004 = CARTESIAN_POINT ( 'NONE',  ( 9.459375000614517859, 4.541064518000418104, -2.621784821874998173 ) ) ;
#42005 = CARTESIAN_POINT ( 'NONE',  ( 3.807538167735159185, -3.240779705755961526, 4.122180188640082399 ) ) ;
#42006 = EDGE_LOOP ( 'NONE', ( #51893, #17082, #48386, #16752, #71608, #48197, #28054, #72021, #31934, #62584, #27174, #53704, #37654, #5823, #42244, #63677, #45195, #58423, #3699, #60488, #58322, #36737, #52824, #59107, #23514, #8101, #5609, #7162, #46636, #67513, #66328, #60051, #62494, #70781, #9082, #12473, #32206, #14302, #55877, #72868, #14977, #69150, #49033, #51017, #41301, #26289, #71125 ) ) ;
#42007 = CARTESIAN_POINT ( 'NONE',  ( 12.29062500061451857, -3.027376345333614438, 5.243569643749998122 ) ) ;
#42008 = LINE ( 'NONE', #63796, #13121 ) ;
#42009 = CARTESIAN_POINT ( 'NONE',  ( 23.36250000122903359, 0.000000000000000000, 4.999999999999998224 ) ) ;
#42010 = CARTESIAN_POINT ( 'NONE',  ( 11.37187500061451750, 3.027376345333611329, 5.243569643749999010 ) ) ;
#42011 = CARTESIAN_POINT ( 'NONE',  ( 11.91562500061451857, -6.054752690667223547, -1.112240025338166033E-15 ) ) ;
#42012 = CARTESIAN_POINT ( 'NONE',  ( 29.38125000122903074, 6.123233995736764310E-16, -4.999999999999998224 ) ) ;
#42013 = CARTESIAN_POINT ( 'NONE',  ( 24.64687500061451431, -3.027376345333610441, -5.243569643749999898 ) ) ;
#42014 = DIRECTION ( 'NONE',  ( 0.000000000000000000, 0.000000000000000000, -1.000000000000000000 ) ) ;
#42015 = CARTESIAN_POINT ( 'NONE',  ( -5.810221930991193690E-16, 10.10000000122903430, -34.00000000000000000 ) ) ;
#42016 = CARTESIAN_POINT ( 'NONE',  ( 20.55000000122903359, 5.773502691896255534, 3.535250795749688401E-16 ) ) ;
#42017 = CARTESIAN_POINT ( 'NONE',  ( 4.243569643749999898, 14.68437500061451750, -30.00000000000000000 ) ) ;
#42018 = CARTESIAN_POINT ( 'NONE',  ( 16.92187500061451999, -6.054752690667223547, -1.112240025338166033E-15 ) ) ;
#42019 = CARTESIAN_POINT ( 'NONE',  ( 16.83750000122903145, 6.123233995736764310E-16, -4.999999999999998224 ) ) ;
#42020 = CARTESIAN_POINT ( 'NONE',  ( 11.93437500061451573, -4.541064518000419881, 2.621784821874995952 ) ) ;
#42021 = CARTESIAN_POINT ( 'NONE',  ( -4.243569643749999898, 17.10312500061451502, -30.00000000000000000 ) ) ;
#42022 = CARTESIAN_POINT ( 'NONE',  ( 20.17500000122903359, 2.886751345948126879, 4.999999999999999112 ) ) ;
#42023 = CARTESIAN_POINT ( 'NONE',  ( 12.81562500061451537, -6.054752690667223547, -1.112240025338166033E-15 ) ) ;
#42024 = ORIENTED_EDGE ( 'NONE', *, *, #20707, .T. ) ;
#42025 = EDGE_LOOP ( 'NONE', ( #13742, #53655, #44991, #66280 ) ) ;
#42026 = CARTESIAN_POINT ( 'NONE',  ( 15.26249999999999929, -5.773502691896255534, -1.060575238724906372E-15 ) ) ;
#42027 = CARTESIAN_POINT ( 'NONE',  ( 18.07499999999999929, 6.123233995736764310E-16, -4.999999999999998224 ) ) ;
#42028 = CARTESIAN_POINT ( 'NONE',  ( 11.85937500061451644, 0.000000000000000000, 5.243569643749999010 ) ) ;
#42029 = CARTESIAN_POINT ( 'NONE',  ( 4.094832220624204489, 2.869363679410234624, 4.355156543258145163 ) ) ;
#42030 = CARTESIAN_POINT ( 'NONE',  ( 11.85000000122903430, -2.886751345948125991, -5.000000000000000000 ) ) ;
#42031 = CARTESIAN_POINT ( 'NONE',  ( 21.63750000122903572, -4.330127018922194537, 2.499999999999995559 ) ) ;
#42032 = CARTESIAN_POINT ( 'NONE',  ( 17.39062500061451644, -3.027376345333610441, -5.243569643749999898 ) ) ;
#42033 = CARTESIAN_POINT ( 'NONE',  ( 21.59062500061451928, 6.054752690667223547, 3.707466751127219781E-16 ) ) ;
#42034 = CARTESIAN_POINT ( 'NONE',  ( 27.78750000122903074, 4.330127018922191873, 2.499999999999999556 ) ) ;
#42035 = CARTESIAN_POINT ( 'NONE',  ( 25.80000000000000071, 4.330127018922192761, -2.499999999999997780 ) ) ;
#42036 = CARTESIAN_POINT ( 'NONE',  ( 20.32499999999999929, 6.123233995736764310E-16, -4.999999999999998224 ) ) ;
#42037 = AXIS2_PLACEMENT_3D ( 'NONE', #67318, #50324, #16677 ) ;
#42038 = CARTESIAN_POINT ( 'NONE',  ( 7.509375000614517681, -4.119189519843965641, -2.378215178125001383 ) ) ;
#42039 = CARTESIAN_POINT ( 'NONE',  ( 28.95937500061451431, 0.000000000000000000, 5.243569643749999010 ) ) ;
#42040 = CARTESIAN_POINT ( 'NONE',  ( 4.059357805649630002, -2.919411146374983446, -4.104029762320235086 ) ) ;
#42041 = CARTESIAN_POINT ( 'NONE',  ( 4.243569643749999010, 13.82187500061451857, -32.45002607614398471 ) ) ;
#42042 = CARTESIAN_POINT ( 'NONE',  ( 4.237500001229036251, 6.123233995736764310E-16, -4.999999999999998224 ) ) ;
#42043 = CARTESIAN_POINT ( 'NONE',  ( 4.875000000000000888, -4.330127018922194537, 2.499999999999995559 ) ) ;
#42044 = FACE_OUTER_BOUND ( 'NONE', #42255, .T. ) ;
#42045 = CARTESIAN_POINT ( 'NONE',  ( 7.771875000614516971, 3.027376345333611329, 5.243569643749999010 ) ) ;
#42046 = CARTESIAN_POINT ( 'NONE',  ( 27.89062500061451289, 6.054752690667223547, 3.707466751127219781E-16 ) ) ;
#42047 = FACE_OUTER_BOUND ( 'NONE', #70463, .T. ) ;
#42048 = CARTESIAN_POINT ( 'NONE',  ( 5.400000001229029678, -2.886751345948063374, 5.000000000000112799 ) ) ;
#42049 = CYLINDRICAL_SURFACE ( 'NONE', #41840, 4.000000000000000000 ) ;
#42050 = CARTESIAN_POINT ( 'NONE',  ( 6.084375000614518747, -4.541064518000419881, 2.621784821874995952 ) ) ;
#42051 = CARTESIAN_POINT ( 'NONE',  ( 11.63437500061451857, 6.421520780324663323E-16, -5.243569643749999010 ) ) ;
#42052 = EDGE_CURVE ( 'NONE', #19796, #59956, #53621, .T. ) ;
#42053 = CARTESIAN_POINT ( 'NONE',  ( 4.875000000000000888, -4.330127018922194537, 2.499999999999995559 ) ) ;
#42054 = CARTESIAN_POINT ( 'NONE',  ( 2.121784821874999061, 13.80312500061459602, 26.32496088578401583 ) ) ;
#42055 = CARTESIAN_POINT ( 'NONE',  ( 4.000000000000000000, 13.43750000000000000, 27.69059892324149885 ) ) ;
#42056 = CARTESIAN_POINT ( 'NONE',  ( 6.899999999999999467, 4.330127018922192761, -2.499999999999997780 ) ) ;
#42057 = CARTESIAN_POINT ( 'NONE',  ( 15.87187500061451573, -4.119189519843968306, 2.378215178124996054 ) ) ;
#42058 = CARTESIAN_POINT ( 'NONE',  ( 19.79062500061451502, 6.054752690667223547, 3.707466751127219781E-16 ) ) ;
#42059 = CARTESIAN_POINT ( 'NONE',  ( 12.25312500061451537, 0.000000000000000000, 5.243569643749999010 ) ) ;
#42060 = CARTESIAN_POINT ( 'NONE',  ( 23.22187500061451360, 5.824947211148865298E-16, -4.756430356249998326 ) ) ;
#42061 = CARTESIAN_POINT ( 'NONE',  ( 9.046875000614518214, 6.054752690667223547, 3.707466751127219781E-16 ) ) ;
#42062 = CARTESIAN_POINT ( 'NONE',  ( 26.09999999999999787, -4.330127018922190985, -2.500000000000001332 ) ) ;
#42063 = CARTESIAN_POINT ( 'NONE',  ( 22.72500000122903430, 2.886751345948129099, -4.999999999999998224 ) ) ;
#42064 = CARTESIAN_POINT ( 'NONE',  ( 45.00000000000000000, 6.123233995736764310E-16, -4.999999999999998224 ) ) ;
#42065 = CARTESIAN_POINT ( 'NONE',  ( 9.796875000614519990, -3.027376345333610441, -5.243569643749999898 ) ) ;
#42066 = CARTESIAN_POINT ( 'NONE',  ( 27.53437500061451360, 4.541064518000418104, 2.621784821874999949 ) ) ;
#42067 = VECTOR ( 'NONE', #36166, 1000.000000000000000 ) ;
#42068 = CARTESIAN_POINT ( 'NONE',  ( 8.737500001229033586, 6.123233995736764310E-16, -4.999999999999998224 ) ) ;
#42069 = CARTESIAN_POINT ( 'NONE',  ( -3.999999999999999112, 12.87500000122903465, -32.30940107675850470 ) ) ;
#42070 = ADVANCED_FACE ( 'NONE', ( #40454 ), #43033, .T. ) ;
#42071 = CARTESIAN_POINT ( 'NONE',  ( 20.74687500061451573, 6.054752690667223547, 3.707466751127219781E-16 ) ) ;
#42072 = CARTESIAN_POINT ( 'NONE',  ( 10.80937500061451928, 4.541064518000418104, -2.621784821874998173 ) ) ;
#42073 = CARTESIAN_POINT ( 'NONE',  ( 1.878215178125000495, 12.71562499938548463, 26.74683588394047007 ) ) ;
#42074 = CARTESIAN_POINT ( 'NONE',  ( 24.56250000000000000, 2.886751345948126879, 4.999999999999999112 ) ) ;
#42075 = CARTESIAN_POINT ( 'NONE',  ( -4.000000000000000888, 14.11249999999999893, 32.30940107675850470 ) ) ;
#42076 = CARTESIAN_POINT ( 'NONE',  ( 9.001249775931846008E-16, 12.77187500061451786, -25.09994784771203058 ) ) ;
#42077 = CARTESIAN_POINT ( 'NONE',  ( 25.88437500061451502, -4.119189519843968306, 2.378215178124996054 ) ) ;
#42078 = CARTESIAN_POINT ( 'NONE',  ( 15.44062500061451537, -3.027376345333614438, 5.243569643749998122 ) ) ;
#42079 = CARTESIAN_POINT ( 'NONE',  ( 4.612500000000002487, 2.886751345948129099, -4.999999999999998224 ) ) ;
#42080 = DIRECTION ( 'NONE',  ( -1.000000000000000000, -0.000000000000000000, -0.000000000000000000 ) ) ;
#42081 = CARTESIAN_POINT ( 'NONE',  ( 5.810221930991193690E-16, 20.20624999877096428, 26.00000000000000000 ) ) ;
#42082 = CARTESIAN_POINT ( 'NONE',  ( 14.55000000000000071, 4.330127018922192761, -2.499999999999997780 ) ) ;
#42083 = ADVANCED_FACE ( 'NONE', ( #66514 ), #55437, .F. ) ;
#42084 = CARTESIAN_POINT ( 'NONE',  ( -2.000000000000000000, 17.33750000122903145, 26.53589838486224650 ) ) ;
#42085 = CARTESIAN_POINT ( 'NONE',  ( 12.93750000122903465, 4.330127018922191873, 2.499999999999999556 ) ) ;
#42086 = CARTESIAN_POINT ( 'NONE',  ( 24.72187500061451360, 3.027376345333613106, -5.243569643749998122 ) ) ;
#42087 = CARTESIAN_POINT ( 'NONE',  ( 16.28437500061452070, 4.541064518000418104, 2.621784821874999949 ) ) ;
#42088 = CIRCLE ( 'NONE', #65387, 4.999999999999998224 ) ;
#42089 = ORIENTED_EDGE ( 'NONE', *, *, #68503, .T. ) ;
#42090 = CARTESIAN_POINT ( 'NONE',  ( 19.22812500061451502, 6.421520780324663323E-16, -5.243569643749999010 ) ) ;
#42091 = CARTESIAN_POINT ( 'NONE',  ( 3.140625000614516882, 6.054752690667223547, 3.707466751127219781E-16 ) ) ;
#42092 = CARTESIAN_POINT ( 'NONE',  ( 18.79687500061451644, -3.027376345333610441, -5.243569643749999898 ) ) ;
#42093 = CARTESIAN_POINT ( 'NONE',  ( 28.20937500061451786, -4.541064518000417216, -2.621784821875001281 ) ) ;
#42094 = CARTESIAN_POINT ( 'NONE',  ( 4.978125000614518569, 4.541064518000418104, 2.621784821874999949 ) ) ;
#42095 = CARTESIAN_POINT ( 'NONE',  ( 22.97812500061451857, 4.541064518000418104, 2.621784821874999949 ) ) ;
#42096 = CARTESIAN_POINT ( 'NONE',  ( -4.243569643749999898, 15.71562500061451573, 27.54997392385601529 ) ) ;
#42097 = CARTESIAN_POINT ( 'NONE',  ( 15.60000000122903607, 5.773502691896255534, 3.535250795749688894E-16 ) ) ;
#42098 = CARTESIAN_POINT ( 'NONE',  ( 12.90937500061451537, -4.119189519843965641, -2.378215178125001383 ) ) ;
#42099 = CARTESIAN_POINT ( 'NONE',  ( 6.815625000614518925, 3.027376345333611329, 5.243569643749999010 ) ) ;
#42100 = DIRECTION ( 'NONE',  ( -0.000000000000000000, -1.000000000000000000, -0.000000000000000000 ) ) ;
#42101 = CARTESIAN_POINT ( 'NONE',  ( 28.71562500061451573, 3.027376345333613106, -5.243569643749998122 ) ) ;
#42102 = CARTESIAN_POINT ( 'NONE',  ( 22.92187500061451644, 3.027376345333613106, -5.243569643749998122 ) ) ;
#42103 = CARTESIAN_POINT ( 'NONE',  ( 15.06562500061451537, -6.054752690667223547, -1.112240025338166033E-15 ) ) ;
#42104 = CARTESIAN_POINT ( 'NONE',  ( 23.70000000122903216, 5.773502691896255534, 3.535250795749688894E-16 ) ) ;
#42105 = CARTESIAN_POINT ( 'NONE',  ( 24.32812500061451289, 4.541064518000418104, 2.621784821874999949 ) ) ;
#42106 = CARTESIAN_POINT ( 'NONE',  ( 20.22187500061451715, 3.027376345333613106, -5.243569643749998122 ) ) ;
#42107 = CARTESIAN_POINT ( 'NONE',  ( 13.64062500061451644, -3.027376345333614438, 5.243569643749998122 ) ) ;
#42108 = CARTESIAN_POINT ( 'NONE',  ( 4.243569643749999898, 14.64687500061451964, 32.45002607614398471 ) ) ;
#42109 = CARTESIAN_POINT ( 'NONE',  ( 19.49062500061451431, -3.027376345333614438, 5.243569643749998122 ) ) ;
#42110 = CARTESIAN_POINT ( 'NONE',  ( 28.64062500061451289, -3.027376345333610441, -5.243569643749999898 ) ) ;
#42111 = ORIENTED_EDGE ( 'NONE', *, *, #336, .F. ) ;
#42112 = CARTESIAN_POINT ( 'NONE',  ( 26.21249999999999858, 2.886751345948129099, -4.999999999999998224 ) ) ;
#42113 = CARTESIAN_POINT ( 'NONE',  ( -2.828200636599751609E-16, 10.88750000000000107, -34.61880215351700230 ) ) ;
#42114 = CARTESIAN_POINT ( 'NONE',  ( 26.84062500061451573, -3.027376345333610441, -5.243569643749999898 ) ) ;
#42115 = CARTESIAN_POINT ( 'NONE',  ( 8.353125000614518569, -4.541064518000417216, -2.621784821875001281 ) ) ;
#42116 = CARTESIAN_POINT ( 'NONE',  ( 20.32500000122903572, -5.773502691896255534, -1.060575238724906372E-15 ) ) ;
#42117 = CARTESIAN_POINT ( 'NONE',  ( 23.69062500061451004, -3.027376345333610441, -5.243569643749999898 ) ) ;
#42118 = CARTESIAN_POINT ( 'NONE',  ( 25.98750000000000071, -2.886751345948129988, 4.999999999999997335 ) ) ;
#42119 = CARTESIAN_POINT ( 'NONE',  ( 28.86562500061451786, 3.027376345333611329, 5.243569643749999010 ) ) ;
#42120 = CARTESIAN_POINT ( 'NONE',  ( 7.753125000614518036, 0.000000000000000000, 5.243569643749999010 ) ) ;
#42121 = ORIENTED_EDGE ( 'NONE', *, *, #63109, .F. ) ;
#42122 = CARTESIAN_POINT ( 'NONE',  ( 26.57812500061451644, 4.541064518000418104, 2.621784821874999949 ) ) ;
#42123 = CARTESIAN_POINT ( 'NONE',  ( 5.803125000614517859, 4.541064518000418104, -2.621784821874998173 ) ) ;
#42124 = CARTESIAN_POINT ( 'NONE',  ( 13.32187500061451502, -5.492252693125287522, -1.008910452111647106E-15 ) ) ;
#42125 = CARTESIAN_POINT ( 'NONE',  ( 0.000000000000000000, 20.00000000000000000, 30.00000000000000000 ) ) ;
#42126 = VECTOR ( 'NONE', #5667, 1000.000000000000000 ) ;
#42127 = CARTESIAN_POINT ( 'NONE',  ( 13.91249999999999964, -5.773502691896255534, -1.060575238724906372E-15 ) ) ;
#42128 = CARTESIAN_POINT ( 'NONE',  ( 14.18437500061451750, -4.541064518000419881, 2.621784821874995952 ) ) ;
#42129 = CARTESIAN_POINT ( 'NONE',  ( 9.150000001229033231, -2.886751345948125991, -5.000000000000000000 ) ) ;
#42130 = CARTESIAN_POINT ( 'NONE',  ( 17.22187500061451715, 3.027376345333611329, 5.243569643749999010 ) ) ;
#42131 = CARTESIAN_POINT ( 'NONE',  ( 15.29999999999999893, -4.330127018922190985, -2.500000000000001332 ) ) ;
#42132 = CARTESIAN_POINT ( 'NONE',  ( 9.571875000614518569, 3.027376345333611329, 5.243569643749999010 ) ) ;
#42133 = CARTESIAN_POINT ( 'NONE',  ( 9.001249775931846008E-16, 12.26562500061451644, -25.09994784771203058 ) ) ;
#42134 = FACE_OUTER_BOUND ( 'NONE', #50171, .T. ) ;
#42135 = CARTESIAN_POINT ( 'NONE',  ( 24.27187500061451431, 4.119189519843966529, 2.378215178124999607 ) ) ;
#42136 = ORIENTED_EDGE ( 'NONE', *, *, #50186, .F. ) ;
#42137 = CARTESIAN_POINT ( 'NONE',  ( 25.00312500061451715, -4.541064518000417216, -2.621784821875001281 ) ) ;
#42138 = CARTESIAN_POINT ( 'NONE',  ( 4.243569643749999010, 10.22187500061451892, 27.54997392385601174 ) ) ;
#42139 = CARTESIAN_POINT ( 'NONE',  ( 45.00000000000000000, 0.000000000000000000, 4.999999999999998224 ) ) ;
#42140 = CARTESIAN_POINT ( 'NONE',  ( 26.48437500061451644, 6.421520780324663323E-16, -5.243569643749999010 ) ) ;
#42141 = CARTESIAN_POINT ( 'NONE',  ( 27.94687500061451502, 6.054752690667223547, 3.707466751127219781E-16 ) ) ;
#42142 = CARTESIAN_POINT ( 'NONE',  ( 3.590625000614518836, 6.054752690667223547, 3.707466751127219781E-16 ) ) ;
#42143 = CARTESIAN_POINT ( 'NONE',  ( 21.38437500061451502, -2.746126346562642428, -4.756430356249999214 ) ) ;
#42144 = CARTESIAN_POINT ( 'NONE',  ( 16.28437500061452070, 4.541064518000418104, 2.621784821874999949 ) ) ;
#42145 = CARTESIAN_POINT ( 'NONE',  ( 9.346875000614517148, 4.119189519843966529, -2.378215178124998275 ) ) ;
#42146 = CARTESIAN_POINT ( 'NONE',  ( 3.215625000614518836, 3.027376345333611329, 5.243569643749999010 ) ) ;
#42147 = CARTESIAN_POINT ( 'NONE',  ( 7.096875000614517148, -3.027376345333610441, -5.243569643749999898 ) ) ;
#42148 = CARTESIAN_POINT ( 'NONE',  ( 17.10937500061451999, 4.541064518000418104, -2.621784821874998173 ) ) ;
#42149 = CARTESIAN_POINT ( 'NONE',  ( 9.843750001229032875, -2.886751345948130876, 4.999999999999996447 ) ) ;
#42150 = CARTESIAN_POINT ( 'NONE',  ( 26.58750000000000213, -2.886751345948125991, -5.000000000000000000 ) ) ;
#42151 = CARTESIAN_POINT ( 'NONE',  ( 27.79687500061451999, -3.027376345333610441, -5.243569643749999898 ) ) ;
#42152 = CARTESIAN_POINT ( 'NONE',  ( -3.756430356250000102, 13.42812499938548321, 30.00000000000000000 ) ) ;
#42153 = CARTESIAN_POINT ( 'NONE',  ( 29.84999999999999787, 4.330127018922192761, -2.499999999999997780 ) ) ;
#42154 = ORIENTED_EDGE ( 'NONE', *, *, #38075, .F. ) ;
#42155 = CARTESIAN_POINT ( 'NONE',  ( 8.212500000000000355, 2.886751345948129099, -4.999999999999998224 ) ) ;
#42156 = CARTESIAN_POINT ( 'NONE',  ( 8.334375000614516082, -2.746126346562642428, -4.756430356249999214 ) ) ;
#42157 = CARTESIAN_POINT ( 'NONE',  ( 22.86562500061451431, 3.027376345333613106, -5.243569643749998122 ) ) ;
#42158 = CARTESIAN_POINT ( 'NONE',  ( 12.41249999999999964, 2.886751345948126879, 4.999999999999999112 ) ) ;
#42159 = CARTESIAN_POINT ( 'NONE',  ( 7.762500001229033053, -4.330127018922190985, -2.500000000000001332 ) ) ;
#42160 = CARTESIAN_POINT ( 'NONE',  ( 6.890625000614516438, -3.027376345333614438, 5.243569643749998122 ) ) ;
#42161 = CARTESIAN_POINT ( 'NONE',  ( 22.61250000000000071, 2.886751345948129099, -4.999999999999998224 ) ) ;
#42162 = EDGE_CURVE ( 'NONE', #37978, #12333, #60930, .T. ) ;
#42163 = CARTESIAN_POINT ( 'NONE',  ( 19.64062500061451644, -3.027376345333610441, -5.243569643749999898 ) ) ;
#42164 = CARTESIAN_POINT ( 'NONE',  ( 14.81250000000000178, -5.773502691896255534, -1.060575238724906372E-15 ) ) ;
#42165 = CARTESIAN_POINT ( 'NONE',  ( 25.16250000122903074, 0.000000000000000000, 4.999999999999998224 ) ) ;
#42166 = CARTESIAN_POINT ( 'NONE',  ( -3.756430356250000102, 20.51562499938548356, 30.00000000000000000 ) ) ;
#42167 = CARTESIAN_POINT ( 'NONE',  ( 6.187500000000002665, -2.886751345948129988, 4.999999999999997335 ) ) ;
#42168 = ORIENTED_EDGE ( 'NONE', *, *, #29620, .F. ) ;
#42169 = CARTESIAN_POINT ( 'NONE',  ( 20.50312500061451715, -4.541064518000417216, -2.621784821875001281 ) ) ;
#42170 = CARTESIAN_POINT ( 'NONE',  ( 25.67812500061451431, 4.541064518000418104, 2.621784821874999949 ) ) ;
#42171 = CARTESIAN_POINT ( 'NONE',  ( 26.59687500061451360, 6.054752690667223547, 3.707466751127219781E-16 ) ) ;
#42172 = CARTESIAN_POINT ( 'NONE',  ( 9.674999999999998934, 4.330127018922191873, 2.499999999999999556 ) ) ;
#42173 = CARTESIAN_POINT ( 'NONE',  ( 10.82812500061451644, 4.541064518000418104, 2.621784821874999949 ) ) ;
#42174 = CARTESIAN_POINT ( 'NONE',  ( 4.898587196589411843E-16, 20.00000000000000000, 33.99999999999999289 ) ) ;
#42175 = CARTESIAN_POINT ( 'NONE',  ( 8.503125000614515372, 4.541064518000418104, -2.621784821874998173 ) ) ;
#42176 = CARTESIAN_POINT ( 'NONE',  ( 23.02499999999999858, 6.123233995736764310E-16, -4.999999999999998224 ) ) ;
#42177 = CARTESIAN_POINT ( 'NONE',  ( 9.001249775931846008E-16, 12.77187500061451786, 34.90005215228797653 ) ) ;
#42178 = VECTOR ( 'NONE', #11294, 1000.000000000000000 ) ;
#42179 = CARTESIAN_POINT ( 'NONE',  ( 24.78750000122903074, -4.330127018922194537, 2.499999999999995559 ) ) ;
#42180 = CARTESIAN_POINT ( 'NONE',  ( 19.35937500061451644, 4.119189519843966529, -2.378215178124998275 ) ) ;
#42181 = CARTESIAN_POINT ( 'NONE',  ( 13.52812500061451750, 4.541064518000418104, 2.621784821874999949 ) ) ;
#42182 = CARTESIAN_POINT ( 'NONE',  ( 11.03437500061451715, -4.541064518000419881, 2.621784821874995952 ) ) ;
#42183 = CARTESIAN_POINT ( 'NONE',  ( 9.684375000614517504, -4.541064518000419881, 2.621784821874995952 ) ) ;
#42184 = CARTESIAN_POINT ( 'NONE',  ( 17.10937500061451999, 4.541064518000418104, -2.621784821874998173 ) ) ;
#42185 = EDGE_LOOP ( 'NONE', ( #43886, #20286, #1218, #42963, #30431, #58938, #64976 ) ) ;
#42186 = CARTESIAN_POINT ( 'NONE',  ( 28.99687500061451573, -3.027376345333614438, 5.243569643749998122 ) ) ;
#42187 = CARTESIAN_POINT ( 'NONE',  ( 21.02812500061451573, 6.421520780324663323E-16, -5.243569643749999010 ) ) ;
#42188 =( BOUNDED_CURVE ( )  B_SPLINE_CURVE ( 2, ( #25447, #36529, #59049, #47990, #8454, #30989, #53522 ),
 .UNSPECIFIED., .F., .F. ) 
 B_SPLINE_CURVE_WITH_KNOTS ( ( 3, 2, 2, 3 ),
 ( 0.1583333333333333814, 0.1611111111111111771, 0.1638888888888889173, 0.1666666666666666852 ),
 .UNSPECIFIED. ) 
 CURVE ( )  GEOMETRIC_REPRESENTATION_ITEM ( )  RATIONAL_B_SPLINE_CURVE ( ( 0.9999999999999973355, 0.8660254037844413721, 1.000000000000000000, 0.8660254037844387076, 1.000000000000000000, 0.8660254037844373753, 1.000000000000001332 ) ) 
 REPRESENTATION_ITEM ( '' )  );
#42189 = CARTESIAN_POINT ( 'NONE',  ( 15.72187500061451892, 3.027376345333613106, -5.243569643749998122 ) ) ;
#42190 = CARTESIAN_POINT ( 'NONE',  ( 21.10312500061451502, 4.541064518000418104, -2.621784821874998173 ) ) ;
#42191 = CARTESIAN_POINT ( 'NONE',  ( -3.999999999999999112, 13.25000000000000178, 30.00000000000000000 ) ) ;
#42192 = CARTESIAN_POINT ( 'NONE',  ( 26.99062500061451431, 6.054752690667223547, 3.707466751127219781E-16 ) ) ;
#42193 = CARTESIAN_POINT ( 'NONE',  ( 8.137500001229033941, -4.330127018922194537, 2.499999999999995559 ) ) ;
#42194 = VERTEX_POINT ( 'NONE', #19318 ) ;
#42195 = CARTESIAN_POINT ( 'NONE',  ( 4.425000001229032698, 2.886751345948126879, 4.999999999999999112 ) ) ;
#42196 = CARTESIAN_POINT ( 'NONE',  ( 8.484601909799253346E-16, 17.41250000000000142, -25.38119784648299770 ) ) ;
#42197 = CARTESIAN_POINT ( 'NONE',  ( 25.53750000122903074, 4.330127018922191873, 2.499999999999999556 ) ) ;
#42198 = CARTESIAN_POINT ( 'NONE',  ( -4.000000000000000888, 20.80624999877096570, 32.30940107675850470 ) ) ;
#42199 = CARTESIAN_POINT ( 'NONE',  ( 7.396875000614519635, -3.027376345333614438, 5.243569643749998122 ) ) ;
#42200 = CARTESIAN_POINT ( 'NONE',  ( 23.25000000000000000, 0.000000000000000000, 4.999999999999998224 ) ) ;
#42201 = CARTESIAN_POINT ( 'NONE',  ( 15.29062500061451679, 6.054752690667223547, 3.707466751127219781E-16 ) ) ;
#42202 = CARTESIAN_POINT ( 'NONE',  ( 9.234375000614518214, -4.541064518000419881, 2.621784821874995952 ) ) ;
#42203 = CARTESIAN_POINT ( 'NONE',  ( 26.58750000122903145, -4.330127018922194537, 2.499999999999995559 ) ) ;
#42204 = CARTESIAN_POINT ( 'NONE',  ( 18.15937500061451715, 0.000000000000000000, 5.243569643749999010 ) ) ;
#42205 = CARTESIAN_POINT ( 'NONE',  ( 5.484375000614518214, 4.541064518000418104, 2.621784821874999949 ) ) ;
#42206 = DIRECTION ( 'NONE',  ( -0.000000000000000000, -1.000000000000000000, -0.000000000000000000 ) ) ;
#42207 = CARTESIAN_POINT ( 'NONE',  ( 5.465625000614517504, 3.027376345333611329, 5.243569643749999010 ) ) ;
#42208 = CARTESIAN_POINT ( 'NONE',  ( 18.40312500061451573, 4.541064518000418104, -2.621784821874998173 ) ) ;
#42209 = ORIENTED_EDGE ( 'NONE', *, *, #47090, .T. ) ;
#42210 = CARTESIAN_POINT ( 'NONE',  ( 13.00312500061451537, 4.541064518000418104, -2.621784821874998173 ) ) ;
#42211 = CARTESIAN_POINT ( 'NONE',  ( 4.837500001229035895, 4.330127018922191873, 2.499999999999999556 ) ) ;
#42212 = CARTESIAN_POINT ( 'NONE',  ( 11.87812500061451537, -4.541064518000419881, 2.621784821874995952 ) ) ;
#42213 = CARTESIAN_POINT ( 'NONE',  ( 22.09687500061451715, 5.492252693125287522, 3.363034840372157021E-16 ) ) ;
#42214 = CARTESIAN_POINT ( 'NONE',  ( 10.05000000000000071, 4.330127018922192761, -2.499999999999997780 ) ) ;
#42215 = CARTESIAN_POINT ( 'NONE',  ( 6.750000001229033764, -2.886751345948129988, 4.999999999999997335 ) ) ;
#42216 = CARTESIAN_POINT ( 'NONE',  ( 19.79999999999999716, -4.330127018922190985, -2.500000000000001332 ) ) ;
#42217 = CARTESIAN_POINT ( 'NONE',  ( 14.10937500061451644, 0.000000000000000000, 5.243569643749999010 ) ) ;
#42218 = CARTESIAN_POINT ( 'NONE',  ( 15.67500000122903181, 2.886751345948126879, 4.999999999999999112 ) ) ;
#42219 = CARTESIAN_POINT ( 'NONE',  ( 22.38749999999999929, -2.886751345948129988, 4.999999999999997335 ) ) ;
#42220 = CARTESIAN_POINT ( 'NONE',  ( -2.121784821874999949, 18.82812500061451644, -33.67503911421598417 ) ) ;
#42221 = DIRECTION ( 'NONE',  ( -0.000000000000000000, -1.000000000000000000, -0.000000000000000000 ) ) ;
#42222 = CARTESIAN_POINT ( 'NONE',  ( 1.999999999999998668, 15.01250000122903394, -33.46410161513775705 ) ) ;
#42223 = CYLINDRICAL_SURFACE ( 'NONE', #71363, 3.999999999999996447 ) ;
#42224 = CARTESIAN_POINT ( 'NONE',  ( 1.071796769724490339, 19.86740381056766225, 26.00000000000000355 ) ) ;
#42225 = CARTESIAN_POINT ( 'NONE',  ( 4.809916128174254624, -1.365542690628744449, -5.062639209831853115 ) ) ;
#42226 = CARTESIAN_POINT ( 'NONE',  ( 15.45937500061451608, 0.000000000000000000, 5.243569643749999010 ) ) ;
#42227 = CARTESIAN_POINT ( 'NONE',  ( 28.08749999999999858, 5.773502691896255534, 3.535250795749688894E-16 ) ) ;
#42228 = CARTESIAN_POINT ( 'NONE',  ( 10.90312500061451928, 0.000000000000000000, 5.243569643749999010 ) ) ;
#42229 = CARTESIAN_POINT ( 'NONE',  ( 28.58437500061451431, -2.746126346562642428, -4.756430356249999214 ) ) ;
#42230 = CARTESIAN_POINT ( 'NONE',  ( 22.92187500061451644, 3.027376345333613106, -5.243569643749998122 ) ) ;
#42231 = CARTESIAN_POINT ( 'NONE',  ( 15.98437500061451821, -2.746126346562641984, -4.756430356249999214 ) ) ;
#42232 = CARTESIAN_POINT ( 'NONE',  ( 9.403125000614517504, 4.541064518000418104, -2.621784821874998173 ) ) ;
#42233 = CARTESIAN_POINT ( 'NONE',  ( 15.08437500061451786, -4.541064518000419881, 2.621784821874995952 ) ) ;
#42234 = ORIENTED_EDGE ( 'NONE', *, *, #18001, .T. ) ;
#42235 = CARTESIAN_POINT ( 'NONE',  ( 27.08437500061451786, 4.541064518000418104, 2.621784821874999949 ) ) ;
#42236 = CARTESIAN_POINT ( 'NONE',  ( 26.95312500061451644, 4.541064518000418104, -2.621784821874998173 ) ) ;
#42237 = CARTESIAN_POINT ( 'NONE',  ( 28.34062500061451928, 6.054752690667223547, 3.707466751127219781E-16 ) ) ;
#42238 = EDGE_CURVE ( 'NONE', #63662, #23724, #53831, .T. ) ;
#42239 = CYLINDRICAL_SURFACE ( 'NONE', #37236, 4.000000000000000000 ) ;
#42240 = CARTESIAN_POINT ( 'NONE',  ( 7.950000000000001954, 0.000000000000000000, 4.999999999999998224 ) ) ;
#42241 = CARTESIAN_POINT ( 'NONE',  ( 16.87500000122903288, 2.886751345948129099, -4.999999999999998224 ) ) ;
#42242 = CARTESIAN_POINT ( 'NONE',  ( 16.59375000122903643, -2.886751345948074920, 5.000000000000092371 ) ) ;
#42243 = CARTESIAN_POINT ( 'NONE',  ( 8.109375000614516438, 2.746126346562643317, 4.756430356249998326 ) ) ;
#42244 = ORIENTED_EDGE ( 'NONE', *, *, #37713, .T. ) ;
#42245 = CARTESIAN_POINT ( 'NONE',  ( 14.55000000000000071, 4.330127018922192761, -2.499999999999997780 ) ) ;
#42246 = CARTESIAN_POINT ( 'NONE',  ( 19.42499999999999716, 6.123233995736764310E-16, -4.999999999999998224 ) ) ;
#42247 = CARTESIAN_POINT ( 'NONE',  ( 13.49062500061451608, 6.054752690667223547, 3.707466751127219781E-16 ) ) ;
#42248 = ORIENTED_EDGE ( 'NONE', *, *, #57822, .T. ) ;
#42249 = CARTESIAN_POINT ( 'NONE',  ( -5.810221930991193690E-16, 18.65000000122903501, -34.00000000000000000 ) ) ;
#42250 = CARTESIAN_POINT ( 'NONE',  ( 4.243569643749999898, 17.79687500061451999, -27.54997392385601529 ) ) ;
#42251 = CARTESIAN_POINT ( 'NONE',  ( 5.578125000614518214, -4.541064518000419881, 2.621784821874995952 ) ) ;
#42252 = CARTESIAN_POINT ( 'NONE',  ( 3.756430356249998770, 13.05312499938548321, 32.16877607737301759 ) ) ;
#42253 = CARTESIAN_POINT ( 'NONE',  ( 11.21250000000000036, -5.773502691896255534, -1.060575238724906372E-15 ) ) ;
#42254 = CARTESIAN_POINT ( 'NONE',  ( 28.69687500061451502, 4.119189519843966529, -2.378215178124998275 ) ) ;
#42255 = EDGE_LOOP ( 'NONE', ( #61343, #38989, #65273, #19082 ) ) ;
#42256 = CARTESIAN_POINT ( 'NONE',  ( 4.243569643749999898, 14.14062500061451644, 32.45002607614398471 ) ) ;
#42257 = CARTESIAN_POINT ( 'NONE',  ( 25.60312500061451502, 4.541064518000418104, -2.621784821874998173 ) ) ;
#42258 = CARTESIAN_POINT ( 'NONE',  ( 7.537500000000002309, -2.886751345948129988, 4.999999999999997335 ) ) ;
#42259 = CARTESIAN_POINT ( 'NONE',  ( -1.878215178124999163, 17.74062499938548498, 26.74683588394047007 ) ) ;
#42260 = CARTESIAN_POINT ( 'NONE',  ( 23.03437500061451715, 4.541064518000418104, 2.621784821874999949 ) ) ;
#42261 = CARTESIAN_POINT ( 'NONE',  ( 22.19062500061451715, -3.027376345333614438, 5.243569643749998122 ) ) ;
#42262 = CARTESIAN_POINT ( 'NONE',  ( 4.243569643749999898, 14.59062500061459744, -27.54997392385601529 ) ) ;
#42263 = CARTESIAN_POINT ( 'NONE',  ( 22.42500000122903359, 2.886751345948126879, 4.999999999999999112 ) ) ;
#42264 = CARTESIAN_POINT ( 'NONE',  ( 5.540625000614515905, -3.027376345333614438, 5.243569643749998122 ) ) ;
#42265 = CARTESIAN_POINT ( 'NONE',  ( 25.54687500061451644, -2.746126346562641984, -4.756430356249999214 ) ) ;
#42266 = CARTESIAN_POINT ( 'NONE',  ( 24.02812500061451573, -4.541064518000419881, 2.621784821874995952 ) ) ;
#42267 = CARTESIAN_POINT ( 'NONE',  ( 10.80937500061451928, 4.119189519843966529, -2.378215178124998275 ) ) ;
#42268 = CARTESIAN_POINT ( 'NONE',  ( -3.756430356250000102, 15.56562499938548427, 30.00000000000000000 ) ) ;
#42269 = CARTESIAN_POINT ( 'NONE',  ( 16.69687500061451502, 6.054752690667223547, 3.707466751127219781E-16 ) ) ;
#42270 = CARTESIAN_POINT ( 'NONE',  ( 25.73437500061451644, 4.541064518000418104, 2.621784821874999949 ) ) ;
#42271 = CARTESIAN_POINT ( 'NONE',  ( -2.121784821874999949, 14.38437500061451679, 26.32496088578401938 ) ) ;
#42272 = CARTESIAN_POINT ( 'NONE',  ( 6.253125000614517148, 4.541064518000418104, -2.621784821874998173 ) ) ;
#42273 = CARTESIAN_POINT ( 'NONE',  ( 29.05312500061451431, -4.541064518000417216, -2.621784821875001281 ) ) ;
#42274 = CARTESIAN_POINT ( 'NONE',  ( 29.31562500061451715, 3.027376345333611329, 5.243569643749999010 ) ) ;
#42275 = CARTESIAN_POINT ( 'NONE',  ( -1.071796769724496334, 14.88259618943233598, 26.00000000000000355 ) ) ;
#42276 = CARTESIAN_POINT ( 'NONE',  ( 3.286795329855858760, 3.767887532774327308, -3.286795329856085690 ) ) ;
#42277 = CARTESIAN_POINT ( 'NONE',  ( 29.32500000122903216, -5.773502691896255534, -1.060575238724906372E-15 ) ) ;
#42278 = CARTESIAN_POINT ( 'NONE',  ( 8.259375000614518569, 0.000000000000000000, 5.243569643749999010 ) ) ;
#42279 = CARTESIAN_POINT ( 'NONE',  ( 14.47500000122903430, -5.773502691896255534, -1.060575238724906372E-15 ) ) ;
#42280 = CARTESIAN_POINT ( 'NONE',  ( 2.971875000614517592, -6.054752690667223547, -1.112240025338166033E-15 ) ) ;
#42281 = CARTESIAN_POINT ( 'NONE',  ( 12.37500000122903465, 2.886751345948129099, -4.999999999999998224 ) ) ;
#42282 = CARTESIAN_POINT ( 'NONE',  ( 4.078125000614517326, 4.541064518000418104, 2.621784821874999949 ) ) ;
#42283 = CARTESIAN_POINT ( 'NONE',  ( 2.828200636599751609E-16, 13.45624999877096606, 25.38119784648299415 ) ) ;
#42284 = CARTESIAN_POINT ( 'NONE',  ( 21.05625000122903145, 0.000000000000000000, 4.999999999999998224 ) ) ;
#42285 = CARTESIAN_POINT ( 'NONE',  ( 15.42187500061451821, 3.027376345333611329, 5.243569643749999010 ) ) ;
#42286 = CARTESIAN_POINT ( 'NONE',  ( 5.000000000000000000, 6.123233995736766282E-16, -50.00000000000000000 ) ) ;
#42287 = ORIENTED_EDGE ( 'NONE', *, *, #7766, .F. ) ;
#42288 = CARTESIAN_POINT ( 'NONE',  ( 22.07812500061451644, 4.541064518000418104, 2.621784821874999949 ) ) ;
#42289 = CARTESIAN_POINT ( 'NONE',  ( 8.390625000614518214, -3.027376345333610441, -5.243569643749999898 ) ) ;
#42290 = CARTESIAN_POINT ( 'NONE',  ( 24.57187500061451502, -6.054752690667223547, -1.112240025338166033E-15 ) ) ;
#42291 = CARTESIAN_POINT ( 'NONE',  ( 7.640625000614517326, 6.054752690667223547, 3.707466751127219781E-16 ) ) ;
#42292 = CARTESIAN_POINT ( 'NONE',  ( 30.00000000000000000, 0.000000000000000000, 0.000000000000000000 ) ) ;
#42293 = CARTESIAN_POINT ( 'NONE',  ( 8.400000001229035007, 5.773502691896255534, 3.535250795749688894E-16 ) ) ;
#42294 = CARTESIAN_POINT ( 'NONE',  ( 24.47812500061451502, -4.541064518000419881, 2.621784821874995952 ) ) ;
#42295 = CARTESIAN_POINT ( 'NONE',  ( 2.000000000000001332, 19.36250000122903359, -26.53589838486224650 ) ) ;
#42296 = CARTESIAN_POINT ( 'NONE',  ( 9.375000001229036428, 2.886751345948126879, 4.999999999999999112 ) ) ;
#42297 = CARTESIAN_POINT ( 'NONE',  ( 18.66562500061451146, -6.054752690667223547, -1.112240025338166033E-15 ) ) ;
#42298 = CARTESIAN_POINT ( 'NONE',  ( 17.84062500061451573, -3.027376345333610441, -5.243569643749999898 ) ) ;
#42299 = CARTESIAN_POINT ( 'NONE',  ( 29.52187500061451431, -5.492252693125287522, -1.008910452111647106E-15 ) ) ;
#42300 = CARTESIAN_POINT ( 'NONE',  ( 17.55000000000000071, -4.330127018922190985, -2.500000000000001332 ) ) ;
#42301 = CARTESIAN_POINT ( 'NONE',  ( 13.65000000122903323, -2.886751345948125991, -5.000000000000000000 ) ) ;
#42302 = CARTESIAN_POINT ( 'NONE',  ( 10.00312500061451715, 0.000000000000000000, 5.243569643749999010 ) ) ;
#42303 = CARTESIAN_POINT ( 'NONE',  ( 13.75312500061451715, -4.541064518000417216, -2.621784821875001281 ) ) ;
#42304 = EDGE_CURVE ( 'NONE', #12333, #72145, #27949, .T. ) ;
#42305 = CARTESIAN_POINT ( 'NONE',  ( 23.21250000122903501, 4.330127018922192761, -2.499999999999997780 ) ) ;
#42306 = CARTESIAN_POINT ( 'NONE',  ( 21.27187500061451786, 3.027376345333611329, 5.243569643749999010 ) ) ;
#42307 = CARTESIAN_POINT ( 'NONE',  ( 21.23437500061451644, 4.541064518000418104, 2.621784821874999949 ) ) ;
#42308 = LINE ( 'NONE', #70381, #64216 ) ;
#42309 = EDGE_CURVE ( 'NONE', #18463, #7096, #68869, .T. ) ;
#42310 = CARTESIAN_POINT ( 'NONE',  ( 8.062500001229034652, 0.000000000000000000, 4.999999999999998224 ) ) ;
#42311 = CARTESIAN_POINT ( 'NONE',  ( 7.659375000614518036, 4.541064518000418104, -2.621784821874998173 ) ) ;
#42312 = CARTESIAN_POINT ( 'NONE',  ( 23.40937500061451715, 4.541064518000418104, -2.621784821874998173 ) ) ;
#42313 = EDGE_CURVE ( 'NONE', #26824, #41179, #30788, .T. ) ;
#42314 = CARTESIAN_POINT ( 'NONE',  ( -1.071796769724490561, 12.63259618943233598, 26.00000000000000000 ) ) ;
#42315 = CARTESIAN_POINT ( 'NONE',  ( 18.02812500061451573, 4.541064518000418104, 2.621784821874999949 ) ) ;
#42316 = CARTESIAN_POINT ( 'NONE',  ( 24.53437500061451715, -4.541064518000419881, 2.621784821874995952 ) ) ;
#42317 = CARTESIAN_POINT ( 'NONE',  ( 1.878215178125000495, 20.02812499938548285, 26.74683588394047007 ) ) ;
#42318 = FACE_OUTER_BOUND ( 'NONE', #6816, .T. ) ;
#42319 = CARTESIAN_POINT ( 'NONE',  ( 16.40625000122903643, 4.330127018922192761, -2.499999999999997780 ) ) ;
#42320 = CARTESIAN_POINT ( 'NONE',  ( 5.596875000614516260, -3.027376345333614438, 5.243569643749998122 ) ) ;
#42321 = CARTESIAN_POINT ( 'NONE',  ( 18.36562500061451431, 3.027376345333613106, -5.243569643749998122 ) ) ;
#42322 = VERTEX_POINT ( 'NONE', #23783 ) ;
#42323 = CARTESIAN_POINT ( 'NONE',  ( 25.16250000000000142, -5.773502691896255534, -1.060575238724906372E-15 ) ) ;
#42324 = CARTESIAN_POINT ( 'NONE',  ( 24.70312500061451644, 4.541064518000418104, -2.621784821874998173 ) ) ;
#42325 = FACE_OUTER_BOUND ( 'NONE', #15658, .T. ) ;
#42326 = CARTESIAN_POINT ( 'NONE',  ( 27.97500000000000142, 6.123233995736764310E-16, -4.999999999999998224 ) ) ;
#42327 = CARTESIAN_POINT ( 'NONE',  ( 14.92500000000000071, 6.123233995736764310E-16, -4.999999999999998224 ) ) ;
#42328 = CARTESIAN_POINT ( 'NONE',  ( 25.46250000122903501, 4.330127018922192761, -2.499999999999997780 ) ) ;
#42329 = CARTESIAN_POINT ( 'NONE',  ( 20.12812500061451715, 6.421520780324663323E-16, -5.243569643749999010 ) ) ;
#42330 = VERTEX_POINT ( 'NONE', #69235 ) ;
#42331 = CARTESIAN_POINT ( 'NONE',  ( 22.53750000000000142, -2.886751345948125991, -5.000000000000000000 ) ) ;
#42332 =( BOUNDED_CURVE ( )  B_SPLINE_CURVE ( 3, ( #52301, #13481, #46042, #29412 ),
 .UNSPECIFIED., .F., .F. ) 
 B_SPLINE_CURVE_WITH_KNOTS ( ( 4, 4 ),
 ( 1.570796326794896780, 3.141592653589793116 ),
 .UNSPECIFIED. ) 
 CURVE ( )  GEOMETRIC_REPRESENTATION_ITEM ( )  RATIONAL_B_SPLINE_CURVE ( ( 1.000000000000000000, 0.8047378541243650485, 0.8047378541243650485, 1.000000000000000000 ) ) 
 REPRESENTATION_ITEM ( '' )  );
#42333 = CARTESIAN_POINT ( 'NONE',  ( 24.94687500061451502, -3.027376345333614438, 5.243569643749998122 ) ) ;
#42334 = ORIENTED_EDGE ( 'NONE', *, *, #12948, .T. ) ;
#42335 = B_SPLINE_CURVE_WITH_KNOTS ( 'NONE', 3,
 ( #9337, #3804, #64745, #31129, #65111, #59190, #26327, #8600, #20402, #53670 ),
 .UNSPECIFIED., .F., .F.,
 ( 4, 3, 3, 4 ),
 ( 0.000000000000000000, 2.812505701543726881E-05, 5.625011473905447835E-05, 9.076251227131168335E-05 ),
 .UNSPECIFIED. ) ;
#42336 = CARTESIAN_POINT ( 'NONE',  ( 11.62500000000000000, -4.330127018922194537, 2.499999999999995559 ) ) ;
#42337 = CARTESIAN_POINT ( 'NONE',  ( 13.26562500061451644, -6.054752690667223547, -1.112240025338166033E-15 ) ) ;
#42338 = CARTESIAN_POINT ( 'NONE',  ( 4.303125000614516971, -4.541064518000417216, -2.621784821875001281 ) ) ;
#42339 = CARTESIAN_POINT ( 'NONE',  ( 17.33437500061451431, -2.746126346562642428, -4.756430356249999214 ) ) ;
#42340 = CARTESIAN_POINT ( 'NONE',  ( 3.346875000614518036, -3.027376345333614438, 5.243569643749998122 ) ) ;
#42341 = CARTESIAN_POINT ( 'NONE',  ( 13.05000000122903536, -2.886751345948129988, 4.999999999999997335 ) ) ;
#42342 = CARTESIAN_POINT ( 'NONE',  ( 18.52499999999999858, 6.123233995736764310E-16, -4.999999999999998224 ) ) ;
#42343 = CARTESIAN_POINT ( 'NONE',  ( 27.89999999999999858, -4.330127018922190985, -2.500000000000001332 ) ) ;
#42344 = CARTESIAN_POINT ( 'NONE',  ( 5.810221930991193690E-16, 14.35624999877096464, 26.00000000000000000 ) ) ;
#42345 = CARTESIAN_POINT ( 'NONE',  ( 6.796875000614516438, 6.054752690667223547, 3.707466751127219781E-16 ) ) ;
#42346 = CARTESIAN_POINT ( 'NONE',  ( 20.10937500061451289, -4.541064518000417216, -2.621784821875001281 ) ) ;
#42347 = CARTESIAN_POINT ( 'NONE',  ( -2.000000000000000000, 13.73750000122903359, 26.53589838486224650 ) ) ;
#42348 = ORIENTED_EDGE ( 'NONE', *, *, #33365, .T. ) ;
#42349 = CARTESIAN_POINT ( 'NONE',  ( 29.39062500061451289, -3.027376345333614438, 5.243569643749998122 ) ) ;
#42350 = CARTESIAN_POINT ( 'NONE',  ( 3.712499999999999911, 2.886751345948129099, -4.999999999999998224 ) ) ;
#42352 = ADVANCED_FACE ( 'NONE', ( #58118 ), #13412, .F. ) ;
#42351 = CARTESIAN_POINT ( 'NONE',  ( 4.509375000614518569, 4.541064518000418104, -2.621784821874998173 ) ) ;
#42353 = CARTESIAN_POINT ( 'NONE',  ( 15.37500000000000000, 6.123233995736764310E-16, -4.999999999999998224 ) ) ;
#42354 = CARTESIAN_POINT ( 'NONE',  ( 14.24062500061451608, -3.027376345333610441, -5.243569643749999898 ) ) ;
#42355 = CARTESIAN_POINT ( 'NONE',  ( 26.00625000122903074, 0.000000000000000000, 4.999999999999998224 ) ) ;
#42356 = LINE ( 'NONE', #25727, #24214 ) ;
#42357 = CARTESIAN_POINT ( 'NONE',  ( 14.08125000122903181, 6.123233995736764310E-16, -4.999999999999998224 ) ) ;
#42358 = CARTESIAN_POINT ( 'NONE',  ( 17.51250000122903216, 0.000000000000000000, 4.999999999999998224 ) ) ;
#42359 = DIRECTION ( 'NONE',  ( -0.000000000000000000, -1.000000000000000000, -0.000000000000000000 ) ) ;
#42360 = CARTESIAN_POINT ( 'NONE',  ( 16.50937500061451502, -4.119189519843965641, -2.378215178125001383 ) ) ;
#42361 = CARTESIAN_POINT ( 'NONE',  ( 8.653125000614515727, 0.000000000000000000, 5.243569643749999010 ) ) ;
#42362 = CARTESIAN_POINT ( 'NONE',  ( 23.48437500061451644, 4.541064518000418104, 2.621784821874999949 ) ) ;
#42363 = CARTESIAN_POINT ( 'NONE',  ( -4.243569643749999898, 18.05937500061451928, 30.00000000000000000 ) ) ;
#42364 = CARTESIAN_POINT ( 'NONE',  ( 23.29687500061451644, -3.027376345333610441, -5.243569643749999898 ) ) ;
#42365 = CARTESIAN_POINT ( 'NONE',  ( 4.387500000000002842, -2.886751345948129988, 4.999999999999997335 ) ) ;
#42366 = CARTESIAN_POINT ( 'NONE',  ( 3.999999999999998668, 10.02500000122903501, 27.69059892324149175 ) ) ;
#42367 = CARTESIAN_POINT ( 'NONE',  ( 13.49062500061451608, 6.054752690667223547, 3.707466751127219781E-16 ) ) ;
#42368 = CARTESIAN_POINT ( 'NONE',  ( 3.450000001229036162, 5.773502691896255534, 3.535250795749688894E-16 ) ) ;
#42369 = CARTESIAN_POINT ( 'NONE',  ( 8.934375000614517504, 6.421520780324663323E-16, -5.243569643749999010 ) ) ;
#42370 = CARTESIAN_POINT ( 'NONE',  ( 45.00000000000000000, 6.123233995736764310E-16, -4.999999999999998224 ) ) ;
#42371 = ORIENTED_EDGE ( 'NONE', *, *, #66440, .T. ) ;
#42372 = CARTESIAN_POINT ( 'NONE',  ( 11.16562500061451679, 3.027376345333613106, -5.243569643749998122 ) ) ;
#42373 = CARTESIAN_POINT ( 'NONE',  ( 15.57187500061451679, -6.054752690667223547, -1.112240025338166033E-15 ) ) ;
#42374 = DIRECTION ( 'NONE',  ( -1.000000000000000000, -0.000000000000000000, -0.000000000000000000 ) ) ;
#42375 = CARTESIAN_POINT ( 'NONE',  ( 24.67500000122903359, 2.886751345948126879, 4.999999999999999112 ) ) ;
#42376 = CARTESIAN_POINT ( 'NONE',  ( 9.346875000614517148, -3.027376345333610441, -5.243569643749999898 ) ) ;
#42377 = CARTESIAN_POINT ( 'NONE',  ( 11.12812500061451715, 6.421520780324663323E-16, -5.243569643749999010 ) ) ;
#42378 = CARTESIAN_POINT ( 'NONE',  ( 27.43125000122903145, -4.330127018922194537, 2.499999999999995559 ) ) ;
#42379 = CARTESIAN_POINT ( 'NONE',  ( 21.90937500061451715, -4.541064518000417216, -2.621784821875001281 ) ) ;
#42380 = FACE_OUTER_BOUND ( 'NONE', #308, .T. ) ;
#42381 = CARTESIAN_POINT ( 'NONE',  ( 5.475000000000000533, 6.123233995736764310E-16, -4.999999999999998224 ) ) ;
#42382 = CARTESIAN_POINT ( 'NONE',  ( 45.00000000000000000, 0.000000000000000000, 0.000000000000000000 ) ) ;
#42383 = CARTESIAN_POINT ( 'NONE',  ( 2.121784821875001281, 15.50937500061451857, -26.32496088578401938 ) ) ;
#42384 = CARTESIAN_POINT ( 'NONE',  ( 15.90937500061451892, 0.000000000000000000, 5.243569643749999010 ) ) ;
#42385 = CARTESIAN_POINT ( 'NONE',  ( 16.57500000122903216, 2.886751345948126879, 4.999999999999999112 ) ) ;
#42386 = CARTESIAN_POINT ( 'NONE',  ( 11.22187500061451892, 3.027376345333613106, -5.243569643749998122 ) ) ;
#42387 = CARTESIAN_POINT ( 'NONE',  ( 2.121784821875001281, 17.70312500061451644, -26.32496088578401938 ) ) ;
#42388 = CARTESIAN_POINT ( 'NONE',  ( 16.72500000122903430, -5.773502691896255534, -1.060575238724906372E-15 ) ) ;
#42389 = CARTESIAN_POINT ( 'NONE',  ( 11.84062500061451750, -3.027376345333614438, 5.243569643749998122 ) ) ;
#42390 = VERTEX_POINT ( 'NONE', #1274 ) ;
#42391 = CARTESIAN_POINT ( 'NONE',  ( 15.11249999999999893, 2.886751345948126879, 4.999999999999999112 ) ) ;
#42392 = CARTESIAN_POINT ( 'NONE',  ( 5.062500001229035540, -4.330127018922190985, -2.500000000000001332 ) ) ;
#42393 = CARTESIAN_POINT ( 'NONE',  ( 10.32187500061451679, 3.027376345333612662, -5.243569643749998122 ) ) ;
#42394 = CARTESIAN_POINT ( 'NONE',  ( 4.060897850599462622, 2.917037649225213247, 4.254917590412954809 ) ) ;
#42395 = CARTESIAN_POINT ( 'NONE',  ( 12.75000000122903643, -2.886751345948125991, -5.000000000000000000 ) ) ;
#42396 = CARTESIAN_POINT ( 'NONE',  ( 21.75000000122903288, -2.886751345948125991, -5.000000000000000000 ) ) ;
#42397 = CARTESIAN_POINT ( 'NONE',  ( 16.79062500061451857, -3.027376345333614438, 5.243569643749998122 ) ) ;
#42398 = CARTESIAN_POINT ( 'NONE',  ( 20.20312500061451644, 4.541064518000418104, -2.621784821874998173 ) ) ;
#42399 = CARTESIAN_POINT ( 'NONE',  ( 27.52500000122903145, -5.773502691896255534, -1.060575238724906372E-15 ) ) ;
#42400 =( BOUNDED_CURVE ( )  B_SPLINE_CURVE ( 2, ( #60872, #5822, #10275, #32807, #55345, #4739, #27273 ),
 .UNSPECIFIED., .F., .F. ) 
 B_SPLINE_CURVE_WITH_KNOTS ( ( 3, 2, 2, 3 ),
 ( 0.1400000000000000133, 0.1433333333333333404, 0.1466666666666666674, 0.1499999999999999944 ),
 .UNSPECIFIED. ) 
 CURVE ( )  GEOMETRIC_REPRESENTATION_ITEM ( )  RATIONAL_B_SPLINE_CURVE ( ( 1.000000000000000000, 0.8660254037844387076, 1.000000000000000000, 0.8660254037844387076, 1.000000000000000000, 0.8660254037844387076, 1.000000000000000000 ) ) 
 REPRESENTATION_ITEM ( '' )  );
#42401 = CARTESIAN_POINT ( 'NONE',  ( 25.61250000000000071, -5.773502691896255534, -1.060575238724906372E-15 ) ) ;
#42402 = DIRECTION ( 'NONE',  ( 0.000000000000000000, 0.000000000000000000, -1.000000000000000000 ) ) ;
#42403 = CARTESIAN_POINT ( 'NONE',  ( 28.87499999999999645, 6.123233995736764310E-16, -4.999999999999998224 ) ) ;
#42404 = CARTESIAN_POINT ( 'NONE',  ( 27.90937500061451715, 4.541064518000418104, -2.621784821874998173 ) ) ;
#42405 = CARTESIAN_POINT ( 'NONE',  ( 45.00000000000000000, -2.499999999999999556, -5.500000000000000000 ) ) ;
#42406 = CARTESIAN_POINT ( 'NONE',  ( -3.000416591977282496E-16, 13.89687500061451786, -34.90005215228797653 ) ) ;
#42407 = CARTESIAN_POINT ( 'NONE',  ( 4.762500001229033941, 4.330127018922192761, -2.499999999999997780 ) ) ;
#42408 = CARTESIAN_POINT ( 'NONE',  ( 4.500000000000000888, -4.330127018922190985, -2.500000000000001332 ) ) ;
#42409 = EDGE_CURVE ( 'NONE', #30305, #2861, #66115, .T. ) ;
#42410 = ADVANCED_FACE ( 'NONE', ( #46335 ), #69592, .T. ) ;
#42411 = CARTESIAN_POINT ( 'NONE',  ( 3.021917804904423743, -3.983467431823952687, -3.409840147052992432 ) ) ;
#42412 = CARTESIAN_POINT ( 'NONE',  ( 6.534375000614517148, -4.541064518000419881, 2.621784821874995952 ) ) ;
#42413 = CARTESIAN_POINT ( 'NONE',  ( 27.40312500061451573, 4.541064518000418104, -2.621784821874998173 ) ) ;
#42414 = DIRECTION ( 'NONE',  ( -0.000000000000000000, -1.000000000000000000, -0.000000000000000000 ) ) ;
#42415 = CARTESIAN_POINT ( 'NONE',  ( 5.625000000000001776, 4.330127018922191873, 2.499999999999999556 ) ) ;
#42416 = LINE ( 'NONE', #63836, #17047 ) ;
#42417 = CARTESIAN_POINT ( 'NONE',  ( 6.121875000614517504, -6.054752690667223547, -1.112240025338166033E-15 ) ) ;
#42418 = CARTESIAN_POINT ( 'NONE',  ( 11.74687500061451573, 6.054752690667223547, 3.707466751127219781E-16 ) ) ;
#42419 = CARTESIAN_POINT ( 'NONE',  ( 3.750000000000000000, 4.330127018922192761, -2.499999999999997780 ) ) ;
#42420 = CARTESIAN_POINT ( 'NONE',  ( 9.001249775931846008E-16, 15.86562500061459602, 34.90005215228797653 ) ) ;
#42421 = CARTESIAN_POINT ( 'NONE',  ( 1.626862140677534273E-15, 17.86250000000000071, 34.00000000000000000 ) ) ;
#42422 = CARTESIAN_POINT ( 'NONE',  ( 5.924999999999999822, 6.123233995736764310E-16, -4.999999999999998224 ) ) ;
#42423 = CARTESIAN_POINT ( 'NONE',  ( 14.63437500061451502, -2.746126346562642428, -4.756430356249999214 ) ) ;
#42424 = CARTESIAN_POINT ( 'NONE',  ( 20.80312500061451431, 0.000000000000000000, 5.243569643749999010 ) ) ;
#42425 = CARTESIAN_POINT ( 'NONE',  ( 9.890625000614516438, 6.054752690667223547, 3.707466751127219781E-16 ) ) ;
#42426 = CARTESIAN_POINT ( 'NONE',  ( 23.97187500061451715, -4.119189519843968306, 2.378215178124996054 ) ) ;
#42427 = CARTESIAN_POINT ( 'NONE',  ( 10.35937500061451644, 4.541064518000418104, -2.621784821874998173 ) ) ;
#42428 = CARTESIAN_POINT ( 'NONE',  ( 26.02499999999999858, -4.330127018922194537, 2.499999999999995559 ) ) ;
#42429 = CARTESIAN_POINT ( 'NONE',  ( 20.88750000122903572, 6.123233995736764310E-16, -4.999999999999998224 ) ) ;
#42430 = CARTESIAN_POINT ( 'NONE',  ( 28.64062500061451289, -3.027376345333610441, -5.243569643749999898 ) ) ;
#42431 = CARTESIAN_POINT ( 'NONE',  ( 15.45000000000000107, 4.330127018922192761, -2.499999999999997780 ) ) ;
#42432 = CARTESIAN_POINT ( 'NONE',  ( 10.39687500061451786, 6.054752690667223547, 3.707466751127219781E-16 ) ) ;
#42433 = CARTESIAN_POINT ( 'NONE',  ( 15.04687500061451644, -3.027376345333614438, 5.243569643749998122 ) ) ;
#42434 = CARTESIAN_POINT ( 'NONE',  ( 26.25937500061451857, 0.000000000000000000, 5.243569643749999010 ) ) ;
#42435 = CARTESIAN_POINT ( 'NONE',  ( 23.64375000122903359, 5.773502691896255534, 3.535250795749688401E-16 ) ) ;
#42436 = CARTESIAN_POINT ( 'NONE',  ( 13.76250000000000107, 2.886751345948126879, 4.999999999999999112 ) ) ;
#42437 = CARTESIAN_POINT ( 'NONE',  ( 19.09687500061451360, -3.027376345333614438, 5.243569643749998122 ) ) ;
#42438 = CARTESIAN_POINT ( 'NONE',  ( 11.33437500061451608, 4.541064518000418104, 2.621784821874999949 ) ) ;
#42439 = CARTESIAN_POINT ( 'NONE',  ( 3.756430356249998770, 13.50312499938548250, 32.16877607737302469 ) ) ;
#42440 = CARTESIAN_POINT ( 'NONE',  ( 23.25000000000000000, 0.000000000000000000, 4.999999999999998224 ) ) ;
#42441 = CARTESIAN_POINT ( 'NONE',  ( -4.000000000000000000, 14.07500000000000107, 30.00000000000000000 ) ) ;
#42442 = CARTESIAN_POINT ( 'NONE',  ( -4.243569643749997233, 13.14687500061451786, -27.54997392385601174 ) ) ;
#42443 = CARTESIAN_POINT ( 'NONE',  ( 25.43437500061451573, -4.119189519843968306, 2.378215178124996054 ) ) ;
#42444 = CARTESIAN_POINT ( 'NONE',  ( 13.97812500061451679, 4.541064518000418104, 2.621784821874999949 ) ) ;
#42445 = CARTESIAN_POINT ( 'NONE',  ( 4.987500000000002487, -2.886751345948125991, -5.000000000000000000 ) ) ;
#42446 = CARTESIAN_POINT ( 'NONE',  ( 1.626862140677534273E-15, 13.92500000122903181, -26.00000000000000355 ) ) ;
#42447 = CARTESIAN_POINT ( 'NONE',  ( 45.00000000000000000, 0.000000000000000000, 0.000000000000000000 ) ) ;
#42448 = CARTESIAN_POINT ( 'NONE',  ( 12.86250000000000071, 2.886751345948126879, 4.999999999999999112 ) ) ;
#42449 = CARTESIAN_POINT ( 'NONE',  ( -3.999999999999997335, 18.35000000122903430, 32.30940107675850470 ) ) ;
#42450 = CARTESIAN_POINT ( 'NONE',  ( 12.67500000122903536, -5.773502691896255534, -1.060575238724906372E-15 ) ) ;
#42451 = CARTESIAN_POINT ( 'NONE',  ( 22.77187500061451786, -6.054752690667223547, -1.112240025338166033E-15 ) ) ;
#42452 = CARTESIAN_POINT ( 'NONE',  ( 15.57187500061451679, -6.054752690667223547, -1.112240025338166033E-15 ) ) ;
#42453 = ORIENTED_EDGE ( 'NONE', *, *, #40242, .F. ) ;
#42454 = CARTESIAN_POINT ( 'NONE',  ( 18.47812500061451857, 4.541064518000418104, 2.621784821874999949 ) ) ;
#42455 = CARTESIAN_POINT ( 'NONE',  ( 5.053125000614517859, 0.000000000000000000, 5.243569643749999010 ) ) ;
#42456 = CARTESIAN_POINT ( 'NONE',  ( 16.54687500061451644, -3.027376345333610441, -5.243569643749999898 ) ) ;
#42457 = CARTESIAN_POINT ( 'NONE',  ( 29.44687500061451857, -3.027376345333614438, 5.243569643749998122 ) ) ;
#42458 = CARTESIAN_POINT ( 'NONE',  ( 4.903125000614516615, 4.541064518000418104, -2.621784821874998173 ) ) ;
#42459 = CARTESIAN_POINT ( 'NONE',  ( 20.35312500061451502, 0.000000000000000000, 5.243569643749999010 ) ) ;
#42460 = ADVANCED_FACE ( 'NONE', ( #47780 ), #12703, .T. ) ;
#42461 = CARTESIAN_POINT ( 'NONE',  ( -3.000416591977282496E-16, 15.19062500061451715, 25.09994784771203058 ) ) ;
#42462 = CARTESIAN_POINT ( 'NONE',  ( 16.53750000122903430, 4.330127018922191873, 2.499999999999999556 ) ) ;
#42463 = CARTESIAN_POINT ( 'NONE',  ( 11.82187500061451857, 2.746126346562643317, 4.756430356249998326 ) ) ;
#42464 = CARTESIAN_POINT ( 'NONE',  ( 6.703125000614516438, 4.541064518000418104, -2.621784821874998173 ) ) ;
#42465 = CARTESIAN_POINT ( 'NONE',  ( 29.20312500061451644, 4.541064518000418104, -2.621784821874998173 ) ) ;
#42466 = DIRECTION ( 'NONE',  ( 0.000000000000000000, 0.000000000000000000, -1.000000000000000000 ) ) ;
#42467 = CARTESIAN_POINT ( 'NONE',  ( 23.93437500061451573, 4.541064518000418104, 2.621784821874999949 ) ) ;
#42468 = CARTESIAN_POINT ( 'NONE',  ( 15.44062500061451537, -3.027376345333614438, 5.243569643749998122 ) ) ;
#42469 = CARTESIAN_POINT ( 'NONE',  ( 24.78750000122903074, -4.330127018922194537, 2.499999999999995559 ) ) ;
#42470 = CARTESIAN_POINT ( 'NONE',  ( 22.49062500061451431, 6.054752690667223547, 3.707466751127219781E-16 ) ) ;
#42471 = CARTESIAN_POINT ( 'NONE',  ( 20.25937500061451857, 4.541064518000418104, -2.621784821874998173 ) ) ;
#42472 = CARTESIAN_POINT ( 'NONE',  ( 13.82812500061451466, 6.421520780324663323E-16, -5.243569643749999010 ) ) ;
#42473 = CARTESIAN_POINT ( 'NONE',  ( -4.243569643749997233, 15.84687500061451715, 32.45002607614398471 ) ) ;
#42474 = CARTESIAN_POINT ( 'NONE',  ( 20.24062500061451431, 6.054752690667223547, 3.707466751127219781E-16 ) ) ;
#42475 = CARTESIAN_POINT ( 'NONE',  ( 28.82812500061451644, 4.541064518000418104, 2.621784821874999949 ) ) ;
#42476 = VERTEX_POINT ( 'NONE', #35961 ) ;
#42477 = EDGE_LOOP ( 'NONE', ( #8484, #41067, #62963, #59625, #48280, #7769, #46457 ) ) ;
#42478 = CARTESIAN_POINT ( 'NONE',  ( 23.88749999999999929, -2.886751345948125991, -5.000000000000000000 ) ) ;
#42479 = CARTESIAN_POINT ( 'NONE',  ( 4.243569643749999898, 19.59687500061452070, -27.54997392385601529 ) ) ;
#42480 = FACE_OUTER_BOUND ( 'NONE', #43360, .T. ) ;
#42481 = CARTESIAN_POINT ( 'NONE',  ( 27.10312500061451502, 0.000000000000000000, 5.243569643749999010 ) ) ;
#42482 = CARTESIAN_POINT ( 'NONE',  ( 8.390625000614518214, -3.027376345333610441, -5.243569643749999898 ) ) ;
#42483 = CARTESIAN_POINT ( 'NONE',  ( 19.38750000122903216, -4.330127018922194537, 2.499999999999995559 ) ) ;
#42484 = CARTESIAN_POINT ( 'NONE',  ( 25.04062500061451502, -3.027376345333610441, -5.243569643749999898 ) ) ;
#42485 = CARTESIAN_POINT ( 'NONE',  ( 26.06250000000000000, -5.773502691896255534, -1.060575238724906372E-15 ) ) ;
#42486 = CARTESIAN_POINT ( 'NONE',  ( 27.21562500061451928, -6.054752690667223547, -1.112240025338166033E-15 ) ) ;
#42487 = CARTESIAN_POINT ( 'NONE',  ( 8.915625000614515017, 3.027376345333613106, -5.243569643749998122 ) ) ;
#42488 = ORIENTED_EDGE ( 'NONE', *, *, #50295, .T. ) ;
#42489 = CARTESIAN_POINT ( 'NONE',  ( 22.45312500061451644, 4.541064518000418104, -2.621784821874998173 ) ) ;
#42490 = CARTESIAN_POINT ( 'NONE',  ( 4.228125000614517681, -4.541064518000419881, 2.621784821874995952 ) ) ;
#42491 = UNCERTAINTY_MEASURE_WITH_UNIT (LENGTH_MEASURE( 1.000000000000000082E-05 ), #50473, 'distance_accuracy_value', 'NONE');
#42492 = CARTESIAN_POINT ( 'NONE',  ( 14.97187500061451892, 2.746126346562643317, 4.756430356249998326 ) ) ;
#42493 = CARTESIAN_POINT ( 'NONE',  ( 1.999999999999998668, 13.10000000000000142, 26.53589838486224650 ) ) ;
#42494 = CARTESIAN_POINT ( 'NONE',  ( 4.000000000000000000, 12.89374999877096606, 30.00000000000000000 ) ) ;
#42495 = CARTESIAN_POINT ( 'NONE',  ( 10.91250000000000320, 2.886751345948129099, -4.999999999999998224 ) ) ;
#42496 = CARTESIAN_POINT ( 'NONE',  ( 11.18437500061451928, 6.421520780324663323E-16, -5.243569643749999010 ) ) ;
#42497 = CARTESIAN_POINT ( 'NONE',  ( 8.137500001229033941, -4.330127018922194537, 2.499999999999995559 ) ) ;
#42498 = CARTESIAN_POINT ( 'NONE',  ( 14.70937500061451786, -4.541064518000417216, -2.621784821875001281 ) ) ;
#42499 = CARTESIAN_POINT ( 'NONE',  ( 15.93750000000000000, 5.773502691896255534, 3.535250795749688894E-16 ) ) ;
#42500 = CARTESIAN_POINT ( 'NONE',  ( 8.446875000614518569, -3.027376345333610441, -5.243569643749999898 ) ) ;
#42501 = DIRECTION ( 'NONE',  ( -1.000000000000000000, -0.000000000000000000, -0.000000000000000000 ) ) ;
#42502 = CARTESIAN_POINT ( 'NONE',  ( 12.98437500061451821, 6.421520780324663323E-16, -5.243569643749999010 ) ) ;
#42503 = DIRECTION ( 'NONE',  ( -1.000000000000000000, -0.000000000000000000, -0.000000000000000000 ) ) ;
#42504 = CARTESIAN_POINT ( 'NONE',  ( 22.64062500061451644, -3.027376345333614438, 5.243569643749998122 ) ) ;
#42505 = CARTESIAN_POINT ( 'NONE',  ( -2.121784821874996840, 10.03437500061451892, 33.67503911421598417 ) ) ;
#42506 = CARTESIAN_POINT ( 'NONE',  ( 2.000000000000000444, 20.61874999877096570, 26.53589838486224650 ) ) ;
#42507 = CARTESIAN_POINT ( 'NONE',  ( 25.43437500061451573, -4.541064518000419881, 2.621784821874995952 ) ) ;
#42508 = CARTESIAN_POINT ( 'NONE',  ( 5.578125000614518214, -4.541064518000419881, 2.621784821874995952 ) ) ;
#42509 = CARTESIAN_POINT ( 'NONE',  ( 21.98437500061451644, 5.492252693125287522, 3.363034840372157021E-16 ) ) ;
#42510 = CARTESIAN_POINT ( 'NONE',  ( 15.90937500061451892, 0.000000000000000000, 5.243569643749999010 ) ) ;
#42511 = CARTESIAN_POINT ( 'NONE',  ( 8.559375000614515727, 2.746126346562643317, 4.756430356249998326 ) ) ;
#42512 = CARTESIAN_POINT ( 'NONE',  ( 28.38750000122903216, -4.330127018922194537, 2.499999999999995559 ) ) ;
#42513 = CARTESIAN_POINT ( 'NONE',  ( 6.721875000614518925, 3.027376345333613106, -5.243569643749998122 ) ) ;
#42514 = CARTESIAN_POINT ( 'NONE',  ( 16.47187500061452070, -6.054752690667223547, -1.112240025338166033E-15 ) ) ;
#42515 = CARTESIAN_POINT ( 'NONE',  ( 21.63749999999999929, -2.886751345948126435, -5.000000000000000000 ) ) ;
#42516 = CARTESIAN_POINT ( 'NONE',  ( 23.69999999999999929, 0.000000000000000000, 4.999999999999998224 ) ) ;
#42517 = CARTESIAN_POINT ( 'NONE',  ( 27.08437500061451786, 4.541064518000418104, 2.621784821874999949 ) ) ;
#42518 = CARTESIAN_POINT ( 'NONE',  ( 3.756430356250000546, 14.14062499938548356, 27.83122392262697886 ) ) ;
#42519 = CARTESIAN_POINT ( 'NONE',  ( 30.00000000000000000, 0.000000000000000000, 4.999999999999998224 ) ) ;
#42520 = CARTESIAN_POINT ( 'NONE',  ( 7.800000000000001599, 4.330127018922192761, -2.499999999999997780 ) ) ;
#42521 = CARTESIAN_POINT ( 'NONE',  ( 9.459375000614519635, 2.746126346562643317, 4.756430356249998326 ) ) ;
#42522 = CARTESIAN_POINT ( 'NONE',  ( 21.59062500061451928, 6.054752690667223547, 3.707466751127219781E-16 ) ) ;
#42523 = CARTESIAN_POINT ( 'NONE',  ( 12.63749999999999929, -2.886751345948125991, -5.000000000000000000 ) ) ;
#42524 = CARTESIAN_POINT ( 'NONE',  ( 7.753125000614518036, 0.000000000000000000, 5.243569643749999010 ) ) ;
#42525 = CARTESIAN_POINT ( 'NONE',  ( 19.50000000000000000, 4.330127018922192761, -2.499999999999997780 ) ) ;
#42526 = CARTESIAN_POINT ( 'NONE',  ( 18.59062500061451573, -3.027376345333614438, 5.243569643749998122 ) ) ;
#42527 = CARTESIAN_POINT ( 'NONE',  ( 4.898587196589411843E-16, 20.00000000000000000, 33.99999999999999289 ) ) ;
#42528 = CARTESIAN_POINT ( 'NONE',  ( 24.18750000122903288, 4.330127018922191873, 2.499999999999999556 ) ) ;
#42529 = CARTESIAN_POINT ( 'NONE',  ( -3.756430356249999214, 18.67812499938548143, 27.83122392262697176 ) ) ;
#42530 = CARTESIAN_POINT ( 'NONE',  ( 6.075000000000000178, 4.330127018922191873, 2.499999999999999556 ) ) ;
#42531 = ORIENTED_EDGE ( 'NONE', *, *, #20226, .T. ) ;
#42532 = CARTESIAN_POINT ( 'NONE',  ( 19.94062500061451715, -3.027376345333614438, 5.243569643749998122 ) ) ;
#42533 = CARTESIAN_POINT ( 'NONE',  ( 26.80312500061451431, -4.541064518000417216, -2.621784821875001281 ) ) ;
#42534 = CARTESIAN_POINT ( 'NONE',  ( 24.23437500061451644, 6.421520780324663323E-16, -5.243569643749999010 ) ) ;
#42535 = CARTESIAN_POINT ( 'NONE',  ( 9.562500000000001776, 2.886751345948129099, -4.999999999999998224 ) ) ;
#42536 = CARTESIAN_POINT ( 'NONE',  ( 11.46562500061451573, -6.054752690667223547, -1.112240025338166033E-15 ) ) ;
#42537 = CARTESIAN_POINT ( 'NONE',  ( 26.39062500061451644, -3.027376345333610441, -5.243569643749999898 ) ) ;
#42538 = CARTESIAN_POINT ( 'NONE',  ( 15.90937500061451892, 0.000000000000000000, 5.243569643749999010 ) ) ;
#42539 = CARTESIAN_POINT ( 'NONE',  ( 8.990625000614516082, 6.054752690667223547, 3.707466751127219781E-16 ) ) ;
#42540 = CARTESIAN_POINT ( 'NONE',  ( 22.98750000000000071, -2.886751345948126435, -5.000000000000000000 ) ) ;
#42541 = CARTESIAN_POINT ( 'NONE',  ( 4.243569643749999898, 11.53437500061451892, 30.00000000000000000 ) ) ;
#42542 = CARTESIAN_POINT ( 'NONE',  ( 23.32500000122903572, 2.886751345948126879, 4.999999999999999112 ) ) ;
#42543 = CARTESIAN_POINT ( 'NONE',  ( 19.92187500061451644, 2.746126346562643317, 4.756430356249998326 ) ) ;
#42544 = CARTESIAN_POINT ( 'NONE',  ( 13.79062500061451502, -3.027376345333610441, -5.243569643749999898 ) ) ;
#42545 = CARTESIAN_POINT ( 'NONE',  ( 10.24687500061451750, -3.027376345333610441, -5.243569643749999898 ) ) ;
#42546 = CARTESIAN_POINT ( 'NONE',  ( 10.73437500061451644, 6.421520780324663323E-16, -5.243569643749999010 ) ) ;
#42547 = VERTEX_POINT ( 'NONE', #58482 ) ;
#42548 = CARTESIAN_POINT ( 'NONE',  ( -0.2030170140429748138, 10.00000000000000711, 36.00000000000002842 ) ) ;
#42549 = CARTESIAN_POINT ( 'NONE',  ( 22.26562500061451644, -6.054752690667223547, -1.112240025338166033E-15 ) ) ;
#42550 = CARTESIAN_POINT ( 'NONE',  ( 16.80937500061451573, 0.000000000000000000, 5.243569643749999010 ) ) ;
#42551 = CARTESIAN_POINT ( 'NONE',  ( 22.00312500061451360, 4.541064518000418104, -2.621784821874998173 ) ) ;
#42552 = CARTESIAN_POINT ( 'NONE',  ( 3.999999999999998668, 12.16250000000000142, 27.69059892324149175 ) ) ;
#42553 = CARTESIAN_POINT ( 'NONE',  ( 26.84062500061451573, -3.027376345333610441, -5.243569643749999898 ) ) ;
#42554 = CARTESIAN_POINT ( 'NONE',  ( 6.225000001229036073, 2.886751345948126879, 4.999999999999999112 ) ) ;
#42555 = ORIENTED_EDGE ( 'NONE', *, *, #37818, .T. ) ;
#42556 = CARTESIAN_POINT ( 'NONE',  ( 29.73750000000000071, -2.886751345948125991, -5.000000000000000000 ) ) ;
#42557 = CARTESIAN_POINT ( 'NONE',  ( -1.999999999999997113, 18.72500000000000142, -26.53589838486224295 ) ) ;
#42558 = CARTESIAN_POINT ( 'NONE',  ( 23.73750000122903359, 4.330127018922191873, 2.499999999999999556 ) ) ;
#42559 = CARTESIAN_POINT ( 'NONE',  ( -7.967954043666661671E-16, 16.24062499938548143, 34.33755215474603517 ) ) ;
#42560 = CARTESIAN_POINT ( 'NONE',  ( 7.921875000614517326, -6.054752690667223547, -1.112240025338166033E-15 ) ) ;
#42561 = CARTESIAN_POINT ( 'NONE',  ( 12.75000000000000178, 4.330127018922192761, -2.499999999999997780 ) ) ;
#42562 = CARTESIAN_POINT ( 'NONE',  ( 14.27812500061451573, 6.421520780324663323E-16, -5.243569643749999010 ) ) ;
#42563 = CARTESIAN_POINT ( 'NONE',  ( 7.734375000614517326, 4.541064518000418104, 2.621784821874999949 ) ) ;
#42564 = CARTESIAN_POINT ( 'NONE',  ( 26.02500000122903145, 2.886751345948126879, 4.999999999999999112 ) ) ;
#42565 = CARTESIAN_POINT ( 'NONE',  ( 16.24687500061451573, 6.054752690667223547, 3.707466751127219781E-16 ) ) ;
#42566 = CARTESIAN_POINT ( 'NONE',  ( 4.584375000614516971, 4.541064518000418104, 2.621784821874999949 ) ) ;
#42567 = CARTESIAN_POINT ( 'NONE',  ( 4.924325218087134637, -0.8666147624583920850, 4.924325218087160394 ) ) ;
#42568 = CARTESIAN_POINT ( 'NONE',  ( 4.565625000614516260, 3.027376345333611329, 5.243569643749999010 ) ) ;
#42569 = CARTESIAN_POINT ( 'NONE',  ( 16.22812500061451857, 4.541064518000418104, 2.621784821874999949 ) ) ;
#42570 = EDGE_LOOP ( 'NONE', ( #68240, #42938, #18589, #55019 ) ) ;
#42571 = EDGE_CURVE ( 'NONE', #18997, #11892, #533, .T. ) ;
#42572 = CARTESIAN_POINT ( 'NONE',  ( 13.11562500061451786, 3.027376345333611329, 5.243569643749999010 ) ) ;
#42573 = CARTESIAN_POINT ( 'NONE',  ( 6.525000001229033231, 2.886751345948129099, -4.999999999999998224 ) ) ;
#42574 = CARTESIAN_POINT ( 'NONE',  ( 9.628125000614517148, -4.541064518000419881, 2.621784821874995952 ) ) ;
#42575 = CARTESIAN_POINT ( 'NONE',  ( 20.93437500061451573, -4.119189519843968306, 2.378215178124996054 ) ) ;
#42576 = CARTESIAN_POINT ( 'NONE',  ( 11.40000000000000036, 4.330127018922192761, -2.499999999999997780 ) ) ;
#42577 = CARTESIAN_POINT ( 'NONE',  ( 4.837500001229035895, 4.330127018922191873, 2.499999999999999556 ) ) ;
#42578 = EDGE_CURVE ( 'NONE', #100, #68026, #32619, .T. ) ;
#42579 = CARTESIAN_POINT ( 'NONE',  ( 21.15000000000000213, -4.330127018922190985, -2.500000000000001332 ) ) ;
#42580 = ADVANCED_FACE ( 'NONE', ( #66231 ), #59950, .T. ) ;
#42581 = CARTESIAN_POINT ( 'NONE',  ( 15.83437500061451608, 4.541064518000418104, 2.621784821874999949 ) ) ;
#42582 = CARTESIAN_POINT ( 'NONE',  ( 15.63750000122903216, 4.330127018922191873, 2.499999999999999556 ) ) ;
#42583 = CARTESIAN_POINT ( 'NONE',  ( 23.28750000000000142, -2.886751345948129988, 4.999999999999997335 ) ) ;
#42584 = CARTESIAN_POINT ( 'NONE',  ( -3.000416591977282496E-16, 18.79062500061451857, -34.90005215228797653 ) ) ;
#42585 = CARTESIAN_POINT ( 'NONE',  ( 30.00000000000000000, 6.123233995736764310E-16, -4.999999999999998224 ) ) ;
#42586 = CARTESIAN_POINT ( 'NONE',  ( 8.849999999999999645, 0.000000000000000000, 4.999999999999998224 ) ) ;
#42587 = CARTESIAN_POINT ( 'NONE',  ( 29.09062500061451573, -3.027376345333610441, -5.243569643749999898 ) ) ;
#42588 = CARTESIAN_POINT ( 'NONE',  ( 3.468651194388615799, -3.601174654424125432, 3.564426390351662199 ) ) ;
#42589 = CARTESIAN_POINT ( 'NONE',  ( 19.51875000122903359, 2.886751345948129099, -4.999999999999997335 ) ) ;
#42590 = CARTESIAN_POINT ( 'NONE',  ( 14.85937500061451644, 4.541064518000418104, -2.621784821874998173 ) ) ;
#42591 = EDGE_CURVE ( 'NONE', #41505, #33272, #20421, .T. ) ;
#42592 = CARTESIAN_POINT ( 'NONE',  ( 29.96250000000000213, 2.886751345948126879, 4.999999999999999112 ) ) ;
#42593 = CARTESIAN_POINT ( 'NONE',  ( 11.46562500061451573, -6.054752690667223547, -1.112240025338166033E-15 ) ) ;
#42594 = CARTESIAN_POINT ( 'NONE',  ( 7.481250001229032165, 4.330127018922191873, 2.499999999999999556 ) ) ;
#42595 = CARTESIAN_POINT ( 'NONE',  ( 23.67187500061451999, -6.054752690667223547, -1.112240025338166033E-15 ) ) ;
#42596 = CARTESIAN_POINT ( 'NONE',  ( 16.62187500061451573, 4.119189519843966529, 2.378215178124999607 ) ) ;
#42597 = CARTESIAN_POINT ( 'NONE',  ( 10.86562500061451431, 3.027376345333611329, 5.243569643749999010 ) ) ;
#42598 = CARTESIAN_POINT ( 'NONE',  ( 14.29687500061451821, -3.027376345333610441, -5.243569643749999898 ) ) ;
#42599 = ORIENTED_EDGE ( 'NONE', *, *, #33236, .F. ) ;
#42600 = CARTESIAN_POINT ( 'NONE',  ( 23.93437500061451573, 4.541064518000418104, 2.621784821874999949 ) ) ;
#42601 = CARTESIAN_POINT ( 'NONE',  ( 27.40312500061451573, 4.541064518000418104, -2.621784821874998173 ) ) ;
#42602 = CARTESIAN_POINT ( 'NONE',  ( 0.000000000000000000, 20.00000000000000000, -30.00000000000000000 ) ) ;
#42603 = CARTESIAN_POINT ( 'NONE',  ( 8.175000000000002487, 6.123233995736764310E-16, -4.999999999999998224 ) ) ;
#42604 = CARTESIAN_POINT ( 'NONE',  ( 17.55000000122903359, -2.886751345948129988, 4.999999999999997335 ) ) ;
#42605 = DIRECTION ( 'NONE',  ( 0.000000000000000000, 0.000000000000000000, -1.000000000000000000 ) ) ;
#42606 = CARTESIAN_POINT ( 'NONE',  ( 9.159375000614517148, -5.492252693125287522, -1.008910452111647106E-15 ) ) ;
#42607 = ORIENTED_EDGE ( 'NONE', *, *, #37730, .F. ) ;
#42608 = CARTESIAN_POINT ( 'NONE',  ( 16.38749999999999929, 5.773502691896255534, 3.535250795749688894E-16 ) ) ;
#42609 = CARTESIAN_POINT ( 'NONE',  ( 18.52499999999999858, 6.123233995736764310E-16, -4.999999999999998224 ) ) ;
#42610 = CARTESIAN_POINT ( 'NONE',  ( 14.50312500061451537, 0.000000000000000000, 5.243569643749999010 ) ) ;
#42611 =( BOUNDED_CURVE ( )  B_SPLINE_CURVE ( 2, ( #61418, #10452, #108, #51065, #10811, #32981, #33346 ),
 .UNSPECIFIED., .F., .F. ) 
 B_SPLINE_CURVE_WITH_KNOTS ( ( 3, 2, 2, 3 ),
 ( 0.5000000000000001110, 0.5033333333333334103, 0.5066666666666667096, 0.5100000000000000089 ),
 .UNSPECIFIED. ) 
 CURVE ( )  GEOMETRIC_REPRESENTATION_ITEM ( )  RATIONAL_B_SPLINE_CURVE ( ( 0.9999999999999955591, 0.8660254037844431485, 1.000000000000000000, 0.8660254037844387076, 1.000000000000000000, 0.8660254037844387076, 1.000000000000000000 ) ) 
 REPRESENTATION_ITEM ( '' )  );
#42612 = VERTEX_POINT ( 'NONE', #54425 ) ;
#42613 = CARTESIAN_POINT ( 'NONE',  ( -1.243387493232115393E-14, 16.60624999877096641, 26.00000000000000000 ) ) ;
#42614 = CARTESIAN_POINT ( 'NONE',  ( -4.243569643749999898, 18.02187500061452141, -32.45002607614398471 ) ) ;
#42615 = CARTESIAN_POINT ( 'NONE',  ( 3.965625000614515727, 3.027376345333613106, -5.243569643749998122 ) ) ;
#42616 = CARTESIAN_POINT ( 'NONE',  ( 19.85625000122902861, -4.330127018922190985, -2.500000000000001332 ) ) ;
#42617 = CARTESIAN_POINT ( 'NONE',  ( 11.62500000000000000, -4.330127018922194537, 2.499999999999995559 ) ) ;
#42618 = CARTESIAN_POINT ( 'NONE',  ( 28.58437500061451431, -2.746126346562642428, -4.756430356249999214 ) ) ;
#42619 = EDGE_LOOP ( 'NONE', ( #61160, #29605, #20598, #10533 ) ) ;
#42620 = CARTESIAN_POINT ( 'NONE',  ( 4.243569643749999898, 14.59062500061451750, 32.45002607614398471 ) ) ;
#42621 = CARTESIAN_POINT ( 'NONE',  ( 26.57812500061451644, 4.541064518000418104, 2.621784821874999949 ) ) ;
#42622 = DIRECTION ( 'NONE',  ( 0.000000000000000000, 0.000000000000000000, 1.000000000000000000 ) ) ;
#42623 = CARTESIAN_POINT ( 'NONE',  ( -7.967954043666661671E-16, 19.27812499938548640, 34.33755215474603517 ) ) ;
#42624 = CARTESIAN_POINT ( 'NONE',  ( 22.77187500061451786, -6.054752690667223547, -1.112240025338166033E-15 ) ) ;
#42625 = CARTESIAN_POINT ( 'NONE',  ( 18.85312500061451502, 4.541064518000418104, -2.621784821874998173 ) ) ;
#42626 = CARTESIAN_POINT ( 'NONE',  ( 4.243569643749999898, 13.69062500061459176, -27.54997392385601529 ) ) ;
#42627 = CARTESIAN_POINT ( 'NONE',  ( 23.51250000122903216, -4.330127018922190985, -2.500000000000001332 ) ) ;
#42628 = CARTESIAN_POINT ( 'NONE',  ( 2.915625000614516793, -6.054752690667223547, -1.112240025338166033E-15 ) ) ;
#42629 = CARTESIAN_POINT ( 'NONE',  ( 26.70937500061451431, 0.000000000000000000, 4.756430356249998326 ) ) ;
#42630 = CARTESIAN_POINT ( 'NONE',  ( 21.85312500061451502, -4.541064518000417216, -2.621784821875001281 ) ) ;
#42631 = CARTESIAN_POINT ( 'NONE',  ( 10.84687500061451892, 5.492252693125287522, 3.363034840372157021E-16 ) ) ;
#42632 = CARTESIAN_POINT ( 'NONE',  ( 3.756430356250000102, 16.69062499938548427, 30.00000000000000000 ) ) ;
#42633 = CARTESIAN_POINT ( 'NONE',  ( 17.40937500061451715, -4.541064518000417216, -2.621784821875001281 ) ) ;
#42634 = CARTESIAN_POINT ( 'NONE',  ( 17.63437500061451502, 4.541064518000418104, 2.621784821874999949 ) ) ;
#42635 = CARTESIAN_POINT ( 'NONE',  ( 25.24687500061451573, 6.054752690667223547, 3.707466751127219781E-16 ) ) ;
#42636 = CARTESIAN_POINT ( 'NONE',  ( -4.243569643749999898, 13.10937500061451821, 30.00000000000000000 ) ) ;
#42637 = CARTESIAN_POINT ( 'NONE',  ( 5.728125000614515905, 6.421520780324663323E-16, -5.243569643749999010 ) ) ;
#42638 = CARTESIAN_POINT ( 'NONE',  ( 28.56562500061451715, -6.054752690667223547, -1.112240025338166033E-15 ) ) ;
#42639 = CARTESIAN_POINT ( 'NONE',  ( 29.80312500061451431, 0.000000000000000000, 5.243569643749999010 ) ) ;
#42640 = CARTESIAN_POINT ( 'NONE',  ( 3.486133158594716510E-16, 19.55000000122903359, -34.00000000000000000 ) ) ;
#42641 = CARTESIAN_POINT ( 'NONE',  ( -1.999999999999997113, 18.27499999999999858, 33.46410161513775705 ) ) ;
#42642 = CARTESIAN_POINT ( 'NONE',  ( 3.740625000614516527, -3.027376345333614438, 5.243569643749998122 ) ) ;
#42643 = CARTESIAN_POINT ( 'NONE',  ( 6.871875000614517504, 3.027376345333611329, 5.243569643749999010 ) ) ;
#42644 = APPLICATION_PROTOCOL_DEFINITION ( 'draft international standard', 'automotive_design', 1998, #50292 ) ;
#42645 = CARTESIAN_POINT ( 'NONE',  ( 13.31250000122903288, 4.330127018922192761, -2.499999999999997780 ) ) ;
#42646 = CARTESIAN_POINT ( 'NONE',  ( 12.71250000122903145, -4.330127018922190985, -2.500000000000001332 ) ) ;
#42647 = CARTESIAN_POINT ( 'NONE',  ( 5.353125000614515905, 4.541064518000418104, -2.621784821874998173 ) ) ;
#42648 = CARTESIAN_POINT ( 'NONE',  ( -3.999999999999999556, 16.23124999877096641, 27.69059892324149175 ) ) ;
#42649 = CARTESIAN_POINT ( 'NONE',  ( 20.00625000122903430, 4.330127018922192761, -2.499999999999997780 ) ) ;
#42650 = CARTESIAN_POINT ( 'NONE',  ( 15.00937500061451679, 0.000000000000000000, 5.243569643749999010 ) ) ;
#42651 = CARTESIAN_POINT ( 'NONE',  ( 1.592000809091587073E-14, 17.18750000000000355, -34.00000000000000000 ) ) ;
#42652 = ORIENTED_EDGE ( 'NONE', *, *, #61749, .T. ) ;
#42653 = CARTESIAN_POINT ( 'NONE',  ( 23.01562500061451644, 3.027376345333611329, 5.243569643749999010 ) ) ;
#42654 = CARTESIAN_POINT ( 'NONE',  ( 7.603125000614517681, 4.541064518000418104, -2.621784821874998173 ) ) ;
#42655 = CARTESIAN_POINT ( 'NONE',  ( 25.32187500061451857, 3.027376345333611329, 5.243569643749999010 ) ) ;
#42656 = CARTESIAN_POINT ( 'NONE',  ( 7.565625000614518036, 3.027376345333613106, -5.243569643749998122 ) ) ;
#42657 = CARTESIAN_POINT ( 'NONE',  ( 1.626862140677534273E-15, 10.32500000122903572, 34.00000000000000000 ) ) ;
#42658 = CARTESIAN_POINT ( 'NONE',  ( 8.662500001229034297, -4.330127018922190985, -2.500000000000001332 ) ) ;
#42659 = CARTESIAN_POINT ( 'NONE',  ( 22.07812500061451644, 4.541064518000418104, 2.621784821874999949 ) ) ;
#42660 = CARTESIAN_POINT ( 'NONE',  ( -2.121784821874999949, 11.17812500061451786, -33.67503911421598417 ) ) ;
#42661 = CARTESIAN_POINT ( 'NONE',  ( 9.975000001229034297, -5.773502691896255534, -1.060575238724906372E-15 ) ) ;
#42662 = CARTESIAN_POINT ( 'NONE',  ( 19.56562500061451715, -6.054752690667223547, -1.112240025338166033E-15 ) ) ;
#42663 = CARTESIAN_POINT ( 'NONE',  ( 18.47812500061451857, 4.541064518000418104, 2.621784821874999949 ) ) ;
#42664 = CARTESIAN_POINT ( 'NONE',  ( 28.54687500061451644, -2.746126346562646425, 4.756430356249996549 ) ) ;
#42665 = EDGE_CURVE ( 'NONE', #1656, #42390, #104, .T. ) ;
#42666 = CARTESIAN_POINT ( 'NONE',  ( 18.14999999999999858, 4.330127018922192761, -2.499999999999997780 ) ) ;
#42667 = CARTESIAN_POINT ( 'NONE',  ( 12.75000000122903643, -2.886751345948125991, -5.000000000000000000 ) ) ;
#42668 = CARTESIAN_POINT ( 'NONE',  ( 11.61562500061451608, 3.027376345333613106, -5.243569643749998122 ) ) ;
#42669 = CARTESIAN_POINT ( 'NONE',  ( 12.47812500061451502, 6.421520780324663323E-16, -5.243569643749999010 ) ) ;
#42670 = EDGE_CURVE ( 'NONE', #66931, #71147, #26608, .T. ) ;
#42671 = CARTESIAN_POINT ( 'NONE',  ( 23.36250000122903359, 0.000000000000000000, 4.999999999999998224 ) ) ;
#42672 = CARTESIAN_POINT ( 'NONE',  ( 21.00937500061451857, -4.541064518000417216, -2.621784821875001281 ) ) ;
#42673 = CARTESIAN_POINT ( 'NONE',  ( 20.37187500061451573, 3.027376345333611329, 5.243569643749999010 ) ) ;
#42674 = CARTESIAN_POINT ( 'NONE',  ( 3.539158067892712811, 3.531921335771147863, -3.875648772243089457 ) ) ;
#42675 = CARTESIAN_POINT ( 'NONE',  ( 8.812500001229034652, 4.330127018922192761, -2.499999999999997780 ) ) ;
#42676 = CARTESIAN_POINT ( 'NONE',  ( 7.359375000614516438, 0.000000000000000000, 5.243569643749999010 ) ) ;
#42677 = CARTESIAN_POINT ( 'NONE',  ( 22.58437500061451431, 4.541064518000418104, 2.621784821874999949 ) ) ;
#42678 = CARTESIAN_POINT ( 'NONE',  ( 26.58750000122903145, -4.330127018922194537, 2.499999999999995559 ) ) ;
#42679 = CARTESIAN_POINT ( 'NONE',  ( 19.67812500061451786, 6.421520780324663323E-16, -5.243569643749999010 ) ) ;
#42680 = CARTESIAN_POINT ( 'NONE',  ( 24.72187500061451360, 3.027376345333613106, -5.243569643749998122 ) ) ;
#42681 = CARTESIAN_POINT ( 'NONE',  ( -1.878215178125001827, 19.80312499938548143, 33.25316411605952283 ) ) ;
#42682 = CARTESIAN_POINT ( 'NONE',  ( -3.999999999999997335, 11.15000000122903501, -27.69059892324149530 ) ) ;
#42683 = CARTESIAN_POINT ( 'NONE',  ( 45.00000000000000000, 0.000000000000000000, 4.999999999999998224 ) ) ;
#42684 = CARTESIAN_POINT ( 'NONE',  ( 6.159375000614517148, -4.541064518000417216, -2.621784821875001281 ) ) ;
#42685 = CARTESIAN_POINT ( 'NONE',  ( 17.54062500061451502, 6.054752690667223547, 3.707466751127219781E-16 ) ) ;
#42686 = CARTESIAN_POINT ( 'NONE',  ( 12.83437500061451786, -4.541064518000419881, 2.621784821874995952 ) ) ;
#42687 = ORIENTED_EDGE ( 'NONE', *, *, #48920, .F. ) ;
#42688 = DIRECTION ( 'NONE',  ( 0.000000000000000000, 1.000000000000000000, 0.000000000000000000 ) ) ;
#42689 = CARTESIAN_POINT ( 'NONE',  ( 24.21562500061451573, 3.027376345333613106, -5.243569643749998122 ) ) ;
#42690 = CARTESIAN_POINT ( 'NONE',  ( 3.531796677802674811, 3.539267187803308179, -3.868928841707397925 ) ) ;
#42691 = LINE ( 'NONE', #24232, #17143 ) ;
#42692 = CARTESIAN_POINT ( 'NONE',  ( 15.45000000000000107, 4.330127018922192761, -2.499999999999997780 ) ) ;
#42693 = CARTESIAN_POINT ( 'NONE',  ( 24.93750000122903288, 6.123233995736764310E-16, -4.999999999999998224 ) ) ;
#42694 = CARTESIAN_POINT ( 'NONE',  ( 17.80312500061451786, -4.541064518000417216, -2.621784821875001281 ) ) ;
#42695 = ORIENTED_EDGE ( 'NONE', *, *, #36009, .F. ) ;
#42696 = CARTESIAN_POINT ( 'NONE',  ( 22.46250000000000213, -5.773502691896255534, -1.060575238724906372E-15 ) ) ;
#42697 = CARTESIAN_POINT ( 'NONE',  ( 23.44687500061451502, 6.054752690667223547, 3.707466751127219781E-16 ) ) ;
#42698 = ORIENTED_EDGE ( 'NONE', *, *, #30396, .T. ) ;
#42699 = CARTESIAN_POINT ( 'NONE',  ( 34.99999999999999289, -2.499999999999999556, -3.499999999999999556 ) ) ;
#42700 = CARTESIAN_POINT ( 'NONE',  ( 13.82812500061451466, 6.421520780324663323E-16, -5.243569643749999010 ) ) ;
#42701 = CARTESIAN_POINT ( 'NONE',  ( 4.265625000614517326, -6.054752690667223547, -1.112240025338166033E-15 ) ) ;
#42702 = CARTESIAN_POINT ( 'NONE',  ( 17.55937500061451573, 2.746126346562643317, 4.756430356249998326 ) ) ;
#42703 = CARTESIAN_POINT ( 'NONE',  ( 28.04062500061451502, -3.027376345333614438, 5.243569643749998122 ) ) ;
#42704 = CARTESIAN_POINT ( 'NONE',  ( 11.81250000122903465, -4.330127018922190985, -2.500000000000001332 ) ) ;
#42705 = CARTESIAN_POINT ( 'NONE',  ( 19.46249999999999858, 2.886751345948129099, -4.999999999999998224 ) ) ;
#42706 = CARTESIAN_POINT ( 'NONE',  ( 27.56250000000000000, 2.886751345948129099, -4.999999999999998224 ) ) ;
#42707 = CARTESIAN_POINT ( 'NONE',  ( 18.30000000000000071, 0.000000000000000000, 4.999999999999998224 ) ) ;
#42708 = CARTESIAN_POINT ( 'NONE',  ( 6.984375000614516438, -4.541064518000419881, 2.621784821874995952 ) ) ;
#42709 = CARTESIAN_POINT ( 'NONE',  ( 18.04687500061451999, 6.054752690667223547, 3.707466751127219781E-16 ) ) ;
#42710 = FACE_OUTER_BOUND ( 'NONE', #41812, .T. ) ;
#42711 = EDGE_LOOP ( 'NONE', ( #67927, #63759, #47260, #7248 ) ) ;
#42712 = CARTESIAN_POINT ( 'NONE',  ( 26.54062500061451146, 6.054752690667223547, 3.707466751127219781E-16 ) ) ;
#42713 = CARTESIAN_POINT ( 'NONE',  ( 26.52187500061451431, 3.027376345333613106, -5.243569643749998122 ) ) ;
#42714 = LINE ( 'NONE', #59316, #19177 ) ;
#42715 = CARTESIAN_POINT ( 'NONE',  ( 16.19999999999999929, -4.330127018922190985, -2.500000000000001332 ) ) ;
#42716 = CARTESIAN_POINT ( 'NONE',  ( 11.50312500061451892, -4.541064518000417216, -2.621784821875001281 ) ) ;
#42717 = CARTESIAN_POINT ( 'NONE',  ( 30.00000000000000000, 6.123233995736764310E-16, -4.999999999999998224 ) ) ;
#42718 = DIRECTION ( 'NONE',  ( -1.000000000000000000, -0.000000000000000000, -0.000000000000000000 ) ) ;
#42719 = CARTESIAN_POINT ( 'NONE',  ( 28.90312500061451217, 0.000000000000000000, 5.243569643749999010 ) ) ;
#42720 = CARTESIAN_POINT ( 'NONE',  ( 17.28750000122903430, 6.123233995736764310E-16, -4.999999999999998224 ) ) ;
#42721 = CARTESIAN_POINT ( 'NONE',  ( 3.619842856578028734, -3.449164782042274169, -3.619842856578066481 ) ) ;
#42722 = CARTESIAN_POINT ( 'NONE',  ( 18.38437500061451857, 5.824947211148865298E-16, -4.756430356249998326 ) ) ;
#42723 = CARTESIAN_POINT ( 'NONE',  ( 5.803125000614517859, 4.541064518000418104, -2.621784821874998173 ) ) ;
#42724 = CARTESIAN_POINT ( 'NONE',  ( 21.04687500061451644, -3.027376345333610441, -5.243569643749999898 ) ) ;
#42725 = CARTESIAN_POINT ( 'NONE',  ( -4.243569643749997233, 16.29687500061451644, 32.45002607614398471 ) ) ;
#42726 = CARTESIAN_POINT ( 'NONE',  ( 24.75937500061451502, 4.541064518000418104, -2.621784821874998173 ) ) ;
#42727 = CARTESIAN_POINT ( 'NONE',  ( 4.050000000000001599, -4.330127018922190985, -2.500000000000001332 ) ) ;
#42728 = CARTESIAN_POINT ( 'NONE',  ( 1.999999999999998668, 10.96250000122903501, 26.53589838486224650 ) ) ;
#42729 = CARTESIAN_POINT ( 'NONE',  ( 11.46562500061451573, -6.054752690667223547, -1.112240025338166033E-15 ) ) ;
#42730 = CARTESIAN_POINT ( 'NONE',  ( 5.100000001229034297, -2.886751345948125991, -5.000000000000000000 ) ) ;
#42731 = EDGE_CURVE ( 'NONE', #3869, #13665, #8066, .T. ) ;
#42732 = AXIS2_PLACEMENT_3D ( 'NONE', #58082, #41833, #8954 ) ;
#42733 = CARTESIAN_POINT ( 'NONE',  ( 10.32187500061451679, 3.027376345333613106, -5.243569643749998122 ) ) ;
#42734 = CARTESIAN_POINT ( 'NONE',  ( 3.849130445941352896, -3.191436642873679119, 4.069143491079585395 ) ) ;
#42735 = CARTESIAN_POINT ( 'NONE',  ( 9.890625000614516438, 6.054752690667223547, 3.707466751127219781E-16 ) ) ;
#42736 = CARTESIAN_POINT ( 'NONE',  ( 13.58437500061451786, 4.541064518000418104, 2.621784821874999949 ) ) ;
#42737 = CYLINDRICAL_SURFACE ( 'NONE', #6067, 4.999999999999998224 ) ;
#42738 = CARTESIAN_POINT ( 'NONE',  ( 21.37500000122902932, 2.886751345948129099, -4.999999999999998224 ) ) ;
#42739 = CARTESIAN_POINT ( 'NONE',  ( 9.721875000614517148, -6.054752690667223547, -1.112240025338166033E-15 ) ) ;
#42740 = CARTESIAN_POINT ( 'NONE',  ( 13.37812500061451715, 6.421520780324663323E-16, -5.243569643749999010 ) ) ;
#42741 = CARTESIAN_POINT ( 'NONE',  ( 28.44375000122902719, -2.886751345948125991, -5.000000000000000000 ) ) ;
#42742 = CARTESIAN_POINT ( 'NONE',  ( 20.52187500061451786, -6.054752690667223547, -1.112240025338166033E-15 ) ) ;
#42743 = CARTESIAN_POINT ( 'NONE',  ( 1.071796769724484344, 15.74509619066136956, 34.00000000000000000 ) ) ;
#42744 = CARTESIAN_POINT ( 'NONE',  ( 1.626862140677534273E-15, 12.12500000122903465, -26.00000000000000355 ) ) ;
#42745 = DIRECTION ( 'NONE',  ( -0.000000000000000000, -1.000000000000000000, -0.000000000000000000 ) ) ;
#42746 = CARTESIAN_POINT ( 'NONE',  ( -2.121784821874999949, 15.28437500061451892, -33.67503911421598417 ) ) ;
#42747 = CARTESIAN_POINT ( 'NONE',  ( 15.22500000122903252, 2.886751345948126879, 4.999999999999999112 ) ) ;
#42748 = CARTESIAN_POINT ( 'NONE',  ( 13.05937500061451750, 4.541064518000418104, -2.621784821874998173 ) ) ;
#42749 = CARTESIAN_POINT ( 'NONE',  ( -4.243569643749999898, 17.55312500061451786, -30.00000000000000000 ) ) ;
#42750 = CARTESIAN_POINT ( 'NONE',  ( 18.56250000122903288, -4.330127018922190985, -2.500000000000001332 ) ) ;
#42751 = CARTESIAN_POINT ( 'NONE',  ( 13.34062500061451750, -3.027376345333610441, -5.243569643749999898 ) ) ;
#42752 = ORIENTED_EDGE ( 'NONE', *, *, #21036, .F. ) ;
#42753 = CARTESIAN_POINT ( 'NONE',  ( 15.67500000000000071, -4.330127018922194537, 2.499999999999995559 ) ) ;
#42754 = CARTESIAN_POINT ( 'NONE',  ( -1.071796769724487453, 17.32009619066136707, -34.00000000000000000 ) ) ;
#42755 = CARTESIAN_POINT ( 'NONE',  ( 9.909375000614517148, 4.541064518000418104, -2.621784821874998173 ) ) ;
#42756 = EDGE_CURVE ( 'NONE', #49222, #38333, #15607, .T. ) ;
#42757 = CARTESIAN_POINT ( 'NONE',  ( -1.071796769724504328, 14.35490381179669939, 33.99999999999999289 ) ) ;
#42758 = CARTESIAN_POINT ( 'NONE',  ( 11.58750000122903501, 4.330127018922191873, 2.499999999999999556 ) ) ;
#42759 = CARTESIAN_POINT ( 'NONE',  ( 22.12500000122903288, -5.773502691896255534, -1.060575238724906372E-15 ) ) ;
#42760 = CARTESIAN_POINT ( 'NONE',  ( 18.47812500061451857, 4.541064518000418104, 2.621784821874999949 ) ) ;
#42761 = CARTESIAN_POINT ( 'NONE',  ( 21.06562500061451715, 3.027376345333613106, -5.243569643749998122 ) ) ;
#42762 = CARTESIAN_POINT ( 'NONE',  ( 27.71250000122903145, 4.330127018922192761, -2.499999999999997780 ) ) ;
#42763 = CARTESIAN_POINT ( 'NONE',  ( 3.403125000614518836, -4.541064518000417216, -2.621784821875001281 ) ) ;
#42764 = CARTESIAN_POINT ( 'NONE',  ( 25.05000000000000071, 0.000000000000000000, 4.999999999999998224 ) ) ;
#42765 = CARTESIAN_POINT ( 'NONE',  ( 28.23750000000000071, -2.886751345948137981, 4.999999999999982236 ) ) ;
#42766 = CARTESIAN_POINT ( 'NONE',  ( 29.58749999999999858, -2.886751345948129988, 4.999999999999997335 ) ) ;
#42767 = CARTESIAN_POINT ( 'NONE',  ( 28.65937500061451715, -4.541064518000417216, -2.621784821875001281 ) ) ;
#42768 = CARTESIAN_POINT ( 'NONE',  ( 2.000000000000001332, 17.44999999999999929, 33.46410161513774995 ) ) ;
#42769 = CARTESIAN_POINT ( 'NONE',  ( 2.962500001229034119, 4.330127018922192761, -2.499999999999997780 ) ) ;
#42770 = CARTESIAN_POINT ( 'NONE',  ( 4.462500000000001243, -5.773502691896255534, -1.060575238724906372E-15 ) ) ;
#42771 =( BOUNDED_CURVE ( )  B_SPLINE_CURVE ( 2, ( #23186, #31185, #6207, #6577, #45740, #68275, #17637, #68999, #34635 ),
 .UNSPECIFIED., .F., .F. ) 
 B_SPLINE_CURVE_WITH_KNOTS ( ( 3, 2, 2, 2, 3 ),
 ( 0.6630434782608696231, 0.6666666666666666297, 0.6739130434782608647, 0.6811594202898550998, 0.6847826086956522174 ),
 .UNSPECIFIED. ) 
 CURVE ( )  GEOMETRIC_REPRESENTATION_ITEM ( )  RATIONAL_B_SPLINE_CURVE ( ( 0.9330127018922192983, 0.9330127018922202975, 1.000000000000000000, 0.8660254037844387076, 1.000000000000000000, 0.8660254037844387076, 1.000000000000000000, 0.9330127018922182991, 0.9330127018922192983 ) ) 
 REPRESENTATION_ITEM ( '' )  );
#42772 = DIRECTION ( 'NONE',  ( 0.000000000000000000, -1.000000000000000000, 0.000000000000000000 ) ) ;
#42773 = CARTESIAN_POINT ( 'NONE',  ( 8.034375000614518925, 6.421520780324663323E-16, -5.243569643749999010 ) ) ;
#42774 = CARTESIAN_POINT ( 'NONE',  ( 26.12812500061451360, 4.541064518000418104, 2.621784821874999949 ) ) ;
#42775 = CARTESIAN_POINT ( 'NONE',  ( 5.810221930991193690E-16, 17.11249999999999716, 26.00000000000000000 ) ) ;
#42776 = CARTESIAN_POINT ( 'NONE',  ( 45.00000000000000000, -4.500000000000000000, 3.499999999999999556 ) ) ;
#42777 = CARTESIAN_POINT ( 'NONE',  ( 4.959375000614516971, 4.541064518000418104, -2.621784821874998173 ) ) ;
#42778 = CARTESIAN_POINT ( 'NONE',  ( 9.234375000614518214, -4.541064518000419881, 2.621784821874995952 ) ) ;
#42779 = CARTESIAN_POINT ( 'NONE',  ( 3.975000000000002753, -4.330127018922194537, 2.499999999999995559 ) ) ;
#42780 = CARTESIAN_POINT ( 'NONE',  ( -2.121784821874999949, 12.07812500061459637, 26.32496088578401938 ) ) ;
#42781 = CARTESIAN_POINT ( 'NONE',  ( 29.88749999999999929, 5.773502691896255534, 3.535250795749688894E-16 ) ) ;
#42782 = CARTESIAN_POINT ( 'NONE',  ( 4.912499999999999645, -5.773502691896255534, -1.060575238724906372E-15 ) ) ;
#42783 = CARTESIAN_POINT ( 'NONE',  ( 15.34687500061451537, 0.000000000000000000, 4.756430356249998326 ) ) ;
#42784 = ORIENTED_EDGE ( 'NONE', *, *, #11885, .T. ) ;
#42785 = CARTESIAN_POINT ( 'NONE',  ( 19.37812500061451715, 4.541064518000418104, 2.621784821874999949 ) ) ;
#42786 = CARTESIAN_POINT ( 'NONE',  ( 11.57812500061451644, 6.421520780324663323E-16, -5.243569643749999010 ) ) ;
#42787 = CARTESIAN_POINT ( 'NONE',  ( 24.60937500061451644, 2.746126346562645981, -4.756430356249997438 ) ) ;
#42788 = CARTESIAN_POINT ( 'NONE',  ( 5.896875000614518747, 6.054752690667223547, 3.707466751127219781E-16 ) ) ;
#42789 = CARTESIAN_POINT ( 'NONE',  ( 24.18750000000000355, -2.886751345948129988, 4.999999999999997335 ) ) ;
#42790 = CARTESIAN_POINT ( 'NONE',  ( 21.33750000122903145, 6.123233995736764310E-16, -4.999999999999998224 ) ) ;
#42791 = CARTESIAN_POINT ( 'NONE',  ( 28.07812500061451289, -4.541064518000419881, 2.621784821874995952 ) ) ;
#42792 = CYLINDRICAL_SURFACE ( 'NONE', #49690, 4.000000000000000000 ) ;
#42793 = CARTESIAN_POINT ( 'NONE',  ( 9.421875000614519990, 3.027376345333613106, -5.243569643749998122 ) ) ;
#42794 = CARTESIAN_POINT ( 'NONE',  ( 14.97187500061451892, 3.027376345333611329, 5.243569643749999010 ) ) ;
#42795 = CARTESIAN_POINT ( 'NONE',  ( 24.53437500061451715, -4.541064518000419881, 2.621784821874995952 ) ) ;
#42796 = CARTESIAN_POINT ( 'NONE',  ( 8.456250001229033586, 0.000000000000000000, 4.999999999999998224 ) ) ;
#42797 = CARTESIAN_POINT ( 'NONE',  ( 12.90000000000000213, 0.000000000000000000, 4.999999999999998224 ) ) ;
#42798 = CARTESIAN_POINT ( 'NONE',  ( 20.22187500061451715, 3.027376345333613106, -5.243569643749998122 ) ) ;
#42799 = CARTESIAN_POINT ( 'NONE',  ( 8.634375000614518569, 4.541064518000418104, 2.621784821874999949 ) ) ;
#42800 = CARTESIAN_POINT ( 'NONE',  ( -7.967954043666661671E-16, 19.84062499938548285, 34.33755215474603517 ) ) ;
#42801 = CARTESIAN_POINT ( 'NONE',  ( 22.76249999999999574, 2.886751345948126879, 4.999999999999999112 ) ) ;
#42802 = CARTESIAN_POINT ( 'NONE',  ( -8.484601909799255319E-16, 14.63750000000000107, 34.61880215351700940 ) ) ;
#42803 = CARTESIAN_POINT ( 'NONE',  ( 4.243569643749999010, 13.37187500061451750, -32.45002607614398471 ) ) ;
#42804 = CARTESIAN_POINT ( 'NONE',  ( 25.69687500061451502, 5.492252693125287522, 3.363034840372157021E-16 ) ) ;
#42805 = CARTESIAN_POINT ( 'NONE',  ( 15.14062500061451644, -3.027376345333610441, -5.243569643749999898 ) ) ;
#42806 = CARTESIAN_POINT ( 'NONE',  ( 3.487500000000000711, -2.886751345948129988, 4.999999999999997335 ) ) ;
#42807 = SURFACE_STYLE_USAGE ( .BOTH. , #36895 ) ;
#42808 = CARTESIAN_POINT ( 'NONE',  ( 15.93750000122903110, 6.123233995736764310E-16, -4.999999999999998224 ) ) ;
#42809 = CARTESIAN_POINT ( 'NONE',  ( 12.07499999999999929, -4.330127018922194537, 2.499999999999995559 ) ) ;
#42810 = CARTESIAN_POINT ( 'NONE',  ( 4.000000000000000000, 18.50000000122903288, 32.30940107675849049 ) ) ;
#42811 = CARTESIAN_POINT ( 'NONE',  ( 11.88750000122903216, 6.123233995736764310E-16, -4.999999999999998224 ) ) ;
#42812 = CARTESIAN_POINT ( 'NONE',  ( 22.09687500061451715, 6.054752690667223547, 3.707466751127219781E-16 ) ) ;
#42813 = CARTESIAN_POINT ( 'NONE',  ( 16.80937500061451573, 0.000000000000000000, 5.243569643749999010 ) ) ;
#42814 = CARTESIAN_POINT ( 'NONE',  ( 7.106250001229032165, 0.000000000000000000, 4.999999999999998224 ) ) ;
#42815 = ORIENTED_EDGE ( 'NONE', *, *, #46671, .F. ) ;
#42816 = CARTESIAN_POINT ( 'NONE',  ( 17.72812500061451502, -4.541064518000419881, 2.621784821874995952 ) ) ;
#42817 = CARTESIAN_POINT ( 'NONE',  ( 28.27500000122903145, 2.886751345948126879, 4.999999999999999112 ) ) ;
#42818 = CARTESIAN_POINT ( 'NONE',  ( 16.47187500061452070, -6.054752690667223547, -1.112240025338166033E-15 ) ) ;
#42819 = CARTESIAN_POINT ( 'NONE',  ( 28.80937500061451573, 4.541064518000418104, -2.621784821874998173 ) ) ;
#42820 = CARTESIAN_POINT ( 'NONE',  ( 4.415625000614518569, 3.027376345333613106, -5.243569643749998122 ) ) ;
#42821 = CARTESIAN_POINT ( 'NONE',  ( 18.59062500061451573, -3.027376345333614438, 5.243569643749998122 ) ) ;
#42822 = CARTESIAN_POINT ( 'NONE',  ( 4.243569643749999898, 13.27812500061451750, 30.00000000000000000 ) ) ;
#42823 = CARTESIAN_POINT ( 'NONE',  ( 16.05000000122903359, 5.773502691896255534, 3.535250795749688894E-16 ) ) ;
#42824 = CARTESIAN_POINT ( 'NONE',  ( 8.934375000614517504, 5.824947211148865298E-16, -4.756430356249998326 ) ) ;
#42825 = CARTESIAN_POINT ( 'NONE',  ( 7.715625000614515727, 3.027376345333611329, 5.243569643749999010 ) ) ;
#42826 = CARTESIAN_POINT ( 'NONE',  ( 26.72812500061451502, -4.541064518000419881, 2.621784821874995952 ) ) ;
#42827 = CARTESIAN_POINT ( 'NONE',  ( 1.071796769724490783, 19.07990381179670081, -34.00000000000000000 ) ) ;
#42828 = EDGE_CURVE ( 'NONE', #53311, #23511, #14888, .T. ) ;
#42829 = CARTESIAN_POINT ( 'NONE',  ( 22.99687500061451573, 6.054752690667223547, 3.707466751127219781E-16 ) ) ;
#42830 = CARTESIAN_POINT ( 'NONE',  ( 14.50312500061451537, 0.000000000000000000, 5.243569643749999010 ) ) ;
#42831 = CARTESIAN_POINT ( 'NONE',  ( 21.75000000122903288, -2.886751345948125991, -5.000000000000000000 ) ) ;
#42832 =( BOUNDED_CURVE ( )  B_SPLINE_CURVE ( 2, ( #15885, #66503, #55788, #26252, #9260, #10356, #37690 ),
 .UNSPECIFIED., .F., .F. ) 
 B_SPLINE_CURVE_WITH_KNOTS ( ( 3, 2, 2, 3 ),
 ( 0.1250000000000000000, 0.1277777777777777679, 0.1305555555555555358, 0.1333333333333333037 ),
 .UNSPECIFIED. ) 
 CURVE ( )  GEOMETRIC_REPRESENTATION_ITEM ( )  RATIONAL_B_SPLINE_CURVE ( ( 1.000000000000000000, 0.8660254037844387076, 1.000000000000000000, 0.8660254037844387076, 1.000000000000000000, 0.8660254037844400399, 0.9999999999999986677 ) ) 
 REPRESENTATION_ITEM ( '' )  );
#42833 = CARTESIAN_POINT ( 'NONE',  ( 23.09062500061451573, -3.027376345333614438, 5.243569643749998122 ) ) ;
#42834 = CARTESIAN_POINT ( 'NONE',  ( 18.68437500061451928, -4.541064518000419881, 2.621784821874995952 ) ) ;
#42835 = CARTESIAN_POINT ( 'NONE',  ( 14.39062500061451821, 6.054752690667223547, 3.707466751127219781E-16 ) ) ;
#42836 = CARTESIAN_POINT ( 'NONE',  ( 2.121784821874999061, 14.30937500061451750, 26.32496088578401583 ) ) ;
#42837 = CARTESIAN_POINT ( 'NONE',  ( 18.77812500061451573, 6.421520780324663323E-16, -5.243569643749999010 ) ) ;
#42838 = CARTESIAN_POINT ( 'NONE',  ( -4.000000000000000000, 17.67500000000000071, 30.00000000000000000 ) ) ;
#42839 = ORIENTED_EDGE ( 'NONE', *, *, #67858, .T. ) ;
#42840 = ORIENTED_EDGE ( 'NONE', *, *, #34767, .T. ) ;
#42841 = CARTESIAN_POINT ( 'NONE',  ( 22.38749999999999929, -2.886751345948129988, 4.999999999999997335 ) ) ;
#42842 = CARTESIAN_POINT ( 'NONE',  ( -4.243569643749997233, 19.44687500061451502, -27.54997392385601174 ) ) ;
#42843 = CARTESIAN_POINT ( 'NONE',  ( 13.12500000122903288, -5.773502691896255534, -1.060575238724906372E-15 ) ) ;
#42844 = CARTESIAN_POINT ( 'NONE',  ( 26.16562500061451502, 3.027376345333611329, 5.243569643749999010 ) ) ;
#42845 = CARTESIAN_POINT ( 'NONE',  ( 8.878125000614515372, 6.421520780324663323E-16, -5.243569643749999010 ) ) ;
#42846 = CARTESIAN_POINT ( 'NONE',  ( 18.97500000122903074, -5.773502691896255534, -1.060575238724906372E-15 ) ) ;
#42847 = CARTESIAN_POINT ( 'NONE',  ( 24.51562500061451289, -6.054752690667223547, -1.112240025338166033E-15 ) ) ;
#42848 = CARTESIAN_POINT ( 'NONE',  ( 21.97500000000000142, -4.330127018922194537, 2.499999999999995559 ) ) ;
#42849 = CARTESIAN_POINT ( 'NONE',  ( 28.97812500061451502, -4.541064518000419881, 2.621784821874995952 ) ) ;
#42850 = CARTESIAN_POINT ( 'NONE',  ( 8.278125000614515727, -4.541064518000419881, 2.621784821874995952 ) ) ;
#42851 = ORIENTED_EDGE ( 'NONE', *, *, #68253, .T. ) ;
#42852 = CARTESIAN_POINT ( 'NONE',  ( 23.46562500061451573, 3.027376345333611329, 5.243569643749999010 ) ) ;
#42853 = CARTESIAN_POINT ( 'NONE',  ( 6.290625000614517681, 6.054752690667223547, 3.707466751127219781E-16 ) ) ;
#42854 = CARTESIAN_POINT ( 'NONE',  ( 14.29687500061451821, -2.746126346562642428, -4.756430356249999214 ) ) ;
#42855 = CARTESIAN_POINT ( 'NONE',  ( 3.890625000614517326, -3.027376345333610441, -5.243569643749999898 ) ) ;
#42856 = CARTESIAN_POINT ( 'NONE',  ( 8.484601909799253346E-16, 14.37500000122903288, -25.38119784648299770 ) ) ;
#42857 = CARTESIAN_POINT ( 'NONE',  ( 4.000000000000000000, 12.93124999877096393, 27.69059892324149885 ) ) ;
#42858 = CARTESIAN_POINT ( 'NONE',  ( 11.81250000000000000, 2.886751345948129099, -4.999999999999998224 ) ) ;
#42859 = CARTESIAN_POINT ( 'NONE',  ( 11.48437500061451644, -4.541064518000419881, 2.621784821874995952 ) ) ;
#42860 = CARTESIAN_POINT ( 'NONE',  ( 8.775000001229033231, 2.886751345948129099, -4.999999999999998224 ) ) ;
#42861 = CARTESIAN_POINT ( 'NONE',  ( 14.52187500061451608, 3.027376345333611329, 5.243569643749999010 ) ) ;
#42862 = CARTESIAN_POINT ( 'NONE',  ( 14.28750000000000142, -2.886751345948129988, 4.999999999999997335 ) ) ;
#42863 = CARTESIAN_POINT ( 'NONE',  ( 5.896875000614518747, 6.054752690667223547, 3.707466751127219781E-16 ) ) ;
#42864 = CARTESIAN_POINT ( 'NONE',  ( 34.99999999999999289, 0.000000000000000000, 4.999999999999998224 ) ) ;
#42865 = CARTESIAN_POINT ( 'NONE',  ( 3.727827348360245097, 3.332161949968362347, -3.727827348360304605 ) ) ;
#42866 = CARTESIAN_POINT ( 'NONE',  ( 13.39687500061451608, -3.027376345333610441, -5.243569643749999898 ) ) ;
#42867 = CARTESIAN_POINT ( 'NONE',  ( 3.673424073952555435, 3.392052302514600548, 3.998632574573837584 ) ) ;
#42868 = EDGE_CURVE ( 'NONE', #31980, #26340, #37788, .T. ) ;
#42869 = CARTESIAN_POINT ( 'NONE',  ( 22.71562500061451573, -6.054752690667223547, -1.112240025338166033E-15 ) ) ;
#42870 = CARTESIAN_POINT ( 'NONE',  ( -2.121784821874999949, 10.78437500061451715, 26.32496088578401938 ) ) ;
#42871 = FACE_OUTER_BOUND ( 'NONE', #34816, .T. ) ;
#42872 = CARTESIAN_POINT ( 'NONE',  ( 26.44687500061451502, -3.027376345333610441, -5.243569643749999898 ) ) ;
#42873 = CARTESIAN_POINT ( 'NONE',  ( 29.66249999999999787, -5.773502691896255534, -1.060575238724906372E-15 ) ) ;
#42874 = CARTESIAN_POINT ( 'NONE',  ( 3.965625000614515727, 3.027376345333613106, -5.243569643749998122 ) ) ;
#42875 = CARTESIAN_POINT ( 'NONE',  ( 22.35937500061451644, 2.746126346562645981, -4.756430356249997438 ) ) ;
#42876 = CARTESIAN_POINT ( 'NONE',  ( 15.00937500061451679, 0.000000000000000000, 5.243569643749999010 ) ) ;
#42877 = CARTESIAN_POINT ( 'NONE',  ( 9.046875000614514661, 0.000000000000000000, 4.756430356249998326 ) ) ;
#42878 = CARTESIAN_POINT ( 'NONE',  ( 27.75000000122903288, 5.773502691896255534, 3.535250795749688894E-16 ) ) ;
#42879 = CARTESIAN_POINT ( 'NONE',  ( 5.184375000614516615, -4.541064518000419881, 2.621784821874995952 ) ) ;
#42880 = CARTESIAN_POINT ( 'NONE',  ( 15.53437500061451715, -4.541064518000419881, 2.621784821874995952 ) ) ;
#42881 = CARTESIAN_POINT ( 'NONE',  ( 3.286795329855858760, 3.767887532774327308, -3.286795329856085690 ) ) ;
#42882 = CARTESIAN_POINT ( 'NONE',  ( 24.52499999999999858, 4.330127018922191873, 2.499999999999999556 ) ) ;
#42883 = CARTESIAN_POINT ( 'NONE',  ( 3.562500001229033764, 0.000000000000000000, 4.999999999999998224 ) ) ;
#42884 = CARTESIAN_POINT ( 'NONE',  ( 26.55937500061451573, 4.541064518000418104, -2.621784821874998173 ) ) ;
#42885 = CARTESIAN_POINT ( 'NONE',  ( 3.999999999999998668, 15.61250000000000249, 32.30940107675850470 ) ) ;
#42886 = CARTESIAN_POINT ( 'NONE',  ( 14.21250000122903323, 4.330127018922192761, -2.499999999999997780 ) ) ;
#42887 = CARTESIAN_POINT ( 'NONE',  ( 8.812500000000000000, 2.886751345948126879, 4.999999999999999112 ) ) ;
#42888 = CARTESIAN_POINT ( 'NONE',  ( 9.871875000614517504, 4.119189519843966529, 2.378215178124999607 ) ) ;
#42889 = CARTESIAN_POINT ( 'NONE',  ( 22.37812500061451360, 6.421520780324663323E-16, -5.243569643749999010 ) ) ;
#42890 = CARTESIAN_POINT ( 'NONE',  ( 11.70000000000000284, -4.330127018922190985, -2.500000000000001332 ) ) ;
#42891 = CARTESIAN_POINT ( 'NONE',  ( 4.940625000614515372, 6.054752690667223547, 3.707466751127219781E-16 ) ) ;
#42892 = CARTESIAN_POINT ( 'NONE',  ( 19.53749999999999432, 5.773502691896255534, 3.535250795749688894E-16 ) ) ;
#42893 = CARTESIAN_POINT ( 'NONE',  ( 17.72812500061451502, -4.541064518000419881, 2.621784821874995952 ) ) ;
#42894 = CARTESIAN_POINT ( 'NONE',  ( -3.999999999999997335, 18.80000000122903003, 32.30940107675850470 ) ) ;
#42895 = CARTESIAN_POINT ( 'NONE',  ( 22.98750000122903003, -4.330127018922194537, 2.499999999999995559 ) ) ;
#42896 = CARTESIAN_POINT ( 'NONE',  ( -3.756430356249999214, 19.57812499938548356, 27.83122392262697176 ) ) ;
#42897 = CARTESIAN_POINT ( 'NONE',  ( 29.85937500061451644, 0.000000000000000000, 5.243569643749999010 ) ) ;
#42898 = VERTEX_POINT ( 'NONE', #9719 ) ;
#42899 = CARTESIAN_POINT ( 'NONE',  ( 19.86562500061451786, 3.027376345333611329, 5.243569643749999010 ) ) ;
#42900 = CARTESIAN_POINT ( 'NONE',  ( 24.17812500061451786, 6.421520780324663323E-16, -5.243569643749999010 ) ) ;
#42901 = CARTESIAN_POINT ( 'NONE',  ( 24.64687500061451431, -3.027376345333610441, -5.243569643749999898 ) ) ;
#42902 = CARTESIAN_POINT ( 'NONE',  ( 8.775000000000002132, 4.330127018922191873, 2.499999999999999556 ) ) ;
#42903 = CARTESIAN_POINT ( 'NONE',  ( 12.25312500061451537, 0.000000000000000000, 5.243569643749999010 ) ) ;
#42904 = CARTESIAN_POINT ( 'NONE',  ( 27.36562500061451786, 3.027376345333613106, -5.243569643749998122 ) ) ;
#42905 = CARTESIAN_POINT ( 'NONE',  ( 17.29687500061451999, -3.027376345333614438, 5.243569643749998122 ) ) ;
#42906 = CARTESIAN_POINT ( 'NONE',  ( 9.328125000614518214, 6.421520780324663323E-16, -5.243569643749999010 ) ) ;
#42907 = CARTESIAN_POINT ( 'NONE',  ( 2.946926184779611990, -4.039365056661180731, 3.279941078183791880 ) ) ;
#42908 = CARTESIAN_POINT ( 'NONE',  ( -4.243569643749999898, 9.921875000614519990, 27.54997392385601529 ) ) ;
#42909 = ADVANCED_FACE ( 'NONE', ( #54785 ), #31149, .T. ) ;
#42910 = CARTESIAN_POINT ( 'NONE',  ( 24.82500000122902861, -5.773502691896255534, -1.060575238724906372E-15 ) ) ;
#42911 = CARTESIAN_POINT ( 'NONE',  ( 20.29687500061451289, 5.492252693125287522, 3.363034840372157021E-16 ) ) ;
#42912 = CARTESIAN_POINT ( 'NONE',  ( 14.95312500061451644, 0.000000000000000000, 5.243569643749999010 ) ) ;
#42913 = CARTESIAN_POINT ( 'NONE',  ( 8.596875000614518925, 6.054752690667223547, 3.707466751127219781E-16 ) ) ;
#42914 = CARTESIAN_POINT ( 'NONE',  ( 6.421875000614519102, 3.027376345333611329, 5.243569643749999010 ) ) ;
#42915 = ORIENTED_EDGE ( 'NONE', *, *, #5973, .F. ) ;
#42916 = CARTESIAN_POINT ( 'NONE',  ( 29.63437500061451502, 6.421520780324663323E-16, -5.243569643749999010 ) ) ;
#42917 = CARTESIAN_POINT ( 'NONE',  ( 20.69062500061451715, 6.054752690667223547, 3.707466751127219781E-16 ) ) ;
#42918 = CARTESIAN_POINT ( 'NONE',  ( 15.94687500061451502, -3.027376345333614438, 5.243569643749998122 ) ) ;
#42919 = CARTESIAN_POINT ( 'NONE',  ( 21.59062500061451928, 6.054752690667223547, 3.707466751127219781E-16 ) ) ;
#42920 = CARTESIAN_POINT ( 'NONE',  ( 3.999999999999998668, 10.81250000000000178, 27.69059892324149175 ) ) ;
#42921 = CARTESIAN_POINT ( 'NONE',  ( 27.96562500061451928, 3.027376345333611329, 5.243569643749999010 ) ) ;
#42922 = CARTESIAN_POINT ( 'NONE',  ( 6.037500001229035185, 6.123233995736764310E-16, -4.999999999999998224 ) ) ;
#42923 = ORIENTED_EDGE ( 'NONE', *, *, #26050, .F. ) ;
#42924 = CARTESIAN_POINT ( 'NONE',  ( 29.51249999999999929, 2.886751345948126879, 4.999999999999999112 ) ) ;
#42925 = CARTESIAN_POINT ( 'NONE',  ( -3.999999999999999112, 18.19999999999999929, -30.00000000000000000 ) ) ;
#42926 = CARTESIAN_POINT ( 'NONE',  ( 24.78750000122903074, -4.330127018922194537, 2.499999999999995559 ) ) ;
#42927 = CARTESIAN_POINT ( 'NONE',  ( -3.756430356250000102, 14.77812499938548463, 30.00000000000000000 ) ) ;
#42928 = CARTESIAN_POINT ( 'NONE',  ( 8.296875000614516438, -3.027376345333614438, 5.243569643749998122 ) ) ;
#42929 = CARTESIAN_POINT ( 'NONE',  ( 23.32499999999999929, -4.330127018922194537, 2.499999999999995559 ) ) ;
#42930 = CARTESIAN_POINT ( 'NONE',  ( 14.80312500061451608, 4.541064518000418104, -2.621784821874998173 ) ) ;
#42931 = CARTESIAN_POINT ( 'NONE',  ( 9.384375000614518569, 6.421520780324663323E-16, -5.243569643749999010 ) ) ;
#42932 = CARTESIAN_POINT ( 'NONE',  ( 27.45000000122903572, -2.886751345948129988, 4.999999999999997335 ) ) ;
#42933 = CARTESIAN_POINT ( 'NONE',  ( 18.27187500061451431, -6.054752690667223547, -1.112240025338166033E-15 ) ) ;
#42934 = CARTESIAN_POINT ( 'NONE',  ( 4.471875000614518925, 3.027376345333613106, -5.243569643749998122 ) ) ;
#42935 = CYLINDRICAL_SURFACE ( 'NONE', #20297, 9.999999999999998224 ) ;
#42936 = CARTESIAN_POINT ( 'NONE',  ( 6.515625000614516438, -6.054752690667223547, -1.112240025338166033E-15 ) ) ;
#42937 = CARTESIAN_POINT ( 'NONE',  ( 16.41562500061451857, -6.054752690667223547, -1.112240025338166033E-15 ) ) ;
#42938 = ORIENTED_EDGE ( 'NONE', *, *, #14420, .F. ) ;
#42939 = CARTESIAN_POINT ( 'NONE',  ( 12.81562500061451537, -6.054752690667223547, -1.112240025338166033E-15 ) ) ;
#42940 = CARTESIAN_POINT ( 'NONE',  ( 6.150000001229033231, 5.773502691896255534, 3.535250795749688894E-16 ) ) ;
#42941 = CARTESIAN_POINT ( 'NONE',  ( 11.24062500061451608, 6.054752690667223547, 3.707466751127219781E-16 ) ) ;
#42942 = CARTESIAN_POINT ( 'NONE',  ( 21.64687500061451786, 5.492252693125287522, 3.363034840372157021E-16 ) ) ;
#42943 = CARTESIAN_POINT ( 'NONE',  ( 11.10000000000000142, 0.000000000000000000, 4.999999999999998224 ) ) ;
#42944 = CARTESIAN_POINT ( 'NONE',  ( 5.362500001229033586, 0.000000000000000000, 4.999999999999998224 ) ) ;
#42945 = CARTESIAN_POINT ( 'NONE',  ( 19.01249999999999929, 2.886751345948129099, -4.999999999999998224 ) ) ;
#42946 = CARTESIAN_POINT ( 'NONE',  ( 17.59687500061451715, 6.054752690667223547, 3.707466751127219781E-16 ) ) ;
#42947 = CARTESIAN_POINT ( 'NONE',  ( 16.80000000122903359, -2.886751345948125991, -5.000000000000000000 ) ) ;
#42948 = CARTESIAN_POINT ( 'NONE',  ( 22.27499999999999858, 4.330127018922191873, 2.499999999999999556 ) ) ;
#42949 = CARTESIAN_POINT ( 'NONE',  ( -4.243569643749999898, 17.51562500061451644, -32.45002607614398471 ) ) ;
#42950 = CARTESIAN_POINT ( 'NONE',  ( 1.071796769724488785, 20.05759618943233491, 34.00000000000000000 ) ) ;
#42951 = CARTESIAN_POINT ( 'NONE',  ( 2.735716306934586672, -4.261472593518762508, 2.618912952963186047 ) ) ;
#42952 = LINE ( 'NONE', #14870, #12407 ) ;
#42953 = CARTESIAN_POINT ( 'NONE',  ( 30.00000000000000000, 6.123233995736764310E-16, -4.999999999999998224 ) ) ;
#42954 = CARTESIAN_POINT ( 'NONE',  ( 4.000000000000000000, 19.73749999999999716, 32.30940107675849760 ) ) ;
#42955 = CARTESIAN_POINT ( 'NONE',  ( 16.28437500061452070, 4.541064518000418104, 2.621784821874999949 ) ) ;
#42956 = CARTESIAN_POINT ( 'NONE',  ( 30.00000000000000000, 0.000000000000000000, 4.999999999999998224 ) ) ;
#42957 = CARTESIAN_POINT ( 'NONE',  ( 11.16562500061451679, 3.027376345333613106, -5.243569643749998122 ) ) ;
#42958 = CARTESIAN_POINT ( 'NONE',  ( 7.406250001229033764, 4.330127018922192761, -2.499999999999997780 ) ) ;
#42959 = CARTESIAN_POINT ( 'NONE',  ( 24.94687500061451502, -3.027376345333614438, 5.243569643749998122 ) ) ;
#42960 = CARTESIAN_POINT ( 'NONE',  ( 15.27187500061451608, 4.119189519843966529, 2.378215178124999607 ) ) ;
#42961 = CARTESIAN_POINT ( 'NONE',  ( 6.778125000614518392, 4.541064518000418104, 2.621784821874999949 ) ) ;
#42962 = CARTESIAN_POINT ( 'NONE',  ( 12.38437500061451857, -4.541064518000419881, 2.621784821874995952 ) ) ;
#42963 = ORIENTED_EDGE ( 'NONE', *, *, #10153, .F. ) ;
#42964 = CARTESIAN_POINT ( 'NONE',  ( 24.53437500061451715, -4.541064518000419881, 2.621784821874995952 ) ) ;
#42965 = CARTESIAN_POINT ( 'NONE',  ( 27.85312500061451502, 4.541064518000418104, -2.621784821874998173 ) ) ;
#42966 = CARTESIAN_POINT ( 'NONE',  ( 25.98750000000000426, -2.886751345948157965, 4.999999999999948486 ) ) ;
#42967 = CARTESIAN_POINT ( 'NONE',  ( 8.625000000000000000, 6.123233995736764310E-16, -4.999999999999998224 ) ) ;
#42968 = CARTESIAN_POINT ( 'NONE',  ( 17.28750000122903430, 6.123233995736764310E-16, -4.999999999999998224 ) ) ;
#42969 = CARTESIAN_POINT ( 'NONE',  ( 27.26250000122903216, 4.330127018922192761, -2.499999999999997780 ) ) ;
#42970 = CARTESIAN_POINT ( 'NONE',  ( 7.996875000614515727, 4.119189519843966529, -2.378215178124998275 ) ) ;
#42971 = ORIENTED_EDGE ( 'NONE', *, *, #14959, .T. ) ;
#42972 = CARTESIAN_POINT ( 'NONE',  ( 14.51250000000000107, 2.886751345948129099, -4.999999999999998224 ) ) ;
#42973 =( BOUNDED_CURVE ( )  B_SPLINE_CURVE ( 2, ( #15378, #32749, #26476, #15741, #50109, #26108, #4681, #65628, #44208 ),
 .UNSPECIFIED., .F., .F. ) 
 B_SPLINE_CURVE_WITH_KNOTS ( ( 3, 2, 2, 2, 3 ),
 ( 0.7916666666666667407, 0.7962962962962962798, 0.8055555555555555802, 0.8148148148148147696, 0.8194444444444444198 ),
 .UNSPECIFIED. ) 
 CURVE ( )  GEOMETRIC_REPRESENTATION_ITEM ( )  RATIONAL_B_SPLINE_CURVE ( ( 0.9330127018922192983, 0.9330127018922200755, 1.000000000000000000, 0.8660254037844387076, 1.000000000000000000, 0.8660254037844387076, 1.000000000000000000, 0.9330127018922194093, 0.9330127018922194093 ) ) 
 REPRESENTATION_ITEM ( '' )  );
#42974 = CARTESIAN_POINT ( 'NONE',  ( 18.11250000000000071, 2.886751345948129099, -4.999999999999998224 ) ) ;
#42975 = CARTESIAN_POINT ( 'NONE',  ( 12.17812500061451608, 4.541064518000418104, 2.621784821874999949 ) ) ;
#42976 = ORIENTED_EDGE ( 'NONE', *, *, #50505, .T. ) ;
#42977 = CARTESIAN_POINT ( 'NONE',  ( 30.00000000000000000, 0.000000000000000000, 4.999999999999998224 ) ) ;
#42978 = CARTESIAN_POINT ( 'NONE',  ( 2.121784821874999061, 17.45937500061451786, -33.67503911421598417 ) ) ;
#42979 = CARTESIAN_POINT ( 'NONE',  ( 3.253125000614518036, 0.000000000000000000, 5.243569643749999010 ) ) ;
#42980 = CARTESIAN_POINT ( 'NONE',  ( -3.756430356250000102, 12.86562499938548321, 30.00000000000000000 ) ) ;
#42981 = CARTESIAN_POINT ( 'NONE',  ( 10.53750000000000320, 5.773502691896255534, 3.535250795749688894E-16 ) ) ;
#42982 = CARTESIAN_POINT ( 'NONE',  ( 16.14375000122903359, -2.886751345948130876, 4.999999999999996447 ) ) ;
#42983 = VERTEX_POINT ( 'NONE', #8620 ) ;
#42984 = CARTESIAN_POINT ( 'NONE',  ( -4.243569643749997233, 14.89062500061451644, 32.45002607614398471 ) ) ;
#42985 = CARTESIAN_POINT ( 'NONE',  ( 25.94062500061451715, -3.027376345333610441, -5.243569643749999898 ) ) ;
#42986 = CARTESIAN_POINT ( 'NONE',  ( 8.775000000000002132, 4.330127018922191873, 2.499999999999999556 ) ) ;
#42987 = CARTESIAN_POINT ( 'NONE',  ( -1.878215178125001827, 19.24062499938548143, 33.25316411605952283 ) ) ;
#42988 = CARTESIAN_POINT ( 'NONE',  ( 22.80937500061451573, -4.541064518000417216, -2.621784821875001281 ) ) ;
#42989 = CARTESIAN_POINT ( 'NONE',  ( 18.81562500061452070, 3.027376345333613106, -5.243569643749998122 ) ) ;
#42990 = EDGE_CURVE ( 'NONE', #46607, #21477, #71788, .T. ) ;
#42991 = CARTESIAN_POINT ( 'NONE',  ( 4.243569643749999010, 13.76562500061459282, -32.45002607614398471 ) ) ;
#42992 = CARTESIAN_POINT ( 'NONE',  ( 23.73750000122903359, 4.330127018922191873, 2.499999999999999556 ) ) ;
#42993 = CARTESIAN_POINT ( 'NONE',  ( 3.628125000614518036, 4.541064518000418104, 2.621784821874999949 ) ) ;
#42994 = CARTESIAN_POINT ( 'NONE',  ( 26.55937500061451573, 4.119189519843966529, -2.378215178124998275 ) ) ;
#42995 = CARTESIAN_POINT ( 'NONE',  ( 21.66562500061451502, 3.027376345333611329, 5.243569643749999010 ) ) ;
#42996 = CARTESIAN_POINT ( 'NONE',  ( 8.521875000614516082, 2.746126346562645981, -4.756430356249997438 ) ) ;
#42997 = CARTESIAN_POINT ( 'NONE',  ( 1.878215178124997609, 17.06562499938548072, 33.25316411605952993 ) ) ;
#42998 = CARTESIAN_POINT ( 'NONE',  ( 17.07187500061451502, 3.027376345333613106, -5.243569643749998122 ) ) ;
#42999 = CARTESIAN_POINT ( 'NONE',  ( 15.64687500061451608, -3.027376345333610441, -5.243569643749999898 ) ) ;
#43000 = CARTESIAN_POINT ( 'NONE',  ( 25.95937500061451431, -4.541064518000417216, -2.621784821875001281 ) ) ;
#43001 = CARTESIAN_POINT ( 'NONE',  ( 4.243569643749999898, 13.74687500061451750, 32.45002607614398471 ) ) ;
#43002 = CARTESIAN_POINT ( 'NONE',  ( 4.565625000614516260, 3.027376345333611329, 5.243569643749999010 ) ) ;
#43003 = CARTESIAN_POINT ( 'NONE',  ( 16.57500000122903216, 2.886751345948161074, 4.999999999999941380 ) ) ;
#43004 = EDGE_CURVE ( 'NONE', #41088, #42194, #12807, .T. ) ;
#43005 = VECTOR ( 'NONE', #11283, 1000.000000000000000 ) ;
#43006 = CARTESIAN_POINT ( 'NONE',  ( 3.384375000614517237, -4.541064518000419881, 2.621784821874995952 ) ) ;
#43007 = CARTESIAN_POINT ( 'NONE',  ( 2.000000000000000444, 15.27500000000000036, 26.53589838486224650 ) ) ;
#43008 = CARTESIAN_POINT ( 'NONE',  ( -1.999999999999997113, 18.72500000000000142, 33.46410161513775705 ) ) ;
#43009 = CARTESIAN_POINT ( 'NONE',  ( 8.334375000614516082, -4.541064518000419881, 2.621784821874995952 ) ) ;
#43010 = DIRECTION ( 'NONE',  ( 1.000000000000000000, 0.000000000000000000, 0.000000000000000000 ) ) ;
#43011 = CARTESIAN_POINT ( 'NONE',  ( 15.30000000122903359, -2.886751345948129988, 4.999999999999997335 ) ) ;
#43012 = CARTESIAN_POINT ( 'NONE',  ( 8.700000001229032165, -2.886751345948125991, -5.000000000000000000 ) ) ;
#43013 = CARTESIAN_POINT ( 'NONE',  ( 5.615625000614517859, -6.054752690667223547, -1.112240025338166033E-15 ) ) ;
#43014 = CARTESIAN_POINT ( 'NONE',  ( -8.484601909799255319E-16, 17.28124999877096712, 34.61880215351700940 ) ) ;
#43015 = CARTESIAN_POINT ( 'NONE',  ( 21.16875000122903216, -5.773502691896255534, -1.060575238724906372E-15 ) ) ;
#43016 = CARTESIAN_POINT ( 'NONE',  ( 15.34687500061451537, 6.054752690667223547, 3.707466751127219781E-16 ) ) ;
#43017 = CARTESIAN_POINT ( 'NONE',  ( 21.15000000000000213, -4.330127018922190985, -2.500000000000001332 ) ) ;
#43018 = ORIENTED_EDGE ( 'NONE', *, *, #9782, .F. ) ;
#43019 = CARTESIAN_POINT ( 'NONE',  ( 21.59062500061451928, 6.054752690667223547, 3.707466751127219781E-16 ) ) ;
#43020 = CARTESIAN_POINT ( 'NONE',  ( 6.440625000614517148, -3.027376345333614438, 5.243569643749998122 ) ) ;
#43021 = CARTESIAN_POINT ( 'NONE',  ( 23.63437500061451502, -4.541064518000419881, 2.621784821874995952 ) ) ;
#43022 = CARTESIAN_POINT ( 'NONE',  ( 7.415625000614516793, -6.054752690667223547, -1.112240025338166033E-15 ) ) ;
#43023 = CARTESIAN_POINT ( 'NONE',  ( 23.23125000122903216, 4.330127018922191873, 2.499999999999999556 ) ) ;
#43024 = CARTESIAN_POINT ( 'NONE',  ( 7.425000001229034474, 2.886751345948129099, -4.999999999999998224 ) ) ;
#43025 = CARTESIAN_POINT ( 'NONE',  ( 21.89062500061451289, -3.027376345333610441, -5.243569643749999898 ) ) ;
#43026 = CARTESIAN_POINT ( 'NONE',  ( 4.243569643749999898, 10.12812500061451715, -30.00000000000000000 ) ) ;
#43027 = CARTESIAN_POINT ( 'NONE',  ( 9.225000001229034297, 2.886751345948129099, -4.999999999999998224 ) ) ;
#43028 = CARTESIAN_POINT ( 'NONE',  ( 19.30312500061451786, 4.541064518000418104, -2.621784821874998173 ) ) ;
#43029 = CARTESIAN_POINT ( 'NONE',  ( 18.55312500061451431, 0.000000000000000000, 5.243569643749999010 ) ) ;
#43030 = CARTESIAN_POINT ( 'NONE',  ( 29.10937500061451644, -4.119189519843965641, -2.378215178125001383 ) ) ;
#43031 = CARTESIAN_POINT ( 'NONE',  ( 17.02499999999999858, -4.330127018922194537, 2.499999999999995559 ) ) ;
#43032 = CARTESIAN_POINT ( 'NONE',  ( 11.92500000122903181, 2.886751345948129099, -4.999999999999998224 ) ) ;
#43033 =( BOUNDED_SURFACE ( )  B_SPLINE_SURFACE ( 1, 2, ( 
 ( #12010, #7825, #17182, #58412, #2647, #25166, #29005, #40100, #45996, #30360, #13723, #41801, #68175, #57063, #47707, #19246, #23450, #62613, #3012, #34170, #70246, #580, #64330, #62970, #23085, #58779, #36624, #17538, #34533, #6470, #19618, #2287, #47347, #25542, #64700, #51542, #11655, #68533, #67808, #24804, #14084, #17894, #36264, #12366, #6107, #34901, #69881, #8188, #59145, #8554, #31081, #62258, #36988, #43642, #10384, #32916, #55453, #26653, #15181, #4124, #15542, #32188, #53996, #65800, #4846, #42904, #48454, #49189, #71719, #21091, #54721, #44009, #8924, #38459, #54361, #43279, #65428, #48816, #37720, #31454, #48085, #70611, #19984, #59883, #66166, #3755, #55090, #60240, #9289, #27019, #60985, #42537, #65063, #49551, #38086, #71346, #3393, #60608, #25914, #10017, #20721, #14454, #4490, #59510, #31822, #14818, #70978, #20353, #26279, #9654, #37361, #32553, #72073, #21454, #66531, #15911, #50284, #72808, #67279, #22191, #16278, #28819, #11107, #57246, #27380, #61349, #16638, #12189, #38834, #33996, #10745, #61708, #43, #67991, #760, #39193, #45459, #11473, #51357, #33278, #55817, #44745, #23268, #33636, #56180, #5573, #67631, #28110, #50639, #22548, #21820, #68354, #11834, #56533, #45818, #17715, #28460, #45096, #40275, #17365, #5926, #5204, #49912, #44385, #16998, #39555, #27745, #62080, #50995, #393, #39922, #62436, #22900, #34352, #34716, #56885, #6290, #72436, #62796, #66910, #46907, #57967, #42095, #1487, #70160, #23993, #69446, #36179, #69800, #58696, #63523, #24723, #2564, #12552, #52807, #29906, #35443, #64617, #64247, #13635, #46178, #35086, #47266, #19166, #18803, #52446, #25084, #51722, #8107, #18077, #1851, #2208, #41367, #40638, #29188, #30635, #7375, #46540, #69082, #53167, #63157, #6659, #24359, #47627, #41720, #19537, #14003, #36542, #18443, #63877, #1123, #13268, #23632, #68717, #41008, #52082, #35806, #58328, #57612, #7015, #29546, #12910, #7739, #30274, #65344, #31372, #43925, #25460, #60525, #64982, #54633, #31739, #42459, #49104, #26938, #19907, #9569, #4040, #26564, #71633, #9931, #71997, #48004, #71257, #32470, #21371, #70896, #21006, #43558, #14373, #70532, #66451, #8467, #15828, #36908, #20637, #14734, #66080, #43194, #59428, #8836, #53913, #31002, #37276, #65714, #3306, #53535, #15458, #59798, #25833, #48370, #55003, #20269, #59062, #54277, #38003, #4409, #49463, #2931, #42821, #9204, #15100, #3671, #48734, #26194, #37636, #60159, #32101, #16556, #28029, #56456, #11393, #38749, #27660, #17282, #61993, #44665, #10663, #23187, #4764, #39843, #44297, #33913, #11027, #21736, #28378, #6208, #72355, #5846, #50915, #313, #22823, #62357, #51277, #27297, #50557, #11753, #680, #50199, #45375, #67911, #66825, #49831, #45741, #60897, #68276, #16198, #73085, #67195, #34270, #22466, #61269, #33193, #55732, #10301, #39108, #39470, #33549, #56803, #28736, #45016, #5126, #32833, #55371, #72724, #22107, #61624, #56099, #5490, #67552, #38372, #16915, #40931, #57537, #2480, #29468, #1405, #17638, #69719, #7298, #57889, #69000, #53085, #12478, #8023, #35006, #29828, #47187, #7655, #19087, #23914, #35728, #13549, #23552, #63799, #63446, #46462, #25005, #2130, #24641, #57165, #46100, #58250, #30194, #52363, #12832, #36096, #62719, #41642, #29109, #35366, #13189, #6937, #1767, #52004, #18361, #40558, #12113, #58616, #64161, #24281, #30559, #47547, #68637, #17999, #40198, #46829, #69366, #34636, #6578, #63076, #51643, #18724, #1044, #41288, #52724, #25749, #43105, #42740, #13925, #48286, #31285, #8752, #70810, #26479, #20924, #59341, #58979, #65631, #32380, #54920, #4327, #48650, #37190, #26111, #37556, #54192, #2846, #14649, #26852, #64899, #70449, #71175, #20547, #15018, #3589, #66000, #30915, #60441, #3220, #65259, #14289, #20185, #59714, #53456, #70076, #19451, #42011, #53827, #60078, #9121, #3956, #31658, #9489, #49019, #9851, #64531, #36463, #71550, #32018, #54554, #25375, #43476, #47920, #15381, #37923, #8385, #19825, #42377, #36826, #16113, #27214, #15744, #55648, #10944, #6125, #56723, #21654, #10583, #67113, #33110, #72277, #44211, #38665, #66743, #38283, #50835, #5044, #49384, #71915, #10219, #61188, #34189, #60811, #56013, #32752, #27580, #22024, #16836, #22743, #50112, #67473, #33466, #235, #55290, #4684, #72641, #45293, #44581, #16470, #43842, #39028, #61542, #49749, #5406, #27943, #50476, #39390, #61909, #73002, #22386, #21289, #44935, #11314, #66369, #28300, #33835, #56377, #5769, #11673, #67827, #39761, #17200, #62278, #58160, #18636, #7564, #12383, #46740, #24552, #34552, #1677, #51918, #57446, #13453, #13100, #35638, #68193, #57080, #69274, #41200, #18267, #1315, #47098, #598, #30100, #40117, #23824, #24186, #40840, #62633, #51195, #52635, #6850, #23469, #46015, #2041, #12027, #28656, #46375, #69630, #63708, #18992, #41554, #64071, #68552, #63358, #23103, #12742, #36001, #58520, #62988, #960, #29384, #35278, #45660, #17556, #29023, #17910, #6488, #52275, #34919, #40473, #51559, #68909, #57800, #7209, #29738, #53734, #64440, #71085, #48929, #41915, #31564, #26020, #3501, #48559, #9399, #20834, #47455, #20090, #31929, #43387, #19732, #20459, #43013, #13832, #19358, #65911, #30468, #15291, #58887, #42647, #36731, #65542, #65171, #36371, #8297, #69988, #52997, #14196, #9034, #3127, #54466, #14929, #14562, #30827, #2393, #37469, #59989, #70715, #31192, #26387, #24912, #3864, #53360, #25656, #71458, #37095, #2757, #25279, #37830, #59253, #47825, #70355, #7930, #42282, #64806, #48192, #8661, #59620, #54103, #28217, #33746, #4595, #72548, #9759, #50023, #22297, #44849, #21566, #32661, #38572, #21935, #5317, #33385, #60719, #49659, #39304, #10851, #66647, #55202, #45205, #26762, #61817, #66275, #55921, #33022, #43750, #50390, #50746 ),
 ( #44491, #16024, #67385, #67024, #21198, #15653, #49294, #32293, #61096, #61457, #55560, #11222, #72915, #16384, #38192, #54828, #4235, #27125, #72187, #10129, #10494, #44120, #38939, #16747, #27859, #4956, #27489, #67738, #56291, #5681, #60350, #149, #22655, #17111, #71827, #1958, #34465, #30009, #56993, #29296, #69189, #29651, #18549, #23378, #57717, #35552, #45573, #12657, #62900, #68458, #24465, #24101, #46649, #6037, #68104, #1591, #505, #51108, #47013, #62190, #69548, #17470, #51826, #17820, #41114, #23735, #23015, #40030, #28571, #11586, #45926, #40750, #12295, #63624, #52189, #46283, #62543, #34103, #56642, #11940, #6400, #28932, #40381, #51468, #1229, #13014, #7122, #34830, #871, #39670, #57356, #6762, #68824, #58071, #18181, #63265, #35192, #7481, #52552, #9311, #13746, #8575, #48475, #8945, #70999, #2670, #37010, #14842, #24825, #65085, #42197, #47730, #3776, #3415, #25935, #58436, #47372, #59533, #31477, #31103, #64721, #37383, #63987, #20375, #30383, #14105, #14476, #53643, #52912, #41468, #42926, #70269, #36287, #58801, #65450, #2310, #18907, #36645, #59906, #54019, #31845, #54381, #26301, #8211, #3035, #13369, #25566, #48838, #35911, #53272, #64355, #19641, #48107, #7847, #69903, #19269, #30740, #41823, #42558, #25187, #59167, #70630, #20005, #691, #4145, #67923, #45029, #54743, #62369, #40209, #32209, #22835, #17295, #39857, #11767, #23199, #12123, #37742, #11407, #45753, #34650, #10042, #34283, #26677, #56815, #67564, #65822, #6222, #43302, #32576, #38109, #49209, #60262, #5502, #33926, #29121, #6592, #43666, #55114, #16929, #28041, #21113, #66188, #60630, #15566, #9676, #68289, #50570, #71369, #20744, #71743, #73097, #57178, #22479, #5859, #39483, #62006, #56468, #28750, #17649, #28391, #51290, #50929, #62731, #326, #45387, #15204, #25016, #18376, #57901, #40944, #18735, #63458, #35378, #1419, #46112, #19464, #36107, #35741, #2492, #47558, #57547, #29481, #70087, #13201, #30205, #36473, #30570, #52018, #68649, #23925, #8397, #58260, #42022, #7310, #24652, #24292, #18013, #29840, #12845, #52375, #1781, #8035, #64543, #46840, #40570, #47198, #13936, #58991, #51655, #52736, #41299, #7666, #19098, #2141, #6949, #69380, #1057, #46475, #69013, #69729, #41653, #64174, #13562, #23567, #12491, #63090, #63809, #58628, #53096, #35018, #48660, #64910, #38293, #66378, #15754, #42750, #3967, #59724, #37932, #71185, #65271, #9860, #21299, #43853, #2858, #32390, #26489, #54202, #59352, #49031, #15029, #14300, #36838, #19836, #25388, #37201, #32028, #3599, #54930, #20935, #37566, #8763, #53467, #47932, #3233, #25760, #31297, #9132, #48296, #20558, #43486, #71560, #26121, #70822, #60822, #14658, #31669, #30926, #4337, #43116, #65641, #60090, #70461, #20196, #42388, #9499, #54564, #60452, #66010, #26862, #15390, #49393, #71924, #53838, #56391, #33477, #39040, #68209, #67842, #17214, #49760, #16124, #28312, #22756, #73015, #56026, #28671, #55299, #11688, #21664, #5418, #5781, #22399, #44221, #32762, #39776, #61554, #5054, #27591, #56738, #66754, #10228, #27957, #62292, #248, #45307, #51211, #6140, #50123, #44948, #4693, #67485, #34204, #611, #44594, #55658, #10956, #16848, #50848, #23118, #10593, #72654, #45673, #33847, #16483, #22035, #17570, #72286, #40132, #38677, #27223, #50489, #61198, #33121, #67125, #39404, #61921, #11327, #58174, #7579, #64086, #2406, #29039, #1691, #13468, #24927, #1329, #30114, #24567, #23483, #973, #47470, #12043, #70002, #40488, #24201, #18280, #47112, #52649, #2055, #36016, #19372, #51574, #46754, #58534, #62646, #23841, #69644, #19006, #46030, #68566, #34566, #57095, #6503, #63003, #69289, #40856, #41568, #18652, #17925, #12398, #34934, #57460, #68924, #63722, #35293, #7946, #30483, #41214, #6866, #29398, #51932, #46389, #63373, #12757, #57814, #7224, #52290, #53012, #29753, #13114, #35654, #26776, #53747, #25670, #41929, #20848, #31579, #9048, #20106, #4251, #36747, #32308, #59267, #54118, #71472, #31944, #43401, #48207, #60004, #37844, #47840, #14945, #65186, #70729, #49308, #26401, #48944, #8312, #70369, #9414, #54480, #3514, #14576, #60365, #13846, #65926, #53375, #37109, #37483, #26034, #2771, #64455, #15306, #42661, #8675, #31206, #9774, #25294, #36386, #59635, #54842, #3880, #71842, #58900, #30841, #3144, #48573, #19747, #71101, #42296, #64821, #20474, #14210, #43027, #65555, #39320, #67401, #21581, #10509, #164, #44865, #27504, #66662, #6051, #60735, #22669, #27141, #16762, #67040, #4611, #11238, #62204, #55216, #61833, #33760, #72204, #10144, #50037, #55937, #51123, #28586, #16039, #55577, #38954, #4970, #44135, #38587, #61113, #33037, #32677, #45220, #72563, #21213, #43766, #49675, #21949, #66290, #44506, #27873, #16400, #61472, #10867, #56305, #67753, #33400, #5694, #5332, #17125, #50406, #72930, #22312, #39685, #28230, #50760, #11600, #34117, #56657, #15669, #38207, #45586, #58086, #24115, #68838, #41129, #63639, #34480, #6415, #13028, #18195, #63280, #52565, #18563, #28947, #68119, #886, #24481, #40766, #35567, #12310, #57731, #6779, #17485, #34845, #17835, #40396, #57371, #69204, #7494, #68473, #40047, #7137, #1972, #30022, #520, #12672, #23750, #35209, #52203, #29667, #57010, #1245, #23031, #29311, #62915, #1604, #46664, #62559, #11955, #51486, #51842, #23393, #45942, #46299, #10729, #67261, #11089, #27363, #745, #28802, #51343, #5189, #39538, #22173, #376, #33617, #27727, #45442, #56870, #6274, #38441, #67975, #62063, #16619, #21802, #11457, #49894, #56517, #39174, #60967, #22884, #10367, #50265, #33261, #72790, #61690, #33978, #39907, #55799, #5910, #50621, #17348, #72419, #44366, #61331, #62420, #44726, #56161, #5556, #28093, #26, #22532, #16261, #32897, #34336, #50979, #45079, #11819, #23254, #66893 ) ),
 .UNSPECIFIED., .F., .F., .F. ) 
 B_SPLINE_SURFACE_WITH_KNOTS ( ( 2, 2 ),
 ( 3, 2, 2, 2, 2, 2, 2, 2, 2, 2, 2, 2, 2, 2, 2, 2, 2, 2, 2, 2, 2, 2, 2, 2, 2, 2, 2, 2, 2, 2, 2, 2, 2, 2, 2, 2, 2, 2, 2, 2, 2, 2, 2, 2, 2, 2, 2, 2, 2, 2, 2, 2, 2, 2, 2, 2, 2, 2, 2, 2, 2, 2, 2, 2, 2, 2, 2, 2, 2, 2, 2, 2, 2, 2, 2, 2, 2, 2, 2, 2, 2, 2, 2, 2, 2, 2, 2, 2, 2, 2, 2, 2, 2, 2, 2, 2, 2, 2, 2, 2, 2, 2, 2, 2, 2, 2, 2, 2, 2, 2, 2, 2, 2, 2, 2, 2, 2, 2, 2, 2, 2, 2, 2, 2, 2, 2, 2, 2, 2, 2, 2, 2, 2, 2, 2, 2, 2, 2, 2, 2, 2, 2, 2, 2, 2, 2, 2, 2, 2, 2, 2, 2, 2, 2, 2, 2, 2, 2, 2, 2, 2, 2, 2, 2, 2, 2, 2, 2, 2, 2, 2, 2, 2, 2, 2, 2, 2, 2, 2, 2, 2, 2, 2, 2, 2, 2, 2, 2, 2, 2, 2, 2, 2, 2, 2, 2, 2, 2, 2, 2, 2, 2, 2, 2, 2, 2, 2, 2, 2, 2, 2, 2, 2, 2, 2, 2, 2, 2, 2, 2, 2, 2, 2, 2, 2, 2, 2, 2, 2, 2, 2, 2, 2, 2, 2, 2, 2, 2, 2, 2, 2, 2, 2, 2, 2, 2, 2, 2, 2, 2, 2, 2, 2, 2, 2, 2, 2, 2, 2, 2, 2, 2, 2, 2, 2, 2, 2, 2, 2, 2, 2, 2, 2, 2, 2, 2, 2, 2, 2, 2, 2, 2, 2, 2, 2, 2, 2, 2, 2, 2, 2, 2, 2, 2, 2, 2, 2, 2, 2, 2, 2, 2, 2, 2, 2, 2, 2, 2, 2, 2, 2, 2, 2, 2, 2, 2, 2, 2, 2, 2, 2, 2, 2, 2, 2, 2, 2, 2, 2, 2, 2, 2, 2, 2, 2, 2, 2, 2, 2, 2, 2, 2, 2, 2, 2, 2, 2, 2, 2, 2, 2, 2, 2, 2, 2, 2, 2, 2, 2, 2, 3 ),
 ( 0.000000000000000000, 1.000000000000000000 ),
 ( 0.000000000000000000, 0.002777777777777777884, 0.005555555555555555768, 0.008333333333333333218, 0.01111111111111111154, 0.01388888888888888812, 0.01666666666666666644, 0.01944444444444444475, 0.02222222222222222307, 0.02500000000000000139, 0.02777777777777777624, 0.03055555555555555455, 0.03333333333333333287, 0.03611111111111110772, 0.03888888888888888951, 0.04166666666666666435, 0.04444444444444444614, 0.04722222222222222099, 0.05000000000000000278, 0.05277777777777777762, 0.05555555555555555247, 0.05833333333333333426, 0.06111111111111110911, 0.06388888888888888395, 0.06666666666666666574, 0.06944444444444444753, 0.07222222222222221544, 0.07499999999999999722, 0.07777777777777777901, 0.08055555555555556080, 0.08333333333333332871, 0.08611111111111111049, 0.08888888888888889228, 0.09166666666666666019, 0.09444444444444444198, 0.09722222222222222376, 0.1000000000000000056, 0.1027777777777777735, 0.1055555555555555552, 0.1083333333333333370, 0.1111111111111111049, 0.1138888888888888867, 0.1166666666666666685, 0.1194444444444444503, 0.1222222222222222182, 0.1250000000000000000, 0.1277777777777777679, 0.1305555555555555636, 0.1333333333333333315, 0.1361111111111110994, 0.1388888888888888951, 0.1416666666666666630, 0.1444444444444444309, 0.1472222222222222265, 0.1499999999999999944, 0.1527777777777777901, 0.1555555555555555580, 0.1583333333333333259, 0.1611111111111111216, 0.1638888888888888895, 0.1666666666666666574, 0.1694444444444444531, 0.1722222222222222210, 0.1749999999999999889, 0.1777777777777777846, 0.1805555555555555525, 0.1833333333333333204, 0.1861111111111111160, 0.1888888888888888840, 0.1916666666666666796, 0.1944444444444444475, 0.1972222222222222154, 0.2000000000000000111, 0.2027777777777777790, 0.2055555555555555469, 0.2083333333333333426, 0.2111111111111111105, 0.2138888888888888784, 0.2166666666666666741, 0.2194444444444444420, 0.2222222222222222099, 0.2250000000000000056, 0.2277777777777777735, 0.2305555555555555691, 0.2333333333333333370, 0.2361111111111111049, 0.2388888888888889006, 0.2416666666666666685, 0.2444444444444444364, 0.2472222222222222321, 0.2500000000000000000, 0.2527777777777777679, 0.2555555555555555358, 0.2583333333333333592, 0.2611111111111111271, 0.2638888888888888951, 0.2666666666666666630, 0.2694444444444444309, 0.2722222222222221988, 0.2750000000000000222, 0.2777777777777777901, 0.2805555555555555580, 0.2833333333333333259, 0.2861111111111110938, 0.2888888888888888618, 0.2916666666666666852, 0.2944444444444444531, 0.2972222222222222210, 0.2999999999999999889, 0.3027777777777777568, 0.3055555555555555802, 0.3083333333333333481, 0.3111111111111111160, 0.3138888888888888840, 0.3166666666666666519, 0.3194444444444444198, 0.3222222222222222432, 0.3250000000000000111, 0.3277777777777777790, 0.3305555555555555469, 0.3333333333333333148, 0.3361111111111111382, 0.3388888888888889062, 0.3416666666666666741, 0.3444444444444444420, 0.3472222222222222099, 0.3499999999999999778, 0.3527777777777778012, 0.3555555555555555691, 0.3583333333333333370, 0.3611111111111111049, 0.3638888888888888729, 0.3666666666666666408, 0.3694444444444444642, 0.3722222222222222321, 0.3750000000000000000, 0.3777777777777777679, 0.3805555555555555358, 0.3833333333333333592, 0.3861111111111111271, 0.3888888888888888951, 0.3916666666666666630, 0.3944444444444444309, 0.3972222222222221988, 0.4000000000000000222, 0.4027777777777777901, 0.4055555555555555580, 0.4083333333333333259, 0.4111111111111110938, 0.4138888888888888618, 0.4166666666666666852, 0.4194444444444444531, 0.4222222222222222210, 0.4249999999999999889, 0.4277777777777777568, 0.4305555555555555802, 0.4333333333333333481, 0.4361111111111111160, 0.4388888888888888840, 0.4416666666666666519, 0.4444444444444444198, 0.4472222222222222432, 0.4500000000000000111, 0.4527777777777777790, 0.4555555555555555469, 0.4583333333333333148, 0.4611111111111111382, 0.4638888888888889062, 0.4666666666666666741, 0.4694444444444444420, 0.4722222222222222099, 0.4749999999999999778, 0.4777777777777778012, 0.4805555555555555691, 0.4833333333333333370, 0.4861111111111111049, 0.4888888888888888729, 0.4916666666666666408, 0.4944444444444444642, 0.4972222222222222321, 0.5000000000000000000, 0.5027777777777777679, 0.5055555555555555358, 0.5083333333333333037, 0.5111111111111110716, 0.5138888888888888395, 0.5166666666666667185, 0.5194444444444444864, 0.5222222222222222543, 0.5250000000000000222, 0.5277777777777777901, 0.5305555555555555580, 0.5333333333333333259, 0.5361111111111110938, 0.5388888888888888618, 0.5416666666666666297, 0.5444444444444443976, 0.5472222222222222765, 0.5500000000000000444, 0.5527777777777778123, 0.5555555555555555802, 0.5583333333333333481, 0.5611111111111111160, 0.5638888888888888840, 0.5666666666666666519, 0.5694444444444444198, 0.5722222222222221877, 0.5749999999999999556, 0.5777777777777777235, 0.5805555555555556024, 0.5833333333333333703, 0.5861111111111111382, 0.5888888888888889062, 0.5916666666666666741, 0.5944444444444444420, 0.5972222222222222099, 0.5999999999999999778, 0.6027777777777777457, 0.6055555555555555136, 0.6083333333333332815, 0.6111111111111111605, 0.6138888888888889284, 0.6166666666666666963, 0.6194444444444444642, 0.6222222222222222321, 0.6250000000000000000, 0.6277777777777777679, 0.6305555555555555358, 0.6333333333333333037, 0.6361111111111110716, 0.6388888888888888395, 0.6416666666666667185, 0.6444444444444444864, 0.6472222222222222543, 0.6500000000000000222, 0.6527777777777777901, 0.6555555555555555580, 0.6583333333333333259, 0.6611111111111110938, 0.6638888888888888618, 0.6666666666666666297, 0.6694444444444443976, 0.6722222222222222765, 0.6750000000000000444, 0.6777777777777778123, 0.6805555555555555802, 0.6833333333333333481, 0.6861111111111111160, 0.6888888888888888840, 0.6916666666666666519, 0.6944444444444444198, 0.6972222222222221877, 0.6999999999999999556, 0.7027777777777777235, 0.7055555555555556024, 0.7083333333333333703, 0.7111111111111111382, 0.7138888888888889062, 0.7166666666666666741, 0.7194444444444444420, 0.7222222222222222099, 0.7249999999999999778, 0.7277777777777777457, 0.7305555555555555136, 0.7333333333333332815, 0.7361111111111111605, 0.7388888888888889284, 0.7416666666666666963, 0.7444444444444444642, 0.7472222222222222321, 0.7500000000000000000, 0.7527777777777777679, 0.7555555555555555358, 0.7583333333333333037, 0.7611111111111110716, 0.7638888888888888395, 0.7666666666666667185, 0.7694444444444444864, 0.7722222222222222543, 0.7750000000000000222, 0.7777777777777777901, 0.7805555555555555580, 0.7833333333333333259, 0.7861111111111110938, 0.7888888888888888618, 0.7916666666666666297, 0.7944444444444443976, 0.7972222222222222765, 0.8000000000000000444, 0.8027777777777778123, 0.8055555555555555802, 0.8083333333333333481, 0.8111111111111111160, 0.8138888888888888840, 0.8166666666666666519, 0.8194444444444444198, 0.8222222222222221877, 0.8249999999999999556, 0.8277777777777777235, 0.8305555555555556024, 0.8333333333333333703, 0.8361111111111111382, 0.8388888888888889062, 0.8416666666666666741, 0.8444444444444444420, 0.8472222222222222099, 0.8499999999999999778, 0.8527777777777777457, 0.8555555555555555136, 0.8583333333333332815, 0.8611111111111111605, 0.8638888888888889284, 0.8666666666666666963, 0.8694444444444444642, 0.8722222222222222321, 0.8750000000000000000, 0.8777777777777777679, 0.8805555555555555358, 0.8833333333333333037, 0.8861111111111110716, 0.8888888888888888395, 0.8916666666666667185, 0.8944444444444444864, 0.8972222222222222543, 0.9000000000000000222, 0.9027777777777777901, 0.9055555555555555580, 0.9083333333333333259, 0.9111111111111110938, 0.9138888888888888618, 0.9166666666666666297, 0.9194444444444443976, 0.9222222222222222765, 0.9250000000000000444, 0.9277777777777778123, 0.9305555555555555802, 0.9333333333333333481, 0.9361111111111111160, 0.9388888888888888840, 0.9416666666666666519, 0.9444444444444444198, 0.9472222222222221877, 0.9499999999999999556, 0.9527777777777777235, 0.9555555555555556024, 0.9583333333333333703, 0.9611111111111111382, 0.9638888888888889062, 0.9666666666666666741, 0.9694444444444444420, 0.9722222222222222099, 0.9749999999999999778, 0.9777777777777777457, 0.9805555555555555136, 0.9833333333333332815, 0.9861111111111111605, 0.9888888888888889284, 0.9916666666666666963, 0.9944444444444444642, 0.9972222222222222321, 1.000000000000000000 ),
 .UNSPECIFIED. ) 
 GEOMETRIC_REPRESENTATION_ITEM ( )  RATIONAL_B_SPLINE_SURFACE ( (
 ( 1.000000000000000000, 0.8660254037844387076, 1.000000000000000000, 0.8660254037844387076, 1.000000000000000000, 0.8660254037844387076, 1.000000000000000000, 0.8660254037844387076, 1.000000000000000000, 0.8660254037844387076, 1.000000000000000000, 0.8660254037844387076, 1.000000000000000000, 0.8660254037844387076, 1.000000000000000000, 0.8660254037844387076, 1.000000000000000000, 0.8660254037844387076, 1.000000000000000000, 0.8660254037844387076, 1.000000000000000000, 0.8660254037844387076, 1.000000000000000000, 0.8660254037844387076, 1.000000000000000000, 0.8660254037844387076, 1.000000000000000000, 0.8660254037844387076, 1.000000000000000000, 0.8660254037844387076, 1.000000000000000000, 0.8660254037844387076, 1.000000000000000000, 0.8660254037844387076, 1.000000000000000000, 0.8660254037844387076, 1.000000000000000000, 0.8660254037844387076, 1.000000000000000000, 0.8660254037844387076, 1.000000000000000000, 0.8660254037844387076, 1.000000000000000000, 0.8660254037844387076, 1.000000000000000000, 0.8660254037844387076, 1.000000000000000000, 0.8660254037844387076, 1.000000000000000000, 0.8660254037844387076, 1.000000000000000000, 0.8660254037844387076, 1.000000000000000000, 0.8660254037844387076, 1.000000000000000000, 0.8660254037844387076, 1.000000000000000000, 0.8660254037844387076, 1.000000000000000000, 0.8660254037844387076, 1.000000000000000000, 0.8660254037844387076, 1.000000000000000000, 0.8660254037844387076, 1.000000000000000000, 0.8660254037844387076, 1.000000000000000000, 0.8660254037844387076, 1.000000000000000000, 0.8660254037844387076, 1.000000000000000000, 0.8660254037844387076, 1.000000000000000000, 0.8660254037844387076, 1.000000000000000000, 0.8660254037844387076, 1.000000000000000000, 0.8660254037844387076, 1.000000000000000000, 0.8660254037844387076, 1.000000000000000000, 0.8660254037844387076, 1.000000000000000000, 0.8660254037844387076, 1.000000000000000000, 0.8660254037844387076, 1.000000000000000000, 0.8660254037844387076, 1.000000000000000000, 0.8660254037844387076, 1.000000000000000000, 0.8660254037844387076, 1.000000000000000000, 0.8660254037844387076, 1.000000000000000000, 0.8660254037844387076, 1.000000000000000000, 0.8660254037844387076, 1.000000000000000000, 0.8660254037844387076, 1.000000000000000000, 0.8660254037844387076, 1.000000000000000000, 0.8660254037844387076, 1.000000000000000000, 0.8660254037844387076, 1.000000000000000000, 0.8660254037844387076, 1.000000000000000000, 0.8660254037844387076, 1.000000000000000000, 0.8660254037844387076, 1.000000000000000000, 0.8660254037844387076, 1.000000000000000000, 0.8660254037844387076, 1.000000000000000000, 0.8660254037844387076, 1.000000000000000000, 0.8660254037844387076, 1.000000000000000000, 0.8660254037844387076, 1.000000000000000000, 0.8660254037844387076, 1.000000000000000000, 0.8660254037844387076, 1.000000000000000000, 0.8660254037844387076, 1.000000000000000000, 0.8660254037844387076, 1.000000000000000000, 0.8660254037844387076, 1.000000000000000000, 0.8660254037844387076, 1.000000000000000000, 0.8660254037844387076, 1.000000000000000000, 0.8660254037844387076, 1.000000000000000000, 0.8660254037844387076, 1.000000000000000000, 0.8660254037844387076, 1.000000000000000000, 0.8660254037844387076, 1.000000000000000000, 0.8660254037844387076, 1.000000000000000000, 0.8660254037844387076, 1.000000000000000000, 0.8660254037844387076, 1.000000000000000000, 0.8660254037844387076, 1.000000000000000000, 0.8660254037844387076, 1.000000000000000000, 0.8660254037844387076, 1.000000000000000000, 0.8660254037844387076, 1.000000000000000000, 0.8660254037844387076, 1.000000000000000000, 0.8660254037844387076, 1.000000000000000000, 0.8660254037844387076, 1.000000000000000000, 0.8660254037844387076, 1.000000000000000000, 0.8660254037844387076, 1.000000000000000000, 0.8660254037844387076, 1.000000000000000000, 0.8660254037844387076, 1.000000000000000000, 0.8660254037844387076, 1.000000000000000000, 0.8660254037844387076, 1.000000000000000000, 0.8660254037844387076, 1.000000000000000000, 0.8660254037844387076, 1.000000000000000000, 0.8660254037844387076, 1.000000000000000000, 0.8660254037844387076, 1.000000000000000000, 0.8660254037844387076, 1.000000000000000000, 0.8660254037844387076, 1.000000000000000000, 0.8660254037844387076, 1.000000000000000000, 0.8660254037844387076, 1.000000000000000000, 0.8660254037844387076, 1.000000000000000000, 0.8660254037844387076, 1.000000000000000000, 0.8660254037844387076, 1.000000000000000000, 0.8660254037844387076, 1.000000000000000000, 0.8660254037844387076, 1.000000000000000000, 0.8660254037844387076, 1.000000000000000000, 0.8660254037844387076, 1.000000000000000000, 0.8660254037844387076, 1.000000000000000000, 0.8660254037844387076, 1.000000000000000000, 0.8660254037844387076, 1.000000000000000000, 0.8660254037844387076, 1.000000000000000000, 0.8660254037844387076, 1.000000000000000000, 0.8660254037844387076, 1.000000000000000000, 0.8660254037844387076, 1.000000000000000000, 0.8660254037844387076, 1.000000000000000000, 0.8660254037844387076, 1.000000000000000000, 0.8660254037844387076, 1.000000000000000000, 0.8660254037844387076, 1.000000000000000000, 0.8660254037844387076, 1.000000000000000000, 0.8660254037844387076, 1.000000000000000000, 0.8660254037844387076, 1.000000000000000000, 0.8660254037844387076, 1.000000000000000000, 0.8660254037844387076, 1.000000000000000000, 0.8660254037844387076, 1.000000000000000000, 0.8660254037844387076, 1.000000000000000000, 0.8660254037844387076, 1.000000000000000000, 0.8660254037844387076, 1.000000000000000000, 0.8660254037844387076, 1.000000000000000000, 0.8660254037844387076, 1.000000000000000000, 0.8660254037844387076, 1.000000000000000000, 0.8660254037844387076, 1.000000000000000000, 0.8660254037844387076, 1.000000000000000000, 0.8660254037844387076, 1.000000000000000000, 0.8660254037844387076, 1.000000000000000000, 0.8660254037844387076, 1.000000000000000000, 0.8660254037844387076, 1.000000000000000000, 0.8660254037844387076, 1.000000000000000000, 0.8660254037844387076, 1.000000000000000000, 0.8660254037844387076, 1.000000000000000000, 0.8660254037844387076, 1.000000000000000000, 0.8660254037844387076, 1.000000000000000000, 0.8660254037844387076, 1.000000000000000000, 0.8660254037844387076, 1.000000000000000000, 0.8660254037844387076, 1.000000000000000000, 0.8660254037844387076, 1.000000000000000000, 0.8660254037844387076, 1.000000000000000000, 0.8660254037844387076, 1.000000000000000000, 0.8660254037844387076, 1.000000000000000000, 0.8660254037844387076, 1.000000000000000000, 0.8660254037844387076, 1.000000000000000000, 0.8660254037844387076, 1.000000000000000000, 0.8660254037844387076, 1.000000000000000000, 0.8660254037844387076, 1.000000000000000000, 0.8660254037844387076, 1.000000000000000000, 0.8660254037844387076, 1.000000000000000000, 0.8660254037844387076, 1.000000000000000000, 0.8660254037844387076, 1.000000000000000000, 0.8660254037844387076, 1.000000000000000000, 0.8660254037844387076, 1.000000000000000000, 0.8660254037844387076, 1.000000000000000000, 0.8660254037844387076, 1.000000000000000000, 0.8660254037844387076, 1.000000000000000000, 0.8660254037844387076, 1.000000000000000000, 0.8660254037844387076, 1.000000000000000000, 0.8660254037844387076, 1.000000000000000000, 0.8660254037844387076, 1.000000000000000000, 0.8660254037844387076, 1.000000000000000000, 0.8660254037844387076, 1.000000000000000000, 0.8660254037844387076, 1.000000000000000000, 0.8660254037844387076, 1.000000000000000000, 0.8660254037844387076, 1.000000000000000000, 0.8660254037844387076, 1.000000000000000000, 0.8660254037844387076, 1.000000000000000000, 0.8660254037844387076, 1.000000000000000000, 0.8660254037844387076, 1.000000000000000000, 0.8660254037844387076, 1.000000000000000000, 0.8660254037844387076, 1.000000000000000000, 0.8660254037844387076, 1.000000000000000000, 0.8660254037844387076, 1.000000000000000000, 0.8660254037844387076, 1.000000000000000000, 0.8660254037844387076, 1.000000000000000000, 0.8660254037844387076, 1.000000000000000000, 0.8660254037844387076, 1.000000000000000000, 0.8660254037844387076, 1.000000000000000000, 0.8660254037844387076, 1.000000000000000000, 0.8660254037844387076, 1.000000000000000000, 0.8660254037844387076, 1.000000000000000000, 0.8660254037844387076, 1.000000000000000000, 0.8660254037844387076, 1.000000000000000000, 0.8660254037844387076, 1.000000000000000000, 0.8660254037844387076, 1.000000000000000000, 0.8660254037844387076, 1.000000000000000000, 0.8660254037844387076, 1.000000000000000000, 0.8660254037844387076, 1.000000000000000000, 0.8660254037844387076, 1.000000000000000000, 0.8660254037844387076, 1.000000000000000000, 0.8660254037844387076, 1.000000000000000000, 0.8660254037844387076, 1.000000000000000000, 0.8660254037844387076, 1.000000000000000000, 0.8660254037844387076, 1.000000000000000000, 0.8660254037844387076, 1.000000000000000000, 0.8660254037844387076, 1.000000000000000000, 0.8660254037844387076, 1.000000000000000000, 0.8660254037844387076, 1.000000000000000000, 0.8660254037844387076, 1.000000000000000000, 0.8660254037844387076, 1.000000000000000000, 0.8660254037844387076, 1.000000000000000000, 0.8660254037844387076, 1.000000000000000000, 0.8660254037844387076, 1.000000000000000000, 0.8660254037844387076, 1.000000000000000000, 0.8660254037844387076, 1.000000000000000000, 0.8660254037844387076, 1.000000000000000000, 0.8660254037844387076, 1.000000000000000000, 0.8660254037844387076, 1.000000000000000000, 0.8660254037844387076, 1.000000000000000000, 0.8660254037844387076, 1.000000000000000000, 0.8660254037844387076, 1.000000000000000000, 0.8660254037844387076, 1.000000000000000000, 0.8660254037844387076, 1.000000000000000000, 0.8660254037844387076, 1.000000000000000000, 0.8660254037844387076, 1.000000000000000000, 0.8660254037844387076, 1.000000000000000000, 0.8660254037844387076, 1.000000000000000000, 0.8660254037844387076, 1.000000000000000000, 0.8660254037844387076, 1.000000000000000000, 0.8660254037844387076, 1.000000000000000000, 0.8660254037844387076, 1.000000000000000000, 0.8660254037844387076, 1.000000000000000000, 0.8660254037844387076, 1.000000000000000000, 0.8660254037844387076, 1.000000000000000000, 0.8660254037844387076, 1.000000000000000000, 0.8660254037844387076, 1.000000000000000000, 0.8660254037844387076, 1.000000000000000000, 0.8660254037844387076, 1.000000000000000000, 0.8660254037844387076, 1.000000000000000000, 0.8660254037844387076, 1.000000000000000000, 0.8660254037844387076, 1.000000000000000000, 0.8660254037844387076, 1.000000000000000000, 0.8660254037844387076, 1.000000000000000000, 0.8660254037844387076, 1.000000000000000000, 0.8660254037844387076, 1.000000000000000000, 0.8660254037844387076, 1.000000000000000000, 0.8660254037844387076, 1.000000000000000000, 0.8660254037844387076, 1.000000000000000000, 0.8660254037844387076, 1.000000000000000000, 0.8660254037844387076, 1.000000000000000000, 0.8660254037844387076, 1.000000000000000000, 0.8660254037844387076, 1.000000000000000000, 0.8660254037844387076, 1.000000000000000000, 0.8660254037844387076, 1.000000000000000000, 0.8660254037844387076, 1.000000000000000000, 0.8660254037844387076, 1.000000000000000000, 0.8660254037844387076, 1.000000000000000000, 0.8660254037844387076, 1.000000000000000000, 0.8660254037844387076, 1.000000000000000000, 0.8660254037844387076, 1.000000000000000000, 0.8660254037844387076, 1.000000000000000000, 0.8660254037844387076, 1.000000000000000000, 0.8660254037844387076, 1.000000000000000000, 0.8660254037844387076, 1.000000000000000000, 0.8660254037844387076, 1.000000000000000000, 0.8660254037844387076, 1.000000000000000000, 0.8660254037844387076, 1.000000000000000000, 0.8660254037844387076, 1.000000000000000000, 0.8660254037844387076, 1.000000000000000000, 0.8660254037844387076, 1.000000000000000000, 0.8660254037844387076, 1.000000000000000000, 0.8660254037844387076, 1.000000000000000000, 0.8660254037844387076, 1.000000000000000000, 0.8660254037844387076, 1.000000000000000000, 0.8660254037844387076, 1.000000000000000000, 0.8660254037844387076, 1.000000000000000000, 0.8660254037844387076, 1.000000000000000000, 0.8660254037844387076, 1.000000000000000000, 0.8660254037844387076, 1.000000000000000000, 0.8660254037844387076, 1.000000000000000000, 0.8660254037844387076, 1.000000000000000000, 0.8660254037844387076, 1.000000000000000000, 0.8660254037844387076, 1.000000000000000000, 0.8660254037844387076, 1.000000000000000000, 0.8660254037844387076, 1.000000000000000000, 0.8660254037844387076, 1.000000000000000000, 0.8660254037844387076, 1.000000000000000000, 0.8660254037844387076, 1.000000000000000000, 0.8660254037844387076, 1.000000000000000000, 0.8660254037844387076, 1.000000000000000000, 0.8660254037844387076, 1.000000000000000000, 0.8660254037844387076, 1.000000000000000000, 0.8660254037844387076, 1.000000000000000000, 0.8660254037844387076, 1.000000000000000000, 0.8660254037844387076, 1.000000000000000000, 0.8660254037844387076, 1.000000000000000000, 0.8660254037844387076, 1.000000000000000000, 0.8660254037844387076, 1.000000000000000000, 0.8660254037844387076, 1.000000000000000000, 0.8660254037844387076, 1.000000000000000000, 0.8660254037844387076, 1.000000000000000000, 0.8660254037844387076, 1.000000000000000000, 0.8660254037844387076, 1.000000000000000000, 0.8660254037844387076, 1.000000000000000000, 0.8660254037844387076, 1.000000000000000000, 0.8660254037844387076, 1.000000000000000000, 0.8660254037844387076, 1.000000000000000000, 0.8660254037844387076, 1.000000000000000000, 0.8660254037844387076, 1.000000000000000000, 0.8660254037844387076, 1.000000000000000000, 0.8660254037844387076, 1.000000000000000000, 0.8660254037844387076, 1.000000000000000000, 0.8660254037844387076, 1.000000000000000000, 0.8660254037844387076, 1.000000000000000000, 0.8660254037844387076, 1.000000000000000000, 0.8660254037844387076, 1.000000000000000000, 0.8660254037844387076, 1.000000000000000000, 0.8660254037844387076, 1.000000000000000000, 0.8660254037844387076, 1.000000000000000000, 0.8660254037844387076, 1.000000000000000000, 0.8660254037844387076, 1.000000000000000000, 0.8660254037844387076, 1.000000000000000000, 0.8660254037844387076, 1.000000000000000000, 0.8660254037844387076, 1.000000000000000000, 0.8660254037844387076, 1.000000000000000000, 0.8660254037844387076, 1.000000000000000000, 0.8660254037844387076, 1.000000000000000000, 0.8660254037844387076, 1.000000000000000000, 0.8660254037844387076, 1.000000000000000000, 0.8660254037844387076, 1.000000000000000000, 0.8660254037844387076, 1.000000000000000000, 0.8660254037844387076, 1.000000000000000000, 0.8660254037844387076, 1.000000000000000000, 0.8660254037844387076, 1.000000000000000000, 0.8660254037844387076, 1.000000000000000000, 0.8660254037844387076, 1.000000000000000000, 0.8660254037844387076, 1.000000000000000000, 0.8660254037844387076, 1.000000000000000000, 0.8660254037844387076, 1.000000000000000000, 0.8660254037844387076, 1.000000000000000000, 0.8660254037844387076, 1.000000000000000000, 0.8660254037844387076, 1.000000000000000000, 0.8660254037844387076, 1.000000000000000000, 0.8660254037844387076, 1.000000000000000000, 0.8660254037844387076, 1.000000000000000000, 0.8660254037844387076, 1.000000000000000000, 0.8660254037844387076, 1.000000000000000000, 0.8660254037844387076, 1.000000000000000000, 0.8660254037844387076, 1.000000000000000000, 0.8660254037844387076, 1.000000000000000000, 0.8660254037844387076, 1.000000000000000000, 0.8660254037844387076, 1.000000000000000000, 0.8660254037844387076, 1.000000000000000000, 0.8660254037844387076, 1.000000000000000000, 0.8660254037844387076, 1.000000000000000000, 0.8660254037844387076, 1.000000000000000000, 0.8660254037844387076, 1.000000000000000000, 0.8660254037844387076, 1.000000000000000000, 0.8660254037844387076, 1.000000000000000000, 0.8660254037844387076, 1.000000000000000000, 0.8660254037844387076, 1.000000000000000000, 0.8660254037844387076, 1.000000000000000000, 0.8660254037844387076, 1.000000000000000000, 0.8660254037844387076, 1.000000000000000000, 0.8660254037844387076, 1.000000000000000000, 0.8660254037844387076, 1.000000000000000000, 0.8660254037844387076, 1.000000000000000000, 0.8660254037844387076, 1.000000000000000000),
 ( 1.000000000000000000, 0.8660254037844387076, 1.000000000000000000, 0.8660254037844387076, 1.000000000000000000, 0.8660254037844387076, 1.000000000000000000, 0.8660254037844387076, 1.000000000000000000, 0.8660254037844387076, 1.000000000000000000, 0.8660254037844387076, 1.000000000000000000, 0.8660254037844387076, 1.000000000000000000, 0.8660254037844387076, 1.000000000000000000, 0.8660254037844387076, 1.000000000000000000, 0.8660254037844387076, 1.000000000000000000, 0.8660254037844387076, 1.000000000000000000, 0.8660254037844387076, 1.000000000000000000, 0.8660254037844387076, 1.000000000000000000, 0.8660254037844387076, 1.000000000000000000, 0.8660254037844387076, 1.000000000000000000, 0.8660254037844387076, 1.000000000000000000, 0.8660254037844387076, 1.000000000000000000, 0.8660254037844387076, 1.000000000000000000, 0.8660254037844387076, 1.000000000000000000, 0.8660254037844387076, 1.000000000000000000, 0.8660254037844387076, 1.000000000000000000, 0.8660254037844387076, 1.000000000000000000, 0.8660254037844387076, 1.000000000000000000, 0.8660254037844387076, 1.000000000000000000, 0.8660254037844387076, 1.000000000000000000, 0.8660254037844387076, 1.000000000000000000, 0.8660254037844387076, 1.000000000000000000, 0.8660254037844387076, 1.000000000000000000, 0.8660254037844387076, 1.000000000000000000, 0.8660254037844387076, 1.000000000000000000, 0.8660254037844387076, 1.000000000000000000, 0.8660254037844387076, 1.000000000000000000, 0.8660254037844387076, 1.000000000000000000, 0.8660254037844387076, 1.000000000000000000, 0.8660254037844387076, 1.000000000000000000, 0.8660254037844387076, 1.000000000000000000, 0.8660254037844387076, 1.000000000000000000, 0.8660254037844387076, 1.000000000000000000, 0.8660254037844387076, 1.000000000000000000, 0.8660254037844387076, 1.000000000000000000, 0.8660254037844387076, 1.000000000000000000, 0.8660254037844387076, 1.000000000000000000, 0.8660254037844387076, 1.000000000000000000, 0.8660254037844387076, 1.000000000000000000, 0.8660254037844387076, 1.000000000000000000, 0.8660254037844387076, 1.000000000000000000, 0.8660254037844387076, 1.000000000000000000, 0.8660254037844387076, 1.000000000000000000, 0.8660254037844387076, 1.000000000000000000, 0.8660254037844387076, 1.000000000000000000, 0.8660254037844387076, 1.000000000000000000, 0.8660254037844387076, 1.000000000000000000, 0.8660254037844387076, 1.000000000000000000, 0.8660254037844387076, 1.000000000000000000, 0.8660254037844387076, 1.000000000000000000, 0.8660254037844387076, 1.000000000000000000, 0.8660254037844387076, 1.000000000000000000, 0.8660254037844387076, 1.000000000000000000, 0.8660254037844387076, 1.000000000000000000, 0.8660254037844387076, 1.000000000000000000, 0.8660254037844387076, 1.000000000000000000, 0.8660254037844387076, 1.000000000000000000, 0.8660254037844387076, 1.000000000000000000, 0.8660254037844387076, 1.000000000000000000, 0.8660254037844387076, 1.000000000000000000, 0.8660254037844387076, 1.000000000000000000, 0.8660254037844387076, 1.000000000000000000, 0.8660254037844387076, 1.000000000000000000, 0.8660254037844387076, 1.000000000000000000, 0.8660254037844387076, 1.000000000000000000, 0.8660254037844387076, 1.000000000000000000, 0.8660254037844387076, 1.000000000000000000, 0.8660254037844387076, 1.000000000000000000, 0.8660254037844387076, 1.000000000000000000, 0.8660254037844387076, 1.000000000000000000, 0.8660254037844387076, 1.000000000000000000, 0.8660254037844387076, 1.000000000000000000, 0.8660254037844387076, 1.000000000000000000, 0.8660254037844387076, 1.000000000000000000, 0.8660254037844387076, 1.000000000000000000, 0.8660254037844387076, 1.000000000000000000, 0.8660254037844387076, 1.000000000000000000, 0.8660254037844387076, 1.000000000000000000, 0.8660254037844387076, 1.000000000000000000, 0.8660254037844387076, 1.000000000000000000, 0.8660254037844387076, 1.000000000000000000, 0.8660254037844387076, 1.000000000000000000, 0.8660254037844387076, 1.000000000000000000, 0.8660254037844387076, 1.000000000000000000, 0.8660254037844387076, 1.000000000000000000, 0.8660254037844387076, 1.000000000000000000, 0.8660254037844387076, 1.000000000000000000, 0.8660254037844387076, 1.000000000000000000, 0.8660254037844387076, 1.000000000000000000, 0.8660254037844387076, 1.000000000000000000, 0.8660254037844387076, 1.000000000000000000, 0.8660254037844387076, 1.000000000000000000, 0.8660254037844387076, 1.000000000000000000, 0.8660254037844387076, 1.000000000000000000, 0.8660254037844387076, 1.000000000000000000, 0.8660254037844387076, 1.000000000000000000, 0.8660254037844387076, 1.000000000000000000, 0.8660254037844387076, 1.000000000000000000, 0.8660254037844387076, 1.000000000000000000, 0.8660254037844387076, 1.000000000000000000, 0.8660254037844387076, 1.000000000000000000, 0.8660254037844387076, 1.000000000000000000, 0.8660254037844387076, 1.000000000000000000, 0.8660254037844387076, 1.000000000000000000, 0.8660254037844387076, 1.000000000000000000, 0.8660254037844387076, 1.000000000000000000, 0.8660254037844387076, 1.000000000000000000, 0.8660254037844387076, 1.000000000000000000, 0.8660254037844387076, 1.000000000000000000, 0.8660254037844387076, 1.000000000000000000, 0.8660254037844387076, 1.000000000000000000, 0.8660254037844387076, 1.000000000000000000, 0.8660254037844387076, 1.000000000000000000, 0.8660254037844387076, 1.000000000000000000, 0.8660254037844387076, 1.000000000000000000, 0.8660254037844387076, 1.000000000000000000, 0.8660254037844387076, 1.000000000000000000, 0.8660254037844387076, 1.000000000000000000, 0.8660254037844387076, 1.000000000000000000, 0.8660254037844387076, 1.000000000000000000, 0.8660254037844387076, 1.000000000000000000, 0.8660254037844387076, 1.000000000000000000, 0.8660254037844387076, 1.000000000000000000, 0.8660254037844387076, 1.000000000000000000, 0.8660254037844387076, 1.000000000000000000, 0.8660254037844387076, 1.000000000000000000, 0.8660254037844387076, 1.000000000000000000, 0.8660254037844387076, 1.000000000000000000, 0.8660254037844387076, 1.000000000000000000, 0.8660254037844387076, 1.000000000000000000, 0.8660254037844387076, 1.000000000000000000, 0.8660254037844387076, 1.000000000000000000, 0.8660254037844387076, 1.000000000000000000, 0.8660254037844387076, 1.000000000000000000, 0.8660254037844387076, 1.000000000000000000, 0.8660254037844387076, 1.000000000000000000, 0.8660254037844387076, 1.000000000000000000, 0.8660254037844387076, 1.000000000000000000, 0.8660254037844387076, 1.000000000000000000, 0.8660254037844387076, 1.000000000000000000, 0.8660254037844387076, 1.000000000000000000, 0.8660254037844387076, 1.000000000000000000, 0.8660254037844387076, 1.000000000000000000, 0.8660254037844387076, 1.000000000000000000, 0.8660254037844387076, 1.000000000000000000, 0.8660254037844387076, 1.000000000000000000, 0.8660254037844387076, 1.000000000000000000, 0.8660254037844387076, 1.000000000000000000, 0.8660254037844387076, 1.000000000000000000, 0.8660254037844387076, 1.000000000000000000, 0.8660254037844387076, 1.000000000000000000, 0.8660254037844387076, 1.000000000000000000, 0.8660254037844387076, 1.000000000000000000, 0.8660254037844387076, 1.000000000000000000, 0.8660254037844387076, 1.000000000000000000, 0.8660254037844387076, 1.000000000000000000, 0.8660254037844387076, 1.000000000000000000, 0.8660254037844387076, 1.000000000000000000, 0.8660254037844387076, 1.000000000000000000, 0.8660254037844387076, 1.000000000000000000, 0.8660254037844387076, 1.000000000000000000, 0.8660254037844387076, 1.000000000000000000, 0.8660254037844387076, 1.000000000000000000, 0.8660254037844387076, 1.000000000000000000, 0.8660254037844387076, 1.000000000000000000, 0.8660254037844387076, 1.000000000000000000, 0.8660254037844387076, 1.000000000000000000, 0.8660254037844387076, 1.000000000000000000, 0.8660254037844387076, 1.000000000000000000, 0.8660254037844387076, 1.000000000000000000, 0.8660254037844387076, 1.000000000000000000, 0.8660254037844387076, 1.000000000000000000, 0.8660254037844387076, 1.000000000000000000, 0.8660254037844387076, 1.000000000000000000, 0.8660254037844387076, 1.000000000000000000, 0.8660254037844387076, 1.000000000000000000, 0.8660254037844387076, 1.000000000000000000, 0.8660254037844387076, 1.000000000000000000, 0.8660254037844387076, 1.000000000000000000, 0.8660254037844387076, 1.000000000000000000, 0.8660254037844387076, 1.000000000000000000, 0.8660254037844387076, 1.000000000000000000, 0.8660254037844387076, 1.000000000000000000, 0.8660254037844387076, 1.000000000000000000, 0.8660254037844387076, 1.000000000000000000, 0.8660254037844387076, 1.000000000000000000, 0.8660254037844387076, 1.000000000000000000, 0.8660254037844387076, 1.000000000000000000, 0.8660254037844387076, 1.000000000000000000, 0.8660254037844387076, 1.000000000000000000, 0.8660254037844387076, 1.000000000000000000, 0.8660254037844387076, 1.000000000000000000, 0.8660254037844387076, 1.000000000000000000, 0.8660254037844387076, 1.000000000000000000, 0.8660254037844387076, 1.000000000000000000, 0.8660254037844387076, 1.000000000000000000, 0.8660254037844387076, 1.000000000000000000, 0.8660254037844387076, 1.000000000000000000, 0.8660254037844387076, 1.000000000000000000, 0.8660254037844387076, 1.000000000000000000, 0.8660254037844387076, 1.000000000000000000, 0.8660254037844387076, 1.000000000000000000, 0.8660254037844387076, 1.000000000000000000, 0.8660254037844387076, 1.000000000000000000, 0.8660254037844387076, 1.000000000000000000, 0.8660254037844387076, 1.000000000000000000, 0.8660254037844387076, 1.000000000000000000, 0.8660254037844387076, 1.000000000000000000, 0.8660254037844387076, 1.000000000000000000, 0.8660254037844387076, 1.000000000000000000, 0.8660254037844387076, 1.000000000000000000, 0.8660254037844387076, 1.000000000000000000, 0.8660254037844387076, 1.000000000000000000, 0.8660254037844387076, 1.000000000000000000, 0.8660254037844387076, 1.000000000000000000, 0.8660254037844387076, 1.000000000000000000, 0.8660254037844387076, 1.000000000000000000, 0.8660254037844387076, 1.000000000000000000, 0.8660254037844387076, 1.000000000000000000, 0.8660254037844387076, 1.000000000000000000, 0.8660254037844387076, 1.000000000000000000, 0.8660254037844387076, 1.000000000000000000, 0.8660254037844387076, 1.000000000000000000, 0.8660254037844387076, 1.000000000000000000, 0.8660254037844387076, 1.000000000000000000, 0.8660254037844387076, 1.000000000000000000, 0.8660254037844387076, 1.000000000000000000, 0.8660254037844387076, 1.000000000000000000, 0.8660254037844387076, 1.000000000000000000, 0.8660254037844387076, 1.000000000000000000, 0.8660254037844387076, 1.000000000000000000, 0.8660254037844387076, 1.000000000000000000, 0.8660254037844387076, 1.000000000000000000, 0.8660254037844387076, 1.000000000000000000, 0.8660254037844387076, 1.000000000000000000, 0.8660254037844387076, 1.000000000000000000, 0.8660254037844387076, 1.000000000000000000, 0.8660254037844387076, 1.000000000000000000, 0.8660254037844387076, 1.000000000000000000, 0.8660254037844387076, 1.000000000000000000, 0.8660254037844387076, 1.000000000000000000, 0.8660254037844387076, 1.000000000000000000, 0.8660254037844387076, 1.000000000000000000, 0.8660254037844387076, 1.000000000000000000, 0.8660254037844387076, 1.000000000000000000, 0.8660254037844387076, 1.000000000000000000, 0.8660254037844387076, 1.000000000000000000, 0.8660254037844387076, 1.000000000000000000, 0.8660254037844387076, 1.000000000000000000, 0.8660254037844387076, 1.000000000000000000, 0.8660254037844387076, 1.000000000000000000, 0.8660254037844387076, 1.000000000000000000, 0.8660254037844387076, 1.000000000000000000, 0.8660254037844387076, 1.000000000000000000, 0.8660254037844387076, 1.000000000000000000, 0.8660254037844387076, 1.000000000000000000, 0.8660254037844387076, 1.000000000000000000, 0.8660254037844387076, 1.000000000000000000, 0.8660254037844387076, 1.000000000000000000, 0.8660254037844387076, 1.000000000000000000, 0.8660254037844387076, 1.000000000000000000, 0.8660254037844387076, 1.000000000000000000, 0.8660254037844387076, 1.000000000000000000, 0.8660254037844387076, 1.000000000000000000, 0.8660254037844387076, 1.000000000000000000, 0.8660254037844387076, 1.000000000000000000, 0.8660254037844387076, 1.000000000000000000, 0.8660254037844387076, 1.000000000000000000, 0.8660254037844387076, 1.000000000000000000, 0.8660254037844387076, 1.000000000000000000, 0.8660254037844387076, 1.000000000000000000, 0.8660254037844387076, 1.000000000000000000, 0.8660254037844387076, 1.000000000000000000, 0.8660254037844387076, 1.000000000000000000, 0.8660254037844387076, 1.000000000000000000, 0.8660254037844387076, 1.000000000000000000, 0.8660254037844387076, 1.000000000000000000, 0.8660254037844387076, 1.000000000000000000, 0.8660254037844387076, 1.000000000000000000, 0.8660254037844387076, 1.000000000000000000, 0.8660254037844387076, 1.000000000000000000, 0.8660254037844387076, 1.000000000000000000, 0.8660254037844387076, 1.000000000000000000, 0.8660254037844387076, 1.000000000000000000, 0.8660254037844387076, 1.000000000000000000, 0.8660254037844387076, 1.000000000000000000, 0.8660254037844387076, 1.000000000000000000, 0.8660254037844387076, 1.000000000000000000, 0.8660254037844387076, 1.000000000000000000, 0.8660254037844387076, 1.000000000000000000, 0.8660254037844387076, 1.000000000000000000, 0.8660254037844387076, 1.000000000000000000, 0.8660254037844387076, 1.000000000000000000, 0.8660254037844387076, 1.000000000000000000, 0.8660254037844387076, 1.000000000000000000, 0.8660254037844387076, 1.000000000000000000, 0.8660254037844387076, 1.000000000000000000, 0.8660254037844387076, 1.000000000000000000, 0.8660254037844387076, 1.000000000000000000, 0.8660254037844387076, 1.000000000000000000, 0.8660254037844387076, 1.000000000000000000, 0.8660254037844387076, 1.000000000000000000, 0.8660254037844387076, 1.000000000000000000, 0.8660254037844387076, 1.000000000000000000, 0.8660254037844387076, 1.000000000000000000, 0.8660254037844387076, 1.000000000000000000, 0.8660254037844387076, 1.000000000000000000, 0.8660254037844387076, 1.000000000000000000, 0.8660254037844387076, 1.000000000000000000, 0.8660254037844387076, 1.000000000000000000, 0.8660254037844387076, 1.000000000000000000, 0.8660254037844387076, 1.000000000000000000, 0.8660254037844387076, 1.000000000000000000, 0.8660254037844387076, 1.000000000000000000, 0.8660254037844387076, 1.000000000000000000, 0.8660254037844387076, 1.000000000000000000, 0.8660254037844387076, 1.000000000000000000, 0.8660254037844387076, 1.000000000000000000, 0.8660254037844387076, 1.000000000000000000, 0.8660254037844387076, 1.000000000000000000, 0.8660254037844387076, 1.000000000000000000, 0.8660254037844387076, 1.000000000000000000, 0.8660254037844387076, 1.000000000000000000, 0.8660254037844387076, 1.000000000000000000, 0.8660254037844387076, 1.000000000000000000, 0.8660254037844387076, 1.000000000000000000, 0.8660254037844387076, 1.000000000000000000, 0.8660254037844387076, 1.000000000000000000, 0.8660254037844387076, 1.000000000000000000, 0.8660254037844387076, 1.000000000000000000, 0.8660254037844387076, 1.000000000000000000, 0.8660254037844387076, 1.000000000000000000, 0.8660254037844387076, 1.000000000000000000, 0.8660254037844387076, 1.000000000000000000, 0.8660254037844387076, 1.000000000000000000, 0.8660254037844387076, 1.000000000000000000, 0.8660254037844387076, 1.000000000000000000, 0.8660254037844387076, 1.000000000000000000, 0.8660254037844387076, 1.000000000000000000, 0.8660254037844387076, 1.000000000000000000, 0.8660254037844387076, 1.000000000000000000, 0.8660254037844387076, 1.000000000000000000, 0.8660254037844387076, 1.000000000000000000, 0.8660254037844387076, 1.000000000000000000, 0.8660254037844387076, 1.000000000000000000, 0.8660254037844387076, 1.000000000000000000, 0.8660254037844387076, 1.000000000000000000, 0.8660254037844387076, 1.000000000000000000, 0.8660254037844387076, 1.000000000000000000, 0.8660254037844387076, 1.000000000000000000, 0.8660254037844387076, 1.000000000000000000, 0.8660254037844387076, 1.000000000000000000, 0.8660254037844387076, 1.000000000000000000, 0.8660254037844387076, 1.000000000000000000, 0.8660254037844387076, 1.000000000000000000) ) ) 
 REPRESENTATION_ITEM ( '' )  SURFACE ( )  );
#43034 = CARTESIAN_POINT ( 'NONE',  ( 8.390625000614518214, -3.027376345333610441, -5.243569643749999898 ) ) ;
#43035 = CARTESIAN_POINT ( 'NONE',  ( 11.05312500061451608, -4.541064518000417216, -2.621784821875001281 ) ) ;
#43036 = CARTESIAN_POINT ( 'NONE',  ( 24.33750000122903145, -4.330127018922194537, 2.499999999999995559 ) ) ;
#43037 = AXIS2_PLACEMENT_3D ( 'NONE', #26412, #36400, #37120 ) ;
#43038 = CARTESIAN_POINT ( 'NONE',  ( 22.47187500061451715, 3.027376345333613106, -5.243569643749998122 ) ) ;
#43039 = CARTESIAN_POINT ( 'NONE',  ( 3.570441056944901881, 3.500278654462113614, -3.904237691275162625 ) ) ;
#43040 = CARTESIAN_POINT ( 'NONE',  ( 6.225000001229036073, 2.886751345948126879, 4.999999999999999112 ) ) ;
#43041 = CARTESIAN_POINT ( 'NONE',  ( 6.009375000614519458, 0.000000000000000000, 5.243569643749999010 ) ) ;
#43042 = CARTESIAN_POINT ( 'NONE',  ( 24.19687500061451857, -3.027376345333610441, -5.243569643749999898 ) ) ;
#43043 =( BOUNDED_CURVE ( )  B_SPLINE_CURVE ( 2, ( #44735, #67269, #39183, #61698, #11097, #56169, #24982, #71153, #70056 ),
 .UNSPECIFIED., .F., .F. ) 
 B_SPLINE_CURVE_WITH_KNOTS ( ( 3, 2, 2, 2, 3 ),
 ( 0.7083333333333333703, 0.7129629629629629095, 0.7222222222222222099, 0.7314814814814815103, 0.7361111111111111605 ),
 .UNSPECIFIED. ) 
 CURVE ( )  GEOMETRIC_REPRESENTATION_ITEM ( )  RATIONAL_B_SPLINE_CURVE ( ( 0.9330127018922192983, 0.9330127018922200755, 1.000000000000000000, 0.8660254037844387076, 1.000000000000000000, 0.8660254037844387076, 1.000000000000000000, 0.9330127018922185211, 0.9330127018922192983 ) ) 
 REPRESENTATION_ITEM ( '' )  );
#43044 = CARTESIAN_POINT ( 'NONE',  ( 4.531380608837685564, 2.113648287258761194, -4.671852478106539586 ) ) ;
#43045 = CARTESIAN_POINT ( 'NONE',  ( 17.72812500061451502, -4.541064518000419881, 2.621784821874995952 ) ) ;
#43046 = CARTESIAN_POINT ( 'NONE',  ( 24.23437500061451644, 6.421520780324663323E-16, -5.243569643749999010 ) ) ;
#43047 = CARTESIAN_POINT ( 'NONE',  ( -3.756430356250000990, 18.41562499938548214, 32.16877607737301048 ) ) ;
#43048 = DIRECTION ( 'NONE',  ( -1.000000000000000000, -0.000000000000000000, -0.000000000000000000 ) ) ;
#43049 = CARTESIAN_POINT ( 'NONE',  ( 34.99999999999999289, 6.363961030678916053, -6.363961030678939146 ) ) ;
#43050 = CARTESIAN_POINT ( 'NONE',  ( 4.996875000614516615, 6.054752690667223547, 3.707466751127219781E-16 ) ) ;
#43051 = CARTESIAN_POINT ( 'NONE',  ( 13.67812500061451786, -4.541064518000419881, 2.621784821874995952 ) ) ;
#43052 = VECTOR ( 'NONE', #25774, 1000.000000000000000 ) ;
#43053 = CARTESIAN_POINT ( 'NONE',  ( 13.05937500061451750, 4.541064518000418104, -2.621784821874998173 ) ) ;
#43054 = ORIENTED_EDGE ( 'NONE', *, *, #7959, .T. ) ;
#43055 = CARTESIAN_POINT ( 'NONE',  ( 22.35000000122903430, 5.773502691896255534, 3.535250795749688401E-16 ) ) ;
#43056 = CARTESIAN_POINT ( 'NONE',  ( 25.07812500061451644, 6.421520780324663323E-16, -5.243569643749999010 ) ) ;
#43057 = CARTESIAN_POINT ( 'NONE',  ( 3.461013385977631529, 3.608566055203085821, -3.626329471737537613 ) ) ;
#43058 = CARTESIAN_POINT ( 'NONE',  ( -3.999999999999999112, 20.33749999999999858, 27.69059892324149530 ) ) ;
#43059 = CARTESIAN_POINT ( 'NONE',  ( 15.67500000000000071, -4.330127018922194537, 2.499999999999995559 ) ) ;
#43060 = CARTESIAN_POINT ( 'NONE',  ( 25.23750000122903359, -4.330127018922194537, 2.499999999999995559 ) ) ;
#43061 = CARTESIAN_POINT ( 'NONE',  ( 19.49062500061451431, -3.027376345333614438, 5.243569643749998122 ) ) ;
#43062 = ORIENTED_EDGE ( 'NONE', *, *, #44217, .F. ) ;
#43063 = CARTESIAN_POINT ( 'NONE',  ( 21.71249999999999858, 2.886751345948129099, -4.999999999999998224 ) ) ;
#43064 = CARTESIAN_POINT ( 'NONE',  ( 23.18437500061451573, -4.541064518000419881, 2.621784821874995952 ) ) ;
#43065 = ORIENTED_EDGE ( 'NONE', *, *, #55566, .F. ) ;
#43066 = DIRECTION ( 'NONE',  ( 0.000000000000000000, 0.000000000000000000, 1.000000000000000000 ) ) ;
#43067 = CARTESIAN_POINT ( 'NONE',  ( 11.05312500061451608, -4.541064518000417216, -2.621784821875001281 ) ) ;
#43068 = CARTESIAN_POINT ( 'NONE',  ( 4.153125000614515727, 0.000000000000000000, 5.243569643749999010 ) ) ;
#43069 = CARTESIAN_POINT ( 'NONE',  ( 14.07187500061451679, -4.119189519843968306, 2.378215178124996054 ) ) ;
#43070 = CARTESIAN_POINT ( 'NONE',  ( 27.10312500061451502, 0.000000000000000000, 5.243569643749999010 ) ) ;
#43071 =( BOUNDED_CURVE ( )  B_SPLINE_CURVE ( 2, ( #14594, #65574, #25316, #53769, #59286, #19767, #47862 ),
 .UNSPECIFIED., .F., .F. ) 
 B_SPLINE_CURVE_WITH_KNOTS ( ( 3, 2, 2, 3 ),
 ( 0.2999999999999999889, 0.3033333333333333437, 0.3066666666666666430, 0.3099999999999999978 ),
 .UNSPECIFIED. ) 
 CURVE ( )  GEOMETRIC_REPRESENTATION_ITEM ( )  RATIONAL_B_SPLINE_CURVE ( ( 1.000000000000000000, 0.8660254037844387076, 1.000000000000000000, 0.8660254037844387076, 1.000000000000000000, 0.8660254037844387076, 1.000000000000000000 ) ) 
 REPRESENTATION_ITEM ( '' )  );
#43072 = CARTESIAN_POINT ( 'NONE',  ( 16.35000000000000142, 4.330127018922192761, -2.499999999999997780 ) ) ;
#43073 = CARTESIAN_POINT ( 'NONE',  ( 27.26249999999999929, 2.886751345948126879, 4.999999999999999112 ) ) ;
#43074 = CARTESIAN_POINT ( 'NONE',  ( 2.000000000000000444, 14.31874999877096499, 26.53589838486224650 ) ) ;
#43075 = CARTESIAN_POINT ( 'NONE',  ( 6.496875000614517504, -3.027376345333614438, 5.243569643749998122 ) ) ;
#43076 = CARTESIAN_POINT ( 'NONE',  ( 17.14687500061451786, 6.054752690667223547, 3.707466751127219781E-16 ) ) ;
#43077 = CARTESIAN_POINT ( 'NONE',  ( -5.810221930991193690E-16, 13.70000000122903394, 26.00000000000000355 ) ) ;
#43078 = ORIENTED_EDGE ( 'NONE', *, *, #51591, .T. ) ;
#43079 = CARTESIAN_POINT ( 'NONE',  ( 25.60312500061451502, 4.541064518000418104, -2.621784821874998173 ) ) ;
#43080 = CARTESIAN_POINT ( 'NONE',  ( 27.87187500061451573, 3.027376345333613106, -5.243569643749998122 ) ) ;
#43081 = CARTESIAN_POINT ( 'NONE',  ( 3.234375000614516438, 4.541064518000418104, 2.621784821874999949 ) ) ;
#43082 = CARTESIAN_POINT ( 'NONE',  ( 12.67499999999999893, 6.123233995736764310E-16, -4.999999999999998224 ) ) ;
#43083 = CARTESIAN_POINT ( 'NONE',  ( 10.86562500061451431, 3.027376345333611329, 5.243569643749999010 ) ) ;
#43084 = DIRECTION ( 'NONE',  ( 0.000000000000000000, 0.000000000000000000, 1.000000000000000000 ) ) ;
#43085 = CARTESIAN_POINT ( 'NONE',  ( 15.41250000122903252, -4.330127018922190985, -2.500000000000001332 ) ) ;
#43086 = CARTESIAN_POINT ( 'NONE',  ( 15.26250000122903216, 0.000000000000000000, 4.999999999999998224 ) ) ;
#43087 = CARTESIAN_POINT ( 'NONE',  ( 17.82187500061451502, -5.492252693125287522, -1.008910452111647106E-15 ) ) ;
#43088 = CARTESIAN_POINT ( 'NONE',  ( 4.528125000614516615, 4.541064518000418104, 2.621784821874999949 ) ) ;
#43089 = CARTESIAN_POINT ( 'NONE',  ( 22.50937500061451857, 4.541064518000418104, -2.621784821874998173 ) ) ;
#43090 = CARTESIAN_POINT ( 'NONE',  ( 4.243569643749999010, 16.97187500061451360, 27.54997392385601174 ) ) ;
#43091 = CARTESIAN_POINT ( 'NONE',  ( 23.82187500061451502, 3.027376345333613106, -5.243569643749998122 ) ) ;
#43092 = CARTESIAN_POINT ( 'NONE',  ( 5.400000000000002132, -4.330127018922190985, -2.500000000000001332 ) ) ;
#43093 = CARTESIAN_POINT ( 'NONE',  ( -1.999999999999997113, 11.18750000122903288, 33.46410161513775705 ) ) ;
#43094 = CARTESIAN_POINT ( 'NONE',  ( 12.92812500061451786, 6.421520780324663323E-16, -5.243569643749999010 ) ) ;
#43095 = CARTESIAN_POINT ( 'NONE',  ( 4.275000001229035895, 2.886751345948129099, -4.999999999999998224 ) ) ;
#43096 = EDGE_CURVE ( 'NONE', #32613, #39358, #62499, .T. ) ;
#43097 = CARTESIAN_POINT ( 'NONE',  ( 9.571875000614518569, 3.027376345333611329, 5.243569643749999010 ) ) ;
#43098 = CARTESIAN_POINT ( 'NONE',  ( 34.99999999999999289, -6.363961030678871644, 4.863961030678981778 ) ) ;
#43099 = AXIS2_PLACEMENT_3D ( 'NONE', #63351, #12736, #23463 ) ;
#43100 = CARTESIAN_POINT ( 'NONE',  ( 10.04062500061451502, -3.027376345333614438, 5.243569643749998122 ) ) ;
#43101 = CARTESIAN_POINT ( 'NONE',  ( 15.53437500061451715, -4.541064518000419881, 2.621784821874995952 ) ) ;
#43102 = CARTESIAN_POINT ( 'NONE',  ( 24.46875000122903643, 2.886751345948129099, -4.999999999999997335 ) ) ;
#43103 = CARTESIAN_POINT ( 'NONE',  ( 20.55000000122903359, 5.773502691896255534, 3.535250795749688894E-16 ) ) ;
#43104 = CARTESIAN_POINT ( 'NONE',  ( 10.24687500061451750, -3.027376345333610441, -5.243569643749999898 ) ) ;
#43105 = CARTESIAN_POINT ( 'NONE',  ( 13.41562500061451502, 3.027376345333613106, -5.243569643749998122 ) ) ;
#43106 = CARTESIAN_POINT ( 'NONE',  ( 28.06875000122903074, 2.886751345948129099, -4.999999999999998224 ) ) ;
#43107 = CARTESIAN_POINT ( 'NONE',  ( 21.79687500061451644, -3.027376345333614438, 5.243569643749998122 ) ) ;
#43108 = DIRECTION ( 'NONE',  ( 0.4999999999999975575, 0.000000000000000000, 0.8660254037844400399 ) ) ;
#43109 = CARTESIAN_POINT ( 'NONE',  ( -2.065650683794914233, 4.559369103593684969, 33.43471409431110430 ) ) ;
#43110 = CARTESIAN_POINT ( 'NONE',  ( 2.958716452545182118, -4.315365460520880880, -3.012707056649966741 ) ) ;
#43111 = CARTESIAN_POINT ( 'NONE',  ( -4.243569643749999898, 13.55937500061451750, -30.00000000000000000 ) ) ;
#43112 = CARTESIAN_POINT ( 'NONE',  ( 15.67500000122903181, 2.886751345948126879, 4.999999999999999112 ) ) ;
#43113 = AXIS2_PLACEMENT_3D ( 'NONE', #6165, #51601, #45699 ) ;
#43114 = CARTESIAN_POINT ( 'NONE',  ( 9.271875000614516082, -6.054752690667223547, -1.112240025338166033E-15 ) ) ;
#43115 = CARTESIAN_POINT ( 'NONE',  ( 2.121784821875001281, 18.60312500061451857, -26.32496088578401938 ) ) ;
#43116 = CARTESIAN_POINT ( 'NONE',  ( 16.91250000122903430, 4.330127018922192761, -2.499999999999997780 ) ) ;
#43117 = CARTESIAN_POINT ( 'NONE',  ( 9.590625000614517504, -3.027376345333614438, 5.243569643749998122 ) ) ;
#43118 = ORIENTED_EDGE ( 'NONE', *, *, #52890, .F. ) ;
#43119 = AXIS2_PLACEMENT_3D ( 'NONE', #5035, #61179, #21646 ) ;
#43120 = CARTESIAN_POINT ( 'NONE',  ( 16.16250000000000142, -5.773502691896255534, -1.060575238724906372E-15 ) ) ;
#43121 = CARTESIAN_POINT ( 'NONE',  ( 10.50000000122903110, -2.886751345948193048, -4.999999999999883649 ) ) ;
#43122 = CARTESIAN_POINT ( 'NONE',  ( 9.046875000614518214, 6.054752690667223547, 3.707466751127219781E-16 ) ) ;
#43123 = CARTESIAN_POINT ( 'NONE',  ( 3.999999999999998668, 16.90624999877096712, 32.30940107675850470 ) ) ;
#43124 = CARTESIAN_POINT ( 'NONE',  ( 9.750000001229032875, 5.773502691896255534, 3.535250795749688894E-16 ) ) ;
#43125 = CARTESIAN_POINT ( 'NONE',  ( 18.22500000122903430, 2.886751345948129099, -4.999999999999998224 ) ) ;
#43126 = CARTESIAN_POINT ( 'NONE',  ( 16.30312500061451786, 0.000000000000000000, 5.243569643749999010 ) ) ;
#43127 = CARTESIAN_POINT ( 'NONE',  ( 20.95312500061451999, -4.541064518000417216, -2.621784821875001281 ) ) ;
#43128 = CARTESIAN_POINT ( 'NONE',  ( 27.48750000122903359, -4.330127018922194537, 2.499999999999995559 ) ) ;
#43129 = CARTESIAN_POINT ( 'NONE',  ( 2.915625000614516793, -6.054752690667223547, -1.112240025338166033E-15 ) ) ;
#43130 = CARTESIAN_POINT ( 'NONE',  ( 24.33749999999999858, -2.886751345948125991, -5.000000000000000000 ) ) ;
#43131 = FACE_OUTER_BOUND ( 'NONE', #44641, .T. ) ;
#43132 = CARTESIAN_POINT ( 'NONE',  ( 26.55000000000000071, -4.330127018922190985, -2.500000000000001332 ) ) ;
#43133 = CARTESIAN_POINT ( 'NONE',  ( 28.99687500061451573, -3.027376345333614438, 5.243569643749998122 ) ) ;
#43134 = CARTESIAN_POINT ( 'NONE',  ( 4.000000000000000000, 17.48750000000000071, 32.30940107675849760 ) ) ;
#43135 = CARTESIAN_POINT ( 'NONE',  ( 12.07500000122903216, 2.886751345948126879, 4.999999999999999112 ) ) ;
#43136 = CARTESIAN_POINT ( 'NONE',  ( 3.862500000000001155, 2.886751345948126879, 4.999999999999999112 ) ) ;
#43137 = ADVANCED_FACE ( 'NONE', ( #72503 ), #27449, .T. ) ;
#43138 = CARTESIAN_POINT ( 'NONE',  ( 22.72499999999999787, 4.330127018922191873, 2.499999999999999556 ) ) ;
#43139 = CARTESIAN_POINT ( 'NONE',  ( 7.134375000614516793, 6.421520780324663323E-16, -5.243569643749999010 ) ) ;
#43140 = CARTESIAN_POINT ( 'NONE',  ( 27.10312500061451502, 0.000000000000000000, 5.243569643749999010 ) ) ;
#43142 = ADVANCED_FACE ( 'NONE', ( #11897 ), #6354, .T. ) ;
#43141 = CARTESIAN_POINT ( 'NONE',  ( -1.878215178125001827, 13.50312499938548427, 33.25316411605952283 ) ) ;
#43143 = CARTESIAN_POINT ( 'NONE',  ( 14.40000000000000036, -4.330127018922190985, -2.500000000000001332 ) ) ;
#43144 = AXIS2_PLACEMENT_3D ( 'NONE', #52007, #35369, #2133 ) ;
#43145 = CARTESIAN_POINT ( 'NONE',  ( 30.00000000000000000, 6.123233995736764310E-16, -4.999999999999998224 ) ) ;
#43146 = CARTESIAN_POINT ( 'NONE',  ( 5.371875000614516615, 3.027376345333613106, -5.243569643749998122 ) ) ;
#43147 = CARTESIAN_POINT ( 'NONE',  ( 7.921875000614517326, -6.054752690667223547, -1.112240025338166033E-15 ) ) ;
#43148 = CARTESIAN_POINT ( 'NONE',  ( 3.075000000000001510, -4.330127018922194537, 2.499999999999995559 ) ) ;
#43149 = CARTESIAN_POINT ( 'NONE',  ( -3.000416591977282496E-16, 12.94062500061459353, 25.09994784771203058 ) ) ;
#43150 = CARTESIAN_POINT ( 'NONE',  ( 22.46250000000000213, -5.773502691896255534, -1.060575238724906372E-15 ) ) ;
#43151 = APPLICATION_CONTEXT ( 'automotive_design' ) ;
#43153 = EDGE_CURVE ( 'NONE', #41603, #8225, #68485, .T. ) ;
#43152 = CARTESIAN_POINT ( 'NONE',  ( 28.98750000000000071, 5.773502691896255534, 3.535250795749688894E-16 ) ) ;
#43154 = CARTESIAN_POINT ( 'NONE',  ( 3.525000000000000355, -4.330127018922194537, 2.499999999999995559 ) ) ;
#43155 = AXIS2_PLACEMENT_3D ( 'NONE', #10086, #15976, #32616 ) ;
#43156 = CARTESIAN_POINT ( 'NONE',  ( 13.84687500061451715, 4.119189519843966529, -2.378215178124998275 ) ) ;
#43157 = ORIENTED_EDGE ( 'NONE', *, *, #51085, .T. ) ;
#43158 = CARTESIAN_POINT ( 'NONE',  ( 17.42812500061451786, 6.421520780324663323E-16, -5.243569643749999010 ) ) ;
#43159 = CARTESIAN_POINT ( 'NONE',  ( 11.35312500061451679, 0.000000000000000000, 5.243569643749999010 ) ) ;
#43160 = CARTESIAN_POINT ( 'NONE',  ( 24.12187500061451573, 5.824947211148865298E-16, -4.756430356249998326 ) ) ;
#43161 = CARTESIAN_POINT ( 'NONE',  ( 6.571875000614517681, -6.054752690667223547, -1.112240025338166033E-15 ) ) ;
#43162 = CARTESIAN_POINT ( 'NONE',  ( 22.94999999999999929, -4.330127018922190985, -2.500000000000001332 ) ) ;
#43163 = CARTESIAN_POINT ( 'NONE',  ( 20.32500000122903572, -5.773502691896255534, -1.060575238724906372E-15 ) ) ;
#43164 = CARTESIAN_POINT ( 'NONE',  ( 23.96249999999999858, 2.886751345948101122, -5.000000000000046185 ) ) ;
#43165 = AXIS2_PLACEMENT_3D ( 'NONE', #32252, #10089, #3084 ) ;
#43166 = CARTESIAN_POINT ( 'NONE',  ( 8.259375000614518569, 0.000000000000000000, 5.243569643749999010 ) ) ;
#43167 = CARTESIAN_POINT ( 'NONE',  ( 13.99687500061451928, 6.054752690667223547, 3.707466751127219781E-16 ) ) ;
#43168 = CARTESIAN_POINT ( 'NONE',  ( 23.70937500061451786, -4.541064518000417216, -2.621784821875001281 ) ) ;
#43169 = EDGE_CURVE ( 'NONE', #66704, #21346, #34422, .T. ) ;
#43170 = CARTESIAN_POINT ( 'NONE',  ( 34.99999999999999289, 6.363961030679004871, 6.363961030678849440 ) ) ;
#43171 = CARTESIAN_POINT ( 'NONE',  ( 13.53749999999999964, -2.886751345948125991, -5.000000000000000000 ) ) ;
#43172 = CARTESIAN_POINT ( 'NONE',  ( 17.70937500061451431, 0.000000000000000000, 5.243569643749999010 ) ) ;
#43173 = CARTESIAN_POINT ( 'NONE',  ( 10.28437500061451715, 6.421520780324663323E-16, -5.243569643749999010 ) ) ;
#43174 = CARTESIAN_POINT ( 'NONE',  ( 1.878215178125000495, 13.61562499938548321, 26.74683588394047007 ) ) ;
#43175 = CARTESIAN_POINT ( 'NONE',  ( 23.09999999999999787, 4.330127018922192761, -2.499999999999997780 ) ) ;
#43176 = CARTESIAN_POINT ( 'NONE',  ( -4.000000000000000000, 15.42500000000000071, 30.00000000000000000 ) ) ;
#43177 = CARTESIAN_POINT ( 'NONE',  ( -0.6945863667395647534, 9.663023495605401081, -33.93923213064925193 ) ) ;
#43178 = CARTESIAN_POINT ( 'NONE',  ( 24.30937500061451573, 4.119189519843966529, -2.378215178124998275 ) ) ;
#43179 = CARTESIAN_POINT ( 'NONE',  ( 12.89062500061451821, -3.027376345333610441, -5.243569643749999898 ) ) ;
#43180 = CARTESIAN_POINT ( 'NONE',  ( 29.70937500061451431, 4.541064518000418104, -2.621784821874998173 ) ) ;
#43181 = DIRECTION ( 'NONE',  ( -1.000000000000000000, -0.000000000000000000, -0.000000000000000000 ) ) ;
#43182 = DIRECTION ( 'NONE',  ( 0.000000000000000000, 0.000000000000000000, 1.000000000000000000 ) ) ;
#43183 = CARTESIAN_POINT ( 'NONE',  ( 13.27500000000000213, 4.330127018922191873, 2.499999999999999556 ) ) ;
#43184 = CARTESIAN_POINT ( 'NONE',  ( -2.000000000000000000, 19.13750000122903216, 26.53589838486224650 ) ) ;
#43185 = CARTESIAN_POINT ( 'NONE',  ( 12.07500000122903216, 2.886751345948126879, 4.999999999999999112 ) ) ;
#43186 = CARTESIAN_POINT ( 'NONE',  ( 21.53437500061451715, 6.421520780324663323E-16, -5.243569643749999010 ) ) ;
#43187 = CARTESIAN_POINT ( 'NONE',  ( 17.14687500061451786, 6.054752690667223547, 3.707466751127219781E-16 ) ) ;
#43188 = CARTESIAN_POINT ( 'NONE',  ( -1.999999999999997113, 16.47500000000000142, -26.53589838486224295 ) ) ;
#43189 = EDGE_LOOP ( 'NONE', ( #4205, #49067, #66619, #44739 ) ) ;
#43190 = CARTESIAN_POINT ( 'NONE',  ( 17.61562500061451786, 3.027376345333611329, 5.243569643749999010 ) ) ;
#43191 = CARTESIAN_POINT ( 'NONE',  ( 28.01250000122903216, -4.330127018922190985, -2.500000000000001332 ) ) ;
#43192 = CARTESIAN_POINT ( 'NONE',  ( 17.74687500061451928, -3.027376345333614438, 5.243569643749998122 ) ) ;
#43193 = CARTESIAN_POINT ( 'NONE',  ( 5.540625000614515905, -3.027376345333614438, 5.243569643749998122 ) ) ;
#43194 = CARTESIAN_POINT ( 'NONE',  ( 19.37812500061451715, 4.541064518000418104, 2.621784821874999949 ) ) ;
#43195 = CARTESIAN_POINT ( 'NONE',  ( 28.55625000122903145, 4.330127018922192761, -2.499999999999997780 ) ) ;
#43196 = CARTESIAN_POINT ( 'NONE',  ( 27.87187500061451573, 3.027376345333613106, -5.243569643749998122 ) ) ;
#43197 = CARTESIAN_POINT ( 'NONE',  ( 4.243569643749999010, 12.41562500061451857, 27.54997392385601174 ) ) ;
#43198 = CARTESIAN_POINT ( 'NONE',  ( 17.10000000122903430, -2.886751345948129988, 4.999999999999997335 ) ) ;
#43199 = CARTESIAN_POINT ( 'NONE',  ( 9.384375000614518569, 5.824947211148865298E-16, -4.756430356249998326 ) ) ;
#43200 = CARTESIAN_POINT ( 'NONE',  ( 27.85312500061451502, 4.541064518000418104, -2.621784821874998173 ) ) ;
#43201 = CARTESIAN_POINT ( 'NONE',  ( -3.999999999999997335, 9.800000001229033586, 32.30940107675850470 ) ) ;
#43202 = CARTESIAN_POINT ( 'NONE',  ( 21.04687500061451644, -3.027376345333610441, -5.243569643749999898 ) ) ;
#43203 = CARTESIAN_POINT ( 'NONE',  ( 22.98750000122903003, -4.330127018922194537, 2.499999999999995559 ) ) ;
#43204 = CARTESIAN_POINT ( 'NONE',  ( 23.95312500061451289, 0.000000000000000000, 5.243569643749999010 ) ) ;
#43205 = CARTESIAN_POINT ( 'NONE',  ( 16.24687500061451573, 6.054752690667223547, 3.707466751127219781E-16 ) ) ;
#43206 = CARTESIAN_POINT ( 'NONE',  ( 11.57812500061451644, 6.421520780324663323E-16, -5.243569643749999010 ) ) ;
#43207 = CARTESIAN_POINT ( 'NONE',  ( -2.121784821874999949, 13.93437500061451750, 26.32496088578401938 ) ) ;
#43208 = AXIS2_PLACEMENT_3D ( 'NONE', #33750, #40034, #34107 ) ;
#43209 = CARTESIAN_POINT ( 'NONE',  ( 20.76562500061451644, 3.027376345333611329, 5.243569643749999010 ) ) ;
#43210 = CARTESIAN_POINT ( 'NONE',  ( 9.975000000000001421, 6.123233995736764310E-16, -4.999999999999998224 ) ) ;
#43211 = EDGE_LOOP ( 'NONE', ( #37371, #57641, #50808, #11853 ) ) ;
#43212 = ORIENTED_EDGE ( 'NONE', *, *, #27586, .T. ) ;
#43213 = CARTESIAN_POINT ( 'NONE',  ( 24.03750000000000142, 5.773502691896255534, 3.535250795749688894E-16 ) ) ;
#43214 = CARTESIAN_POINT ( 'NONE',  ( -3.000416591977282496E-16, 18.39687500061451786, -34.90005215228797653 ) ) ;
#43215 = CARTESIAN_POINT ( 'NONE',  ( 3.250662400336420177, 3.799104362746421604, 3.614115195980558859 ) ) ;
#43216 = CARTESIAN_POINT ( 'NONE',  ( 24.44062500061451715, -3.027376345333614438, 5.243569643749998122 ) ) ;
#43217 = CARTESIAN_POINT ( 'NONE',  ( 4.303125000614516971, -4.541064518000417216, -2.621784821875001281 ) ) ;
#43218 = CARTESIAN_POINT ( 'NONE',  ( 20.62500000122903288, 2.886751345948126879, 4.999999999999999112 ) ) ;
#43219 = CARTESIAN_POINT ( 'NONE',  ( 25.45312500061451644, -4.541064518000417216, -2.621784821875001281 ) ) ;
#43220 = CARTESIAN_POINT ( 'NONE',  ( 21.89999999999999858, 0.000000000000000000, 4.999999999999998224 ) ) ;
#43221 =( BOUNDED_CURVE ( )  B_SPLINE_CURVE ( 2, ( #48038, #19939, #42493, #62024, #10330, #32864, #50228, #27327, #55399 ),
 .UNSPECIFIED., .F., .F. ) 
 B_SPLINE_CURVE_WITH_KNOTS ( ( 3, 2, 2, 2, 3 ),
 ( 0.6630434782608696231, 0.6666666666666666297, 0.6739130434782608647, 0.6811594202898550998, 0.6847826086956522174 ),
 .UNSPECIFIED. ) 
 CURVE ( )  GEOMETRIC_REPRESENTATION_ITEM ( )  RATIONAL_B_SPLINE_CURVE ( ( 0.9330127018922192983, 0.9330127018922202975, 1.000000000000000000, 0.8660254037844387076, 1.000000000000000000, 0.8660254037844387076, 1.000000000000000000, 0.9330127018922182991, 0.9330127018922192983 ) ) 
 REPRESENTATION_ITEM ( '' )  );
#43222 = CARTESIAN_POINT ( 'NONE',  ( 27.29062500061451502, -3.027376345333610441, -5.243569643749999898 ) ) ;
#43223 = CARTESIAN_POINT ( 'NONE',  ( 8.878125000614515372, 6.421520780324663323E-16, -5.243569643749999010 ) ) ;
#43224 = ORIENTED_EDGE ( 'NONE', *, *, #27906, .T. ) ;
#43225 = CARTESIAN_POINT ( 'NONE',  ( 24.47812500061451502, -4.541064518000419881, 2.621784821874995952 ) ) ;
#43226 = CARTESIAN_POINT ( 'NONE',  ( 5.053125000614517859, 0.000000000000000000, 5.243569643749999010 ) ) ;
#43227 = CARTESIAN_POINT ( 'NONE',  ( 14.40937500061451715, 4.119189519843966529, -2.378215178124998275 ) ) ;
#43228 = CARTESIAN_POINT ( 'NONE',  ( 3.815625000614518036, -6.054752690667223547, -1.112240025338166033E-15 ) ) ;
#43229 = CARTESIAN_POINT ( 'NONE',  ( 1.999999999999998668, 12.76250000122903394, -33.46410161513775705 ) ) ;
#43230 = CARTESIAN_POINT ( 'NONE',  ( 30.00000000000000000, 6.123233995736764310E-16, -4.999999999999998224 ) ) ;
#43231 = CARTESIAN_POINT ( 'NONE',  ( 11.10000000000000142, 0.000000000000000000, 4.999999999999998224 ) ) ;
#43232 = CARTESIAN_POINT ( 'NONE',  ( 10.84687500061451892, 6.054752690667223547, 3.707466751127219781E-16 ) ) ;
#43233 = CARTESIAN_POINT ( 'NONE',  ( 5.812500001229035540, 0.000000000000000000, 4.999999999999998224 ) ) ;
#43234 = CARTESIAN_POINT ( 'NONE',  ( 13.50937500061451679, 4.541064518000418104, -2.621784821874998173 ) ) ;
#43235 = CARTESIAN_POINT ( 'NONE',  ( 14.51250000000000107, 2.886751345948129099, -4.999999999999998224 ) ) ;
#43236 = CARTESIAN_POINT ( 'NONE',  ( 5.559375000614517504, 0.000000000000000000, 5.243569643749999010 ) ) ;
#43237 = CARTESIAN_POINT ( 'NONE',  ( 2.226602359779148887, 9.751272476441998904, -34.70164361699148259 ) ) ;
#43238 = VECTOR ( 'NONE', #18792, 1000.000000000000000 ) ;
#43240 = ADVANCED_FACE ( 'NONE', ( #22612 ), #461, .T. ) ;
#43239 = CARTESIAN_POINT ( 'NONE',  ( 11.52187500061451608, -6.054752690667223547, -1.112240025338166033E-15 ) ) ;
#43241 = CARTESIAN_POINT ( 'NONE',  ( 5.000000000000000000, 6.123233995736766282E-16, 50.00000000000000000 ) ) ;
#43242 = CARTESIAN_POINT ( 'NONE',  ( 22.00312500061451360, 4.541064518000418104, -2.621784821874998173 ) ) ;
#43243 = CARTESIAN_POINT ( 'NONE',  ( 4.243569643749999898, 19.57812500061459460, 30.00000000000000000 ) ) ;
#43244 = CARTESIAN_POINT ( 'NONE',  ( 24.57187500061451502, -6.054752690667223547, -1.112240025338166033E-15 ) ) ;
#43245 = EDGE_CURVE ( 'NONE', #61968, #28919, #62145, .T. ) ;
#43246 = CARTESIAN_POINT ( 'NONE',  ( -1.071796769724488563, 13.90490381179670010, -26.00000000000000000 ) ) ;
#43247 = CARTESIAN_POINT ( 'NONE',  ( 4.603125000614518569, 0.000000000000000000, 5.243569643749999010 ) ) ;
#43248 = CARTESIAN_POINT ( 'NONE',  ( 19.02187500061451431, -4.119189519843968306, 2.378215178124996054 ) ) ;
#43249 = CARTESIAN_POINT ( 'NONE',  ( 18.02812500061451573, 4.541064518000418104, 2.621784821874999949 ) ) ;
#43250 = CARTESIAN_POINT ( 'NONE',  ( 14.67187500061451821, -6.054752690667223547, -1.112240025338166033E-15 ) ) ;
#43251 = VECTOR ( 'NONE', #44700, 1000.000000000000000 ) ;
#43252 = CARTESIAN_POINT ( 'NONE',  ( 26.17500000122903359, -5.773502691896255534, -1.060575238724906372E-15 ) ) ;
#43253 = CARTESIAN_POINT ( 'NONE',  ( 6.121875000614517504, -6.054752690667223547, -1.112240025338166033E-15 ) ) ;
#43254 = CARTESIAN_POINT ( 'NONE',  ( 15.57187500061451679, -6.054752690667223547, -1.112240025338166033E-15 ) ) ;
#43255 = CARTESIAN_POINT ( 'NONE',  ( 24.07499999999999929, 4.330127018922191873, 2.499999999999999556 ) ) ;
#43256 = CARTESIAN_POINT ( 'NONE',  ( 4.050000001229035362, -2.886751345948129988, 4.999999999999997335 ) ) ;
#43257 = CARTESIAN_POINT ( 'NONE',  ( 24.12187500061451217, -6.054752690667223547, -1.112240025338166033E-15 ) ) ;
#43258 = CARTESIAN_POINT ( 'NONE',  ( 17.29687500061451999, -3.027376345333614438, 5.243569643749998122 ) ) ;
#43259 = CARTESIAN_POINT ( 'NONE',  ( -7.967954043666661671E-16, 13.09062499938548285, 34.33755215474603517 ) ) ;
#43260 = CARTESIAN_POINT ( 'NONE',  ( 29.69999999999999574, -4.330127018922190985, -2.500000000000001332 ) ) ;
#43261 = CARTESIAN_POINT ( 'NONE',  ( 8.175000000000002487, 6.123233995736764310E-16, -4.999999999999998224 ) ) ;
#43262 = CARTESIAN_POINT ( 'NONE',  ( 10.50937500061451502, -5.492252693125287522, -1.008910452111647106E-15 ) ) ;
#43263 = CARTESIAN_POINT ( 'NONE',  ( 19.82812500061451644, 4.541064518000418104, 2.621784821874999949 ) ) ;
#43264 = CARTESIAN_POINT ( 'NONE',  ( 10.23750000000000071, -2.886751345948129988, 4.999999999999997335 ) ) ;
#43265 = CARTESIAN_POINT ( 'NONE',  ( 3.478125000614517237, 6.421520780324663323E-16, -5.243569643749999010 ) ) ;
#43266 =( BOUNDED_CURVE ( )  B_SPLINE_CURVE ( 2, ( #18606, #51886, #18236 ),
 .UNSPECIFIED., .F., .F. ) 
 B_SPLINE_CURVE_WITH_KNOTS ( ( 3, 3 ),
 ( 0.9861111111111111605, 0.9876227234888749207 ),
 .UNSPECIFIED. ) 
 CURVE ( )  GEOMETRIC_REPRESENTATION_ITEM ( )  RATIONAL_B_SPLINE_CURVE ( ( 0.9330127018922194093, 0.9330127018922196314, 0.9401540605060327849 ) ) 
 REPRESENTATION_ITEM ( '' )  );
#43267 = CARTESIAN_POINT ( 'NONE',  ( 19.65000000000000213, 0.000000000000000000, 4.999999999999998224 ) ) ;
#43268 = CARTESIAN_POINT ( 'NONE',  ( 17.50312500061451715, 4.541064518000418104, -2.621784821874998173 ) ) ;
#43269 = CARTESIAN_POINT ( 'NONE',  ( 45.00000000000000000, 6.123233995736764310E-16, -4.999999999999998224 ) ) ;
#43270 = CARTESIAN_POINT ( 'NONE',  ( 22.57500000122903572, -5.773502691896255534, -1.060575238724906372E-15 ) ) ;
#43271 = CARTESIAN_POINT ( 'NONE',  ( 3.035296952380284186, 9.529902216964481809, 35.17929436357654538 ) ) ;
#43272 = CARTESIAN_POINT ( 'NONE',  ( 29.07187500061451502, -6.054752690667223547, -1.112240025338166033E-15 ) ) ;
#43273 = VERTEX_POINT ( 'NONE', #11540 ) ;
#43274 = CARTESIAN_POINT ( 'NONE',  ( 16.67812500061451786, 4.541064518000418104, 2.621784821874999949 ) ) ;
#43275 = CARTESIAN_POINT ( 'NONE',  ( 24.77812500061451217, 4.541064518000418104, 2.621784821874999949 ) ) ;
#43276 = CARTESIAN_POINT ( 'NONE',  ( 25.62187500061451573, 3.027376345333613106, -5.243569643749998122 ) ) ;
#43277 = CARTESIAN_POINT ( 'NONE',  ( 9.187500000000001776, 5.773502691896255534, 3.535250795749688894E-16 ) ) ;
#43278 = CARTESIAN_POINT ( 'NONE',  ( 12.96562500061451750, 3.027376345333613106, -5.243569643749998122 ) ) ;
#43279 = CARTESIAN_POINT ( 'NONE',  ( 26.99062500061451431, 6.054752690667223547, 3.707466751127219781E-16 ) ) ;
#43280 = CARTESIAN_POINT ( 'NONE',  ( 16.73437500061451644, 4.541064518000418104, 2.621784821874999949 ) ) ;
#43281 = CARTESIAN_POINT ( 'NONE',  ( 9.290625000614515017, -3.027376345333610441, -5.243569643749999898 ) ) ;
#43282 = CARTESIAN_POINT ( 'NONE',  ( 14.23125000122903394, 4.330127018922191873, 2.499999999999999556 ) ) ;
#43283 = CARTESIAN_POINT ( 'NONE',  ( -2.121784821874996840, 19.42812500061451786, 33.67503911421598417 ) ) ;
#43284 = EDGE_CURVE ( 'NONE', #15624, #35381, #68932, .T. ) ;
#43285 = CARTESIAN_POINT ( 'NONE',  ( 24.07500000122903216, 2.886751345948129099, -4.999999999999998224 ) ) ;
#43286 = CARTESIAN_POINT ( 'NONE',  ( 18.27187500061451431, -5.492252693125287522, -1.008910452111647106E-15 ) ) ;
#43287 = CARTESIAN_POINT ( 'NONE',  ( 14.35312500061451679, 4.541064518000418104, -2.621784821874998173 ) ) ;
#43288 = CARTESIAN_POINT ( 'NONE',  ( 8.484375000614518214, 6.421520780324663323E-16, -5.243569643749999010 ) ) ;
#43289 = CARTESIAN_POINT ( 'NONE',  ( 6.946875000614517681, -3.027376345333614438, 5.243569643749998122 ) ) ;
#43290 = ORIENTED_EDGE ( 'NONE', *, *, #30129, .T. ) ;
#43291 = CARTESIAN_POINT ( 'NONE',  ( -3.040073828171251158, 9.532700238123332781, 35.18707943735392973 ) ) ;
#43292 = CARTESIAN_POINT ( 'NONE',  ( 20.27812500061451573, 4.541064518000418104, 2.621784821874999949 ) ) ;
#43293 = CARTESIAN_POINT ( 'NONE',  ( 15.53437500061451715, -4.541064518000419881, 2.621784821874995952 ) ) ;
#43294 = CARTESIAN_POINT ( 'NONE',  ( 19.04062500061451146, -3.027376345333614438, 5.243569643749998122 ) ) ;
#43295 = CARTESIAN_POINT ( 'NONE',  ( -3.999999999999997335, 12.83750000000000213, 32.30940107675850470 ) ) ;
#43296 = CARTESIAN_POINT ( 'NONE',  ( 26.80312500061451431, -4.541064518000417216, -2.621784821875001281 ) ) ;
#43297 = CARTESIAN_POINT ( 'NONE',  ( 6.562500001229032875, 4.330127018922192761, -2.499999999999997780 ) ) ;
#43298 = ORIENTED_EDGE ( 'NONE', *, *, #57235, .T. ) ;
#43299 = CARTESIAN_POINT ( 'NONE',  ( 29.88749999999999929, 5.773502691896255534, 3.535250795749688894E-16 ) ) ;
#43300 = CARTESIAN_POINT ( 'NONE',  ( -3.999999999999999556, 18.16250000000000497, -32.30940107675850470 ) ) ;
#43301 = AXIS2_PLACEMENT_3D ( 'NONE', #8042, #7316, #41660 ) ;
#43302 = CARTESIAN_POINT ( 'NONE',  ( 22.61250000122903003, -4.330127018922190985, -2.500000000000001332 ) ) ;
#43303 = CARTESIAN_POINT ( 'NONE',  ( 3.756430356250000546, 15.04062499938548392, 27.83122392262697886 ) ) ;
#43304 = CARTESIAN_POINT ( 'NONE',  ( 7.359375000614516438, 0.000000000000000000, 5.243569643749999010 ) ) ;
#43305 = CARTESIAN_POINT ( 'NONE',  ( 12.47812500061451502, 6.421520780324663323E-16, -5.243569643749999010 ) ) ;
#43306 = VECTOR ( 'NONE', #51975, 1000.000000000000000 ) ;
#43307 = CARTESIAN_POINT ( 'NONE',  ( 7.509375000614517681, -4.541064518000417216, -2.621784821875001281 ) ) ;
#43308 = CARTESIAN_POINT ( 'NONE',  ( 26.32500000122903216, 2.886751345948129099, -4.999999999999998224 ) ) ;
#43309 = CARTESIAN_POINT ( 'NONE',  ( 16.43437500061451573, -4.541064518000419881, 2.621784821874995952 ) ) ;
#43310 = CARTESIAN_POINT ( 'NONE',  ( 4.171875000614517326, 3.027376345333611329, 5.243569643749999010 ) ) ;
#43311 = CARTESIAN_POINT ( 'NONE',  ( 29.58749999999999858, -2.886751345948129988, 4.999999999999997335 ) ) ;
#43312 = CARTESIAN_POINT ( 'NONE',  ( 5.315625000614516260, 3.027376345333613106, -5.243569643749998122 ) ) ;
#43313 = CARTESIAN_POINT ( 'NONE',  ( 16.11562500061451786, 3.027376345333613106, -5.243569643749998122 ) ) ;
#43314 = ORIENTED_EDGE ( 'NONE', *, *, #37707, .T. ) ;
#43315 = CARTESIAN_POINT ( 'NONE',  ( 11.50312500061451892, -4.541064518000417216, -2.621784821875001281 ) ) ;
#43316 = CARTESIAN_POINT ( 'NONE',  ( 5.512500001229033941, -4.330127018922190985, -2.500000000000001332 ) ) ;
#43317 = CARTESIAN_POINT ( 'NONE',  ( 8.878125000614515372, 6.421520780324663323E-16, -5.243569643749999010 ) ) ;
#43318 = CARTESIAN_POINT ( 'NONE',  ( 22.05937500061451573, 4.119189519843966529, -2.378215178124998275 ) ) ;
#43319 = CARTESIAN_POINT ( 'NONE',  ( 7.800000000000001599, 4.330127018922192761, -2.499999999999997780 ) ) ;
#43320 = CARTESIAN_POINT ( 'NONE',  ( 4.650000001229035895, -2.886751345948125991, -5.000000000000000000 ) ) ;
#43321 = CARTESIAN_POINT ( 'NONE',  ( 16.83749999999999858, 5.773502691896255534, 3.535250795749688894E-16 ) ) ;
#43322 = CARTESIAN_POINT ( 'NONE',  ( 18.98437500061451644, 4.541064518000418104, 2.621784821874999949 ) ) ;
#43323 = CARTESIAN_POINT ( 'NONE',  ( 14.28750000122903430, 4.330127018922191873, 2.499999999999999556 ) ) ;
#43324 = CARTESIAN_POINT ( 'NONE',  ( 22.61250000000000071, 2.886751345948129099, -4.999999999999998224 ) ) ;
#43325 = CARTESIAN_POINT ( 'NONE',  ( -3.000416591977282496E-16, 16.09062500061451573, -34.90005215228797653 ) ) ;
#43326 = CARTESIAN_POINT ( 'NONE',  ( -1.071796769724483234, 15.97009619066136565, 25.99999999999999645 ) ) ;
#43327 = CARTESIAN_POINT ( 'NONE',  ( -1.999999999999999112, 13.49374999877096570, 26.53589838486224650 ) ) ;
#43328 = DIRECTION ( 'NONE',  ( 0.000000000000000000, 1.000000000000000000, -8.673617379884036705E-17 ) ) ;
#43329 = CARTESIAN_POINT ( 'NONE',  ( 29.54062500061451502, -3.027376345333610441, -5.243569643749999898 ) ) ;
#43330 = CARTESIAN_POINT ( 'NONE',  ( 11.83125000122903181, 6.123233995736764310E-16, -4.999999999999998224 ) ) ;
#43331 = CARTESIAN_POINT ( 'NONE',  ( 15.75937500061451857, 4.541064518000418104, -2.621784821874998173 ) ) ;
#43332 = EDGE_CURVE ( 'NONE', #16892, #10170, #44449, .T. ) ;
#43333 = CARTESIAN_POINT ( 'NONE',  ( 27.86249999999999716, -5.773502691896255534, -1.060575238724906372E-15 ) ) ;
#43334 = CARTESIAN_POINT ( 'NONE',  ( 11.42812500061451608, -4.541064518000419881, 2.621784821874995952 ) ) ;
#43335 = CARTESIAN_POINT ( 'NONE',  ( 7.293750001229033053, -2.886751345948125991, -5.000000000000000000 ) ) ;
#43336 = CARTESIAN_POINT ( 'NONE',  ( 22.13437500061451502, 4.541064518000418104, 2.621784821874999949 ) ) ;
#43337 = CARTESIAN_POINT ( 'NONE',  ( 14.74687500061451573, 4.119189519843966529, -2.378215178124998275 ) ) ;
#43338 = CARTESIAN_POINT ( 'NONE',  ( 7.115625000614516082, 3.027376345333613106, -5.243569643749998122 ) ) ;
#43339 = CARTESIAN_POINT ( 'NONE',  ( 12.00937500061451857, -4.541064518000417216, -2.621784821875001281 ) ) ;
#43340 = ORIENTED_EDGE ( 'NONE', *, *, #63166, .F. ) ;
#43341 = CARTESIAN_POINT ( 'NONE',  ( 23.63437500061451502, -4.541064518000419881, 2.621784821874995952 ) ) ;
#43342 = CARTESIAN_POINT ( 'NONE',  ( 4.000175247584507154, 2.999766337098573654, -29.86665409634473178 ) ) ;
#43343 = CARTESIAN_POINT ( 'NONE',  ( 26.99062500061451431, 6.054752690667223547, 3.707466751127219781E-16 ) ) ;
#43344 = CARTESIAN_POINT ( 'NONE',  ( 50.00000000000000000, -1.494782592887706318, -8.874999999999994671 ) ) ;
#43345 = CARTESIAN_POINT ( 'NONE',  ( 7.875000000000000000, 4.330127018922191873, 2.499999999999999556 ) ) ;
#43346 = VECTOR ( 'NONE', #24943, 1000.000000000000000 ) ;
#43347 = CARTESIAN_POINT ( 'NONE',  ( 17.13750000122903216, -4.330127018922194537, 2.499999999999995559 ) ) ;
#43348 = DIRECTION ( 'NONE',  ( -1.000000000000000000, -0.000000000000000000, -0.000000000000000000 ) ) ;
#43349 = CARTESIAN_POINT ( 'NONE',  ( 8.334375000614516082, -2.746126346562642428, -4.756430356249999214 ) ) ;
#43350 = VERTEX_POINT ( 'NONE', #56249 ) ;
#43351 = CARTESIAN_POINT ( 'NONE',  ( 14.40000000000000036, -4.330127018922190985, -2.500000000000001332 ) ) ;
#43352 = CARTESIAN_POINT ( 'NONE',  ( 17.88749999999999929, -2.886751345948129988, 4.999999999999997335 ) ) ;
#43353 = CARTESIAN_POINT ( 'NONE',  ( 11.54062500061451857, -3.027376345333610441, -5.243569643749999898 ) ) ;
#43354 = ORIENTED_EDGE ( 'NONE', *, *, #15041, .F. ) ;
#43355 = CARTESIAN_POINT ( 'NONE',  ( 2.121784821875001281, 16.85937500061451999, -26.32496088578401938 ) ) ;
#43356 = CARTESIAN_POINT ( 'NONE',  ( 2.953125000614516438, -4.541064518000417216, -2.621784821875001281 ) ) ;
#43357 = CARTESIAN_POINT ( 'NONE',  ( 5.810221930991193690E-16, 13.96249999999999858, 26.00000000000000000 ) ) ;
#43358 = CARTESIAN_POINT ( 'NONE',  ( 10.83750000000000036, -2.886751345948125991, -5.000000000000000000 ) ) ;
#43359 = CARTESIAN_POINT ( 'NONE',  ( 3.950402052914877782, 3.833526817994171942, 3.360136779056243750 ) ) ;
#43360 = EDGE_LOOP ( 'NONE', ( #1181, #17384, #47283, #26914, #5728 ) ) ;
#43361 = CARTESIAN_POINT ( 'NONE',  ( 4.243569643749999898, 13.27812500061451750, 30.00000000000000000 ) ) ;
#43362 = CARTESIAN_POINT ( 'NONE',  ( 27.55312500061451786, 0.000000000000000000, 5.243569643749999010 ) ) ;
#43363 = CARTESIAN_POINT ( 'NONE',  ( -5.810221930991193690E-16, 13.58750000000000036, -34.00000000000000000 ) ) ;
#43364 = CARTESIAN_POINT ( 'NONE',  ( -3.756430356249999214, 20.47812499938548214, 27.83122392262697531 ) ) ;
#43365 = CARTESIAN_POINT ( 'NONE',  ( 21.60937500061451644, 4.541064518000418104, -2.621784821874998173 ) ) ;
#43366 = CARTESIAN_POINT ( 'NONE',  ( 19.75312500061451360, 4.541064518000418104, -2.621784821874998173 ) ) ;
#43367 = CARTESIAN_POINT ( 'NONE',  ( 2.121784821874999061, 13.80312500061459424, -33.67503911421598417 ) ) ;
#43368 = CARTESIAN_POINT ( 'NONE',  ( 22.27500000122903145, 2.886751345948129099, -4.999999999999998224 ) ) ;
#43369 = CARTESIAN_POINT ( 'NONE',  ( 3.553125000614516082, 4.541064518000418104, -2.621784821874998173 ) ) ;
#43370 = CARTESIAN_POINT ( 'NONE',  ( 23.44687500061451502, 5.492252693125287522, 3.363034840372157021E-16 ) ) ;
#43371 = CARTESIAN_POINT ( 'NONE',  ( 21.06562500061451715, 3.027376345333612662, -5.243569643749998122 ) ) ;
#43372 = CARTESIAN_POINT ( 'NONE',  ( 7.509375000614517681, -4.119189519843965641, -2.378215178125001383 ) ) ;
#43373 = CARTESIAN_POINT ( 'NONE',  ( -1.878215178124999163, 17.29062499938548214, 26.74683588394047007 ) ) ;
#43374 = CARTESIAN_POINT ( 'NONE',  ( 15.98437500061451821, -4.541064518000419881, 2.621784821874995952 ) ) ;
#43375 = CARTESIAN_POINT ( 'NONE',  ( 13.69687500061451679, -3.027376345333614438, 5.243569643749998122 ) ) ;
#43376 = CARTESIAN_POINT ( 'NONE',  ( 23.74687500061451573, -3.027376345333610441, -5.243569643749999898 ) ) ;
#43377 = CARTESIAN_POINT ( 'NONE',  ( -3.000416591977282496E-16, 11.64687500061451786, 25.09994784771203058 ) ) ;
#43378 = CARTESIAN_POINT ( 'NONE',  ( 4.228125000614517681, -4.541064518000419881, 2.621784821874995952 ) ) ;
#43379 = CARTESIAN_POINT ( 'NONE',  ( 28.34062500061451928, 6.054752690667223547, 3.707466751127219781E-16 ) ) ;
#43380 = CARTESIAN_POINT ( 'NONE',  ( 26.84062500061451573, -3.027376345333610441, -5.243569643749999898 ) ) ;
#43381 = CARTESIAN_POINT ( 'NONE',  ( 8.400000001229035007, 5.773502691896255534, 3.535250795749688401E-16 ) ) ;
#43382 = CARTESIAN_POINT ( 'NONE',  ( 8.484601909799253346E-16, 19.66249999999999787, 34.61880215351700230 ) ) ;
#43383 = CARTESIAN_POINT ( 'NONE',  ( 8.221875000614518925, 3.027376345333611329, 5.243569643749999010 ) ) ;
#43384 = APPLICATION_PROTOCOL_DEFINITION ( 'draft international standard', 'automotive_design', 1998, #62028 ) ;
#43385 = CARTESIAN_POINT ( 'NONE',  ( 13.80000000122903181, 5.773502691896255534, 3.535250795749688894E-16 ) ) ;
#43386 = CARTESIAN_POINT ( 'NONE',  ( 8.775000001229033231, 2.886751345948129099, -4.999999999999998224 ) ) ;
#43387 = CARTESIAN_POINT ( 'NONE',  ( 5.728125000614515905, 6.421520780324663323E-16, -5.243569643749999010 ) ) ;
#43388 = CARTESIAN_POINT ( 'NONE',  ( -4.000000000000000888, 16.75624999877096855, 32.30940107675850470 ) ) ;
#43389 = CARTESIAN_POINT ( 'NONE',  ( 17.56875000122903074, -5.773502691896255534, -1.060575238724906372E-15 ) ) ;
#43390 = CARTESIAN_POINT ( 'NONE',  ( 14.40937500061451715, 4.541064518000418104, -2.621784821874998173 ) ) ;
#43391 = CARTESIAN_POINT ( 'NONE',  ( 21.31875000122903430, 2.886751345948129099, -4.999999999999997335 ) ) ;
#43392 = ORIENTED_EDGE ( 'NONE', *, *, #17585, .T. ) ;
#43393 = EDGE_CURVE ( 'NONE', #58790, #22068, #50589, .T. ) ;
#43394 = CARTESIAN_POINT ( 'NONE',  ( 21.21562500061451573, 3.027376345333611329, 5.243569643749999010 ) ) ;
#43395 = CARTESIAN_POINT ( 'NONE',  ( 7.190625000614518036, 6.054752690667223547, 3.707466751127219781E-16 ) ) ;
#43396 = CARTESIAN_POINT ( 'NONE',  ( 24.72187500061451360, 3.027376345333612662, -5.243569643749998122 ) ) ;
#43397 = CARTESIAN_POINT ( 'NONE',  ( 8.278125000614515727, -4.541064518000419881, 2.621784821874995952 ) ) ;
#43398 = CARTESIAN_POINT ( 'NONE',  ( 8.587500001229035007, -4.330127018922194537, 2.499999999999995559 ) ) ;
#43399 = CARTESIAN_POINT ( 'NONE',  ( 23.46562500061451573, 3.027376345333611329, 5.243569643749999010 ) ) ;
#43400 = CARTESIAN_POINT ( 'NONE',  ( -3.999999999999999556, 18.27500000122903501, -32.30940107675850470 ) ) ;
#43401 = CARTESIAN_POINT ( 'NONE',  ( 10.98750000122903536, 6.123233995736764310E-16, -4.999999999999998224 ) ) ;
#43402 = CARTESIAN_POINT ( 'NONE',  ( 20.84062500061451573, -3.027376345333614438, 5.243569643749998122 ) ) ;
#43403 = CARTESIAN_POINT ( 'NONE',  ( 16.56562500061451715, 3.027376345333613106, -5.243569643749998122 ) ) ;
#43404 = CARTESIAN_POINT ( 'NONE',  ( 27.94687500061451502, 5.492252693125287522, 3.363034840372157021E-16 ) ) ;
#43405 = CARTESIAN_POINT ( 'NONE',  ( 14.73749999999999893, -2.886751345948129988, 4.999999999999997335 ) ) ;
#43406 = CARTESIAN_POINT ( 'NONE',  ( 10.20000000122903572, 5.773502691896255534, 3.535250795749688894E-16 ) ) ;
#43407 = AXIS2_PLACEMENT_3D ( 'NONE', #69005, #53460, #7302 ) ;
#43408 = CARTESIAN_POINT ( 'NONE',  ( 8.053125000614516082, 4.541064518000418104, -2.621784821874998173 ) ) ;
#43409 = CARTESIAN_POINT ( 'NONE',  ( 12.06562500061451537, 3.027376345333613106, -5.243569643749998122 ) ) ;
#43410 = CARTESIAN_POINT ( 'NONE',  ( 22.08750000122903501, -4.330127018922194537, 2.499999999999995559 ) ) ;
#43411 = CARTESIAN_POINT ( 'NONE',  ( 20.40937500061451715, 0.000000000000000000, 5.243569643749999010 ) ) ;
#43412 = CARTESIAN_POINT ( 'NONE',  ( 4.715625000614516615, -6.054752690667223547, -1.112240025338166033E-15 ) ) ;
#43413 = EDGE_CURVE ( 'NONE', #44627, #4916, #61377, .T. ) ;
#43414 = CARTESIAN_POINT ( 'NONE',  ( 5.025000001229035895, -5.773502691896255534, -1.060575238724906372E-15 ) ) ;
#43415 = CARTESIAN_POINT ( 'NONE',  ( 3.571875000614517237, 3.027376345333613106, -5.243569643749998122 ) ) ;
#43416 = CARTESIAN_POINT ( 'NONE',  ( 22.24687500061451217, -3.027376345333614438, 5.243569643749998122 ) ) ;
#43417 =( BOUNDED_SURFACE ( )  B_SPLINE_SURFACE ( 1, 2, ( 
 ( #10327, #51302, #16582, #56480, #10689, #56124, #4791, #67221, #32861, #5517, #5152, #28404, #17310, #62381, #27324, #50941, #39497, #49858, #72382, #72750, #44691, #33937, #28055, #50583, #22493, #340, #22847, #28763, #45400, #11781, #34296, #56828, #704, #23212, #63103, #7681, #51667, #24665, #1796, #29853, #12857, #40583, #2506, #41312, #25029, #53109, #52389, #35390, #47572, #58641, #68663, #58274, #23580, #30217, #23938, #40955, #13215, #46125, #70102, #24306, #46853, #40222, #18026, #62744, #57915, #1432, #52751, #69394, #2154, #7322, #6605, #18748, #12137, #34662, #63822, #57191, #35753, #47211, #69743, #57559, #19111, #30583, #1072, #41667, #12503, #46487, #64189, #13576, #35031, #69026, #6962, #29134, #36121, #29493, #52029, #8049, #18388, #63470, #9874, #19850, #54216, #49407, #4351, #36485, #59737, #20210, #19477, #36849, #59004, #48311, #32408, #8409, #42035, #37216, #3613, #47944, #3245, #42401, #26878, #71574, #54946, #64559, #20948, #54577, #70835, #13948, #64923, #26134, #30938, #53479, #2871, #9146, #42764, #25402, #59365, #70473, #65284, #14313, #8776, #31311, #53853, #25773, #43501, #14672, #15404, #31682, #66026, #48675, #71199, #20574, #60465, #43130, #65653, #15043, #37580, #60103, #9512, #32045, #3981, #26505, #49046, #37946, #5069, #6151, #44608, #44236, #67496, #5790, #28322, #15769, #16859, #50500, #38311, #28680, #66767, #72299, #27970, #56747, #4707, #10967, #27238, #61211, #17225, #66392, #61935, #22047, #5430, #22411, #55672, #21679, #39414, #10243, #56400, #33490, #61565, #67138, #16140, #34213, #73027, #71939, #11697, #56038, #16496, #21315, #39785, #49775, #11340, #55313, #33856, #27604, #72668, #44958, #38692, #43868, #50859, #257, #60838, #10606, #32776, #39051, #33135, #22766, #45317, #67852, #62301, #50137, #68936, #37030, #59554, #35303, #68218, #57826, #53292, #70289, #68576, #36666, #42579, #62657, #7235, #12053, #12412, #622, #51220, #46040, #53664, #63014, #48126, #34577, #3056, #17936, #29049, #30760, #20024, #17580, #2691, #1340, #34945, #8965, #65106, #6877, #47754, #6516, #46400, #45685, #57472, #23129, #23852, #23493, #19661, #59185, #8595, #40141, #42216, #25206, #57105, #51585, #40498, #985, #64740, #29410, #51943, #63383, #18294, #40866, #70649, #12768, #14128, #31124, #25587, #14495, #15224, #54399, #72115, #42945, #15954, #66207, #21131, #4165, #31864, #66952, #32595, #16320, #44425, #43684, #26695, #38873, #49953, #59925, #49590, #14862, #21498, #37763, #32227, #4532, #37401, #61391, #15585, #38127, #31499, #9331, #54039, #49229, #65841, #44051, #60648, #66575, #71762, #71018, #10063, #3435, #25954, #55133, #48494, #27060, #38502, #61028, #48859, #10426, #21864, #65472, #32957, #3798, #60281, #55493, #4887, #26321, #9694, #71390, #20396, #27423, #20764, #43321, #72478, #54761, #39597, #1161, #11151, #45502, #40676, #68755, #27788, #51036, #11511, #10785, #28150, #50325, #62119, #23670, #72849, #34394, #67671, #33678, #51397, #22230, #68391, #68033, #433, #56570, #56221, #46216, #11871, #18113, #33318, #22941, #5967, #55857, #29227, #39235, #28858, #67319, #800, #17039, #34033, #56924, #16679, #5246, #17403, #39960, #44786, #61747, #5614, #28499, #45138, #23308, #62474, #45856, #6328, #50678, #17752, #82, #22587, #40311, #62834, #12227, #34755, #57291, #6696, #51762, #53570, #1524, #69836, #24030, #24396, #7777, #24758, #18481, #46945, #12947, #70566, #42127, #25495, #19941, #64653, #25118, #18840, #2967, #63560, #47300, #63196, #48041, #7056, #30312, #63918, #12592, #7413, #29584, #41402, #35125, #52122, #57649, #46579, #58005, #14037, #1891, #59098, #69123, #36578, #29941, #41047, #19201, #31034, #35484, #64283, #13303, #69482, #52481, #35840, #58365, #58731, #52844, #2242, #41755, #13672, #36216, #8143, #30669, #53202, #70194, #19571, #2598, #47661, #8505, #59464, #72387, #37313, #42858, #71668, #27332, #48408, #54671, #70934, #31777, #60931, #36944, #32504, #65751, #49140, #43595, #3346, #21405, #14769, #49864, #25868, #49499, #43231, #15135, #55040, #59837, #15862, #42495, #26970, #8873, #4442, #66483, #72029, #9968, #66116, #43962, #32138, #37673, #38037, #20304, #26601, #60195, #38409, #10335, #65380, #53949, #21043, #54316, #9242, #32867, #31409, #9606, #55403, #71295, #65018, #3707, #26234, #15495, #14407, #48771, #20674, #4074, #60561, #4798, #57198, #21768, #56130, #17316, #29141, #5158, #39877, #67228, #23220, #6613, #62388, #45050, #61657, #51674, #27693, #34670, #10695, #11056, #33227, #50232, #55766, #347, #39140, #68309, #5880, #11787, #56487, #62029, #44331, #66860, #45773, #72756, #16231, #11427, #45408, #22142, #16588, #28412, #34304, #44695, #50950, #51309, #5523, #56835, #6243, #22853, #38784, #12144, #17668, #33584, #28770, #61301, #28061, #713, #50591, #40229, #62751, #73117, #22501, #67943, #67585, #16951, #39504, #33945, #58281, #63477, #52396, #7688, #1439, #36492, #30225, #46494, #12865, #18395, #69033, #1803, #63829, #19118, #18755, #40962, #47579, #30945, #58648, #18034, #13583, #25036, #36129, #41673, #2161, #53116, #13221, #69400, #69750, #52036, #52758, #41319, #64196, #8056, #35038, #12510, #24672, #35396, #57566, #30591, #40590, #24313, #2514, #29860, #1079, #63111, #6969, #47218, #8415, #29500, #23945, #57922, #35760, #70109, #59012, #23587, #7329, #19485, #46132, #46861, #42043, #64566, #13954, #68670, #71579, #3619, #20216, #38316, #36856, #66398, #42408, #42770, #64930, #59372, #14321, #32051, #70841, #26883, #37587, #20953, #15049, #20581, #60843, #10248, #54951, #8783, #2878, #43136, #3987, #31317, #25780, #60109, #43506, #53861, #9519, #9879, #37222, #49052, #15409, #54583, #53486, #43873, #49412, #3252, #60471, #19857, #14678, #66031, #65290, #37952, #32414 ),
 ( #25409, #48318, #65660, #59744, #9152, #71943, #47952, #4357, #26140, #26512, #21320, #31687, #15775, #70480, #54222, #48681, #71205, #17587, #16145, #45690, #21685, #22053, #44242, #38697, #66772, #11343, #50144, #6155, #16863, #50863, #67500, #73031, #40146, #62662, #34217, #61216, #55318, #22415, #56404, #10611, #5074, #39418, #261, #33140, #61940, #62306, #16502, #28325, #67856, #33861, #32781, #23134, #28685, #55677, #39789, #72304, #67143, #22770, #72673, #45322, #11701, #27244, #17229, #5794, #56751, #51224, #628, #39056, #68224, #44613, #10972, #4712, #27609, #49780, #61569, #33494, #56043, #5435, #27974, #50504, #44962, #30132, #29769, #13129, #46046, #64100, #57477, #19387, #68581, #19023, #12773, #57831, #2071, #6882, #58552, #41948, #69658, #29054, #24580, #36034, #47127, #52664, #35668, #13485, #1705, #7240, #7594, #63019, #69304, #52304, #41583, #7962, #17941, #23498, #18666, #1347, #40504, #30498, #51590, #35308, #53026, #40871, #12059, #990, #12418, #63738, #34582, #34950, #29415, #23857, #24220, #46769, #47486, #57110, #46404, #2420, #6521, #51948, #24942, #68942, #41227, #18300, #63388, #70017, #58191, #14589, #26416, #20123, #64469, #53390, #47857, #43042, #71855, #2786, #70386, #3159, #31595, #3528, #26790, #13862, #25688, #60017, #21228, #19762, #9429, #36763, #65940, #49324, #31957, #37123, #31221, #36404, #42312, #4266, #25310, #53764, #64839, #14226, #59281, #65569, #8689, #37859, #48589, #54495, #26049, #54133, #58916, #8325, #15320, #48222, #30855, #71115, #14958, #70746, #42677, #20487, #3896, #65200, #37497, #20865, #59652, #48958, #71488, #43416, #9062, #54857, #60380, #9788, #32322, #10160, #4985, #11253, #61128, #61847, #22683, #38222, #33776, #67414, #50419, #67766, #28244, #27517, #27885, #16054, #39333, #50775, #178, #60751, #56319, #22326, #32694, #535, #38602, #44150, #72945, #28600, #49689, #55951, #72218, #33051, #62218, #55231, #5709, #67055, #44879, #16776, #50051, #66679, #45234, #4626, #17140, #5347, #33413, #16414, #10523, #6066, #39700, #51136, #56670, #11613, #38970, #43780, #34131, #21596, #66307, #27155, #15684, #55590, #61486, #72579, #10882, #21964, #44522, #7152, #40059, #29682, #24130, #41145, #40413, #7508, #13394, #34494, #52218, #57022, #57386, #40781, #57745, #51500, #6792, #45956, #30412, #1986, #58464, #52940, #24497, #58103, #51857, #35942, #23409, #1621, #23044, #7876, #62574, #63295, #23764, #45602, #62930, #11970, #1259, #68135, #6428, #17499, #28962, #17851, #47040, #34859, #18937, #901, #69575, #12323, #68488, #46680, #64017, #29327, #69219, #46317, #68853, #18210, #12687, #35224, #18579, #63653, #13044, #35582, #30039, #52578, #41495, #47764, #71030, #9343, #31875, #19302, #20407, #54050, #41855, #32237, #70300, #2702, #31510, #60292, #8241, #14506, #30771, #64750, #20775, #69932, #65484, #25598, #8977, #25964, #59195, #25217, #42955, #13775, #59936, #37040, #65116, #48135, #19672, #37773, #3445, #9703, #15236, #59564, #70660, #2337, #43331, #53302, #14873, #58831, #37413, #8605, #3068, #48504, #42226, #24855, #54410, #3810, #47400, #14140, #64383, #20034, #36676, #26332, #48870, #65853, #31134, #71401, #53675, #36316, #42590, #55503, #28778, #38137, #40598, #17325, #62397, #54771, #60659, #4176, #355, #15964, #723, #39884, #68317, #49965, #21142, #22862, #63120, #12516, #11795, #71772, #34312, #56845, #23229, #72128, #40236, #46141, #66217, #6251, #15594, #38514, #45417, #51319, #10074, #61038, #4541, #26705, #34678, #18041, #49239, #57207, #17677, #10436, #68680, #55143, #45782, #43695, #32605, #27069, #67953, #4899, #49601, #21507, #44060, #32966, #66587, #27434, #62759, #12151, #6622, #29150, #51684, #1088, #23595, #59021, #29867, #12873, #64204, #2886, #52044, #36138, #58290, #18763, #64938, #25416, #63838, #30598, #63485, #30234, #40970, #58657, #7697, #42418, #7338, #53125, #42051, #64574, #1448, #2524, #13591, #23953, #35047, #52404, #35405, #8064, #19865, #57931, #47227, #1812, #24320, #53494, #29509, #25045, #52766, #41681, #47588, #41329, #46868, #70117, #46503, #19494, #69759, #24680, #2169, #69408, #70488, #13963, #57575, #47960, #19127, #36500, #6978, #18403, #8422, #69041, #13229, #35768, #30958, #54593, #26522, #49788, #14329, #48689, #9888, #21694, #70851, #32423, #59753, #15784, #72313, #54960, #37596, #54230, #44251, #20224, #27255, #3260, #3627, #25789, #42778, #48326, #66039, #31695, #60854, #71588, #4365, #49060, #3995, #36864, #59382, #38326, #65298, #8793, #20961, #37960, #14688, #9160, #43516, #26894, #37230, #15417, #43882, #71213, #49420, #71953, #60480, #31326, #4721, #10258, #26149, #21329, #53869, #20590, #66408, #43147, #32790, #55327, #65669, #15058, #60117, #9527, #32059, #67866, #23143, #27618, #44622, #44970, #50871, #67152, #29064, #269, #39065, #56052, #10982, #61579, #67508, #56412, #11710, #11351, #17238, #50152, #45698, #33503, #1000, #72682, #636, #16873, #39427, #56759, #5444, #40154, #23507, #51232, #10620, #6164, #17595, #28693, #34226, #39798, #68231, #5803, #61947, #62314, #16512, #22779, #33869, #62673, #12068, #22064, #5083, #45330, #27984, #50514, #34591, #33150, #28333, #57119, #22423, #66782, #55687, #6531, #16154, #51600, #73040, #38706, #61226, #36046, #29780, #46781, #19037, #29424, #30867, #7606, #52675, #46056, #51959, #68590, #63751, #7251, #64113, #30144, #58567, #41239, #12428, #13140, #53405, #2797, #2083, #63029, #24592, #47140, #13499, #63398, #30510, #36414, #57489, #69671, #6893, #52316, #35679, #41595, #1359, #1719, #68953, #17952, #24955, #8337, #40514, #47498, #7974, #24231, #58929, #46416, #53037, #34962, #23868, #18311, #58202, #69316, #40882, #12783, #35320, #18677, #57842, #2432, #70029, #19401, #41960, #64482, #13875 ) ),
 .UNSPECIFIED., .F., .F., .F. ) 
 B_SPLINE_SURFACE_WITH_KNOTS ( ( 2, 2 ),
 ( 3, 2, 2, 2, 2, 2, 2, 2, 2, 2, 2, 2, 2, 2, 2, 2, 2, 2, 2, 2, 2, 2, 2, 2, 2, 2, 2, 2, 2, 2, 2, 2, 2, 2, 2, 2, 2, 2, 2, 2, 2, 2, 2, 2, 2, 2, 2, 2, 2, 2, 2, 2, 2, 2, 2, 2, 2, 2, 2, 2, 2, 2, 2, 2, 2, 2, 2, 2, 2, 2, 2, 2, 2, 2, 2, 2, 2, 2, 2, 2, 2, 2, 2, 2, 2, 2, 2, 2, 2, 2, 2, 2, 2, 2, 2, 2, 2, 2, 2, 2, 2, 2, 2, 2, 2, 2, 2, 2, 2, 2, 2, 2, 2, 2, 2, 2, 2, 2, 2, 2, 2, 2, 2, 2, 2, 2, 2, 2, 2, 2, 2, 2, 2, 2, 2, 2, 2, 2, 2, 2, 2, 2, 2, 2, 2, 2, 2, 2, 2, 2, 2, 2, 2, 2, 2, 2, 2, 2, 2, 2, 2, 2, 2, 2, 2, 2, 2, 2, 2, 2, 2, 2, 2, 2, 2, 2, 2, 2, 2, 2, 2, 2, 2, 2, 2, 2, 2, 2, 2, 2, 2, 2, 2, 2, 2, 2, 2, 2, 2, 2, 2, 2, 2, 2, 2, 2, 2, 2, 2, 2, 2, 2, 2, 2, 2, 2, 2, 2, 2, 2, 2, 2, 2, 2, 2, 2, 2, 2, 2, 2, 2, 2, 2, 2, 2, 2, 2, 2, 2, 2, 2, 2, 2, 2, 2, 2, 2, 2, 2, 2, 2, 2, 2, 2, 2, 2, 2, 2, 2, 2, 2, 2, 2, 2, 2, 2, 2, 2, 2, 2, 2, 2, 2, 2, 2, 2, 2, 2, 2, 2, 2, 2, 2, 2, 2, 2, 2, 2, 2, 2, 2, 2, 2, 2, 2, 2, 2, 2, 2, 2, 2, 2, 2, 2, 2, 2, 2, 2, 2, 2, 2, 2, 2, 2, 2, 2, 2, 2, 2, 2, 2, 2, 2, 2, 2, 2, 2, 2, 2, 2, 2, 2, 2, 2, 2, 2, 2, 2, 2, 2, 2, 2, 2, 2, 2, 2, 2, 2, 2, 2, 2, 2, 2, 2, 2, 2, 2, 2, 2, 2, 3 ),
 ( 0.000000000000000000, 1.000000000000000000 ),
 ( 0.000000000000000000, 0.002777777777777777884, 0.005555555555555555768, 0.008333333333333333218, 0.01111111111111111154, 0.01388888888888888812, 0.01666666666666666644, 0.01944444444444444475, 0.02222222222222222307, 0.02500000000000000139, 0.02777777777777777624, 0.03055555555555555455, 0.03333333333333333287, 0.03611111111111110772, 0.03888888888888888951, 0.04166666666666666435, 0.04444444444444444614, 0.04722222222222222099, 0.05000000000000000278, 0.05277777777777777762, 0.05555555555555555247, 0.05833333333333333426, 0.06111111111111110911, 0.06388888888888888395, 0.06666666666666666574, 0.06944444444444444753, 0.07222222222222221544, 0.07499999999999999722, 0.07777777777777777901, 0.08055555555555556080, 0.08333333333333332871, 0.08611111111111111049, 0.08888888888888889228, 0.09166666666666666019, 0.09444444444444444198, 0.09722222222222222376, 0.1000000000000000056, 0.1027777777777777735, 0.1055555555555555552, 0.1083333333333333370, 0.1111111111111111049, 0.1138888888888888867, 0.1166666666666666685, 0.1194444444444444503, 0.1222222222222222182, 0.1250000000000000000, 0.1277777777777777679, 0.1305555555555555636, 0.1333333333333333315, 0.1361111111111110994, 0.1388888888888888951, 0.1416666666666666630, 0.1444444444444444309, 0.1472222222222222265, 0.1499999999999999944, 0.1527777777777777901, 0.1555555555555555580, 0.1583333333333333259, 0.1611111111111111216, 0.1638888888888888895, 0.1666666666666666574, 0.1694444444444444531, 0.1722222222222222210, 0.1749999999999999889, 0.1777777777777777846, 0.1805555555555555525, 0.1833333333333333204, 0.1861111111111111160, 0.1888888888888888840, 0.1916666666666666796, 0.1944444444444444475, 0.1972222222222222154, 0.2000000000000000111, 0.2027777777777777790, 0.2055555555555555469, 0.2083333333333333426, 0.2111111111111111105, 0.2138888888888888784, 0.2166666666666666741, 0.2194444444444444420, 0.2222222222222222099, 0.2250000000000000056, 0.2277777777777777735, 0.2305555555555555691, 0.2333333333333333370, 0.2361111111111111049, 0.2388888888888889006, 0.2416666666666666685, 0.2444444444444444364, 0.2472222222222222321, 0.2500000000000000000, 0.2527777777777777679, 0.2555555555555555358, 0.2583333333333333592, 0.2611111111111111271, 0.2638888888888888951, 0.2666666666666666630, 0.2694444444444444309, 0.2722222222222221988, 0.2750000000000000222, 0.2777777777777777901, 0.2805555555555555580, 0.2833333333333333259, 0.2861111111111110938, 0.2888888888888888618, 0.2916666666666666852, 0.2944444444444444531, 0.2972222222222222210, 0.2999999999999999889, 0.3027777777777777568, 0.3055555555555555802, 0.3083333333333333481, 0.3111111111111111160, 0.3138888888888888840, 0.3166666666666666519, 0.3194444444444444198, 0.3222222222222222432, 0.3250000000000000111, 0.3277777777777777790, 0.3305555555555555469, 0.3333333333333333148, 0.3361111111111111382, 0.3388888888888889062, 0.3416666666666666741, 0.3444444444444444420, 0.3472222222222222099, 0.3499999999999999778, 0.3527777777777778012, 0.3555555555555555691, 0.3583333333333333370, 0.3611111111111111049, 0.3638888888888888729, 0.3666666666666666408, 0.3694444444444444642, 0.3722222222222222321, 0.3750000000000000000, 0.3777777777777777679, 0.3805555555555555358, 0.3833333333333333592, 0.3861111111111111271, 0.3888888888888888951, 0.3916666666666666630, 0.3944444444444444309, 0.3972222222222221988, 0.4000000000000000222, 0.4027777777777777901, 0.4055555555555555580, 0.4083333333333333259, 0.4111111111111110938, 0.4138888888888888618, 0.4166666666666666852, 0.4194444444444444531, 0.4222222222222222210, 0.4249999999999999889, 0.4277777777777777568, 0.4305555555555555802, 0.4333333333333333481, 0.4361111111111111160, 0.4388888888888888840, 0.4416666666666666519, 0.4444444444444444198, 0.4472222222222222432, 0.4500000000000000111, 0.4527777777777777790, 0.4555555555555555469, 0.4583333333333333148, 0.4611111111111111382, 0.4638888888888889062, 0.4666666666666666741, 0.4694444444444444420, 0.4722222222222222099, 0.4749999999999999778, 0.4777777777777778012, 0.4805555555555555691, 0.4833333333333333370, 0.4861111111111111049, 0.4888888888888888729, 0.4916666666666666408, 0.4944444444444444642, 0.4972222222222222321, 0.5000000000000000000, 0.5027777777777777679, 0.5055555555555555358, 0.5083333333333333037, 0.5111111111111110716, 0.5138888888888888395, 0.5166666666666667185, 0.5194444444444444864, 0.5222222222222222543, 0.5250000000000000222, 0.5277777777777777901, 0.5305555555555555580, 0.5333333333333333259, 0.5361111111111110938, 0.5388888888888888618, 0.5416666666666666297, 0.5444444444444443976, 0.5472222222222222765, 0.5500000000000000444, 0.5527777777777778123, 0.5555555555555555802, 0.5583333333333333481, 0.5611111111111111160, 0.5638888888888888840, 0.5666666666666666519, 0.5694444444444444198, 0.5722222222222221877, 0.5749999999999999556, 0.5777777777777777235, 0.5805555555555556024, 0.5833333333333333703, 0.5861111111111111382, 0.5888888888888889062, 0.5916666666666666741, 0.5944444444444444420, 0.5972222222222222099, 0.5999999999999999778, 0.6027777777777777457, 0.6055555555555555136, 0.6083333333333332815, 0.6111111111111111605, 0.6138888888888889284, 0.6166666666666666963, 0.6194444444444444642, 0.6222222222222222321, 0.6250000000000000000, 0.6277777777777777679, 0.6305555555555555358, 0.6333333333333333037, 0.6361111111111110716, 0.6388888888888888395, 0.6416666666666667185, 0.6444444444444444864, 0.6472222222222222543, 0.6500000000000000222, 0.6527777777777777901, 0.6555555555555555580, 0.6583333333333333259, 0.6611111111111110938, 0.6638888888888888618, 0.6666666666666666297, 0.6694444444444443976, 0.6722222222222222765, 0.6750000000000000444, 0.6777777777777778123, 0.6805555555555555802, 0.6833333333333333481, 0.6861111111111111160, 0.6888888888888888840, 0.6916666666666666519, 0.6944444444444444198, 0.6972222222222221877, 0.6999999999999999556, 0.7027777777777777235, 0.7055555555555556024, 0.7083333333333333703, 0.7111111111111111382, 0.7138888888888889062, 0.7166666666666666741, 0.7194444444444444420, 0.7222222222222222099, 0.7249999999999999778, 0.7277777777777777457, 0.7305555555555555136, 0.7333333333333332815, 0.7361111111111111605, 0.7388888888888889284, 0.7416666666666666963, 0.7444444444444444642, 0.7472222222222222321, 0.7500000000000000000, 0.7527777777777777679, 0.7555555555555555358, 0.7583333333333333037, 0.7611111111111110716, 0.7638888888888888395, 0.7666666666666667185, 0.7694444444444444864, 0.7722222222222222543, 0.7750000000000000222, 0.7777777777777777901, 0.7805555555555555580, 0.7833333333333333259, 0.7861111111111110938, 0.7888888888888888618, 0.7916666666666666297, 0.7944444444444443976, 0.7972222222222222765, 0.8000000000000000444, 0.8027777777777778123, 0.8055555555555555802, 0.8083333333333333481, 0.8111111111111111160, 0.8138888888888888840, 0.8166666666666666519, 0.8194444444444444198, 0.8222222222222221877, 0.8249999999999999556, 0.8277777777777777235, 0.8305555555555556024, 0.8333333333333333703, 0.8361111111111111382, 0.8388888888888889062, 0.8416666666666666741, 0.8444444444444444420, 0.8472222222222222099, 0.8499999999999999778, 0.8527777777777777457, 0.8555555555555555136, 0.8583333333333332815, 0.8611111111111111605, 0.8638888888888889284, 0.8666666666666666963, 0.8694444444444444642, 0.8722222222222222321, 0.8750000000000000000, 0.8777777777777777679, 0.8805555555555555358, 0.8833333333333333037, 0.8861111111111110716, 0.8888888888888888395, 0.8916666666666667185, 0.8944444444444444864, 0.8972222222222222543, 0.9000000000000000222, 0.9027777777777777901, 0.9055555555555555580, 0.9083333333333333259, 0.9111111111111110938, 0.9138888888888888618, 0.9166666666666666297, 0.9194444444444443976, 0.9222222222222222765, 0.9250000000000000444, 0.9277777777777778123, 0.9305555555555555802, 0.9333333333333333481, 0.9361111111111111160, 0.9388888888888888840, 0.9416666666666666519, 0.9444444444444444198, 0.9472222222222221877, 0.9499999999999999556, 0.9527777777777777235, 0.9555555555555556024, 0.9583333333333333703, 0.9611111111111111382, 0.9638888888888889062, 0.9666666666666666741, 0.9694444444444444420, 0.9722222222222222099, 0.9749999999999999778, 0.9777777777777777457, 0.9805555555555555136, 0.9833333333333332815, 0.9861111111111111605, 0.9888888888888889284, 0.9916666666666666963, 0.9944444444444444642, 0.9972222222222222321, 1.000000000000000000 ),
 .UNSPECIFIED. ) 
 GEOMETRIC_REPRESENTATION_ITEM ( )  RATIONAL_B_SPLINE_SURFACE ( (
 ( 1.000000000000000000, 0.8660254037844387076, 1.000000000000000000, 0.8660254037844387076, 1.000000000000000000, 0.8660254037844387076, 1.000000000000000000, 0.8660254037844387076, 1.000000000000000000, 0.8660254037844387076, 1.000000000000000000, 0.8660254037844387076, 1.000000000000000000, 0.8660254037844387076, 1.000000000000000000, 0.8660254037844387076, 1.000000000000000000, 0.8660254037844387076, 1.000000000000000000, 0.8660254037844387076, 1.000000000000000000, 0.8660254037844387076, 1.000000000000000000, 0.8660254037844387076, 1.000000000000000000, 0.8660254037844387076, 1.000000000000000000, 0.8660254037844387076, 1.000000000000000000, 0.8660254037844387076, 1.000000000000000000, 0.8660254037844387076, 1.000000000000000000, 0.8660254037844387076, 1.000000000000000000, 0.8660254037844387076, 1.000000000000000000, 0.8660254037844387076, 1.000000000000000000, 0.8660254037844387076, 1.000000000000000000, 0.8660254037844387076, 1.000000000000000000, 0.8660254037844387076, 1.000000000000000000, 0.8660254037844387076, 1.000000000000000000, 0.8660254037844387076, 1.000000000000000000, 0.8660254037844387076, 1.000000000000000000, 0.8660254037844387076, 1.000000000000000000, 0.8660254037844387076, 1.000000000000000000, 0.8660254037844387076, 1.000000000000000000, 0.8660254037844387076, 1.000000000000000000, 0.8660254037844387076, 1.000000000000000000, 0.8660254037844387076, 1.000000000000000000, 0.8660254037844387076, 1.000000000000000000, 0.8660254037844387076, 1.000000000000000000, 0.8660254037844387076, 1.000000000000000000, 0.8660254037844387076, 1.000000000000000000, 0.8660254037844387076, 1.000000000000000000, 0.8660254037844387076, 1.000000000000000000, 0.8660254037844387076, 1.000000000000000000, 0.8660254037844387076, 1.000000000000000000, 0.8660254037844387076, 1.000000000000000000, 0.8660254037844387076, 1.000000000000000000, 0.8660254037844387076, 1.000000000000000000, 0.8660254037844387076, 1.000000000000000000, 0.8660254037844387076, 1.000000000000000000, 0.8660254037844387076, 1.000000000000000000, 0.8660254037844387076, 1.000000000000000000, 0.8660254037844387076, 1.000000000000000000, 0.8660254037844387076, 1.000000000000000000, 0.8660254037844387076, 1.000000000000000000, 0.8660254037844387076, 1.000000000000000000, 0.8660254037844387076, 1.000000000000000000, 0.8660254037844387076, 1.000000000000000000, 0.8660254037844387076, 1.000000000000000000, 0.8660254037844387076, 1.000000000000000000, 0.8660254037844387076, 1.000000000000000000, 0.8660254037844387076, 1.000000000000000000, 0.8660254037844387076, 1.000000000000000000, 0.8660254037844387076, 1.000000000000000000, 0.8660254037844387076, 1.000000000000000000, 0.8660254037844387076, 1.000000000000000000, 0.8660254037844387076, 1.000000000000000000, 0.8660254037844387076, 1.000000000000000000, 0.8660254037844387076, 1.000000000000000000, 0.8660254037844387076, 1.000000000000000000, 0.8660254037844387076, 1.000000000000000000, 0.8660254037844387076, 1.000000000000000000, 0.8660254037844387076, 1.000000000000000000, 0.8660254037844387076, 1.000000000000000000, 0.8660254037844387076, 1.000000000000000000, 0.8660254037844387076, 1.000000000000000000, 0.8660254037844387076, 1.000000000000000000, 0.8660254037844387076, 1.000000000000000000, 0.8660254037844387076, 1.000000000000000000, 0.8660254037844387076, 1.000000000000000000, 0.8660254037844387076, 1.000000000000000000, 0.8660254037844387076, 1.000000000000000000, 0.8660254037844387076, 1.000000000000000000, 0.8660254037844387076, 1.000000000000000000, 0.8660254037844387076, 1.000000000000000000, 0.8660254037844387076, 1.000000000000000000, 0.8660254037844387076, 1.000000000000000000, 0.8660254037844387076, 1.000000000000000000, 0.8660254037844387076, 1.000000000000000000, 0.8660254037844387076, 1.000000000000000000, 0.8660254037844387076, 1.000000000000000000, 0.8660254037844387076, 1.000000000000000000, 0.8660254037844387076, 1.000000000000000000, 0.8660254037844387076, 1.000000000000000000, 0.8660254037844387076, 1.000000000000000000, 0.8660254037844387076, 1.000000000000000000, 0.8660254037844387076, 1.000000000000000000, 0.8660254037844387076, 1.000000000000000000, 0.8660254037844387076, 1.000000000000000000, 0.8660254037844387076, 1.000000000000000000, 0.8660254037844387076, 1.000000000000000000, 0.8660254037844387076, 1.000000000000000000, 0.8660254037844387076, 1.000000000000000000, 0.8660254037844387076, 1.000000000000000000, 0.8660254037844387076, 1.000000000000000000, 0.8660254037844387076, 1.000000000000000000, 0.8660254037844387076, 1.000000000000000000, 0.8660254037844387076, 1.000000000000000000, 0.8660254037844387076, 1.000000000000000000, 0.8660254037844387076, 1.000000000000000000, 0.8660254037844387076, 1.000000000000000000, 0.8660254037844387076, 1.000000000000000000, 0.8660254037844387076, 1.000000000000000000, 0.8660254037844387076, 1.000000000000000000, 0.8660254037844387076, 1.000000000000000000, 0.8660254037844387076, 1.000000000000000000, 0.8660254037844387076, 1.000000000000000000, 0.8660254037844387076, 1.000000000000000000, 0.8660254037844387076, 1.000000000000000000, 0.8660254037844387076, 1.000000000000000000, 0.8660254037844387076, 1.000000000000000000, 0.8660254037844387076, 1.000000000000000000, 0.8660254037844387076, 1.000000000000000000, 0.8660254037844387076, 1.000000000000000000, 0.8660254037844387076, 1.000000000000000000, 0.8660254037844387076, 1.000000000000000000, 0.8660254037844387076, 1.000000000000000000, 0.8660254037844387076, 1.000000000000000000, 0.8660254037844387076, 1.000000000000000000, 0.8660254037844387076, 1.000000000000000000, 0.8660254037844387076, 1.000000000000000000, 0.8660254037844387076, 1.000000000000000000, 0.8660254037844387076, 1.000000000000000000, 0.8660254037844387076, 1.000000000000000000, 0.8660254037844387076, 1.000000000000000000, 0.8660254037844387076, 1.000000000000000000, 0.8660254037844387076, 1.000000000000000000, 0.8660254037844387076, 1.000000000000000000, 0.8660254037844387076, 1.000000000000000000, 0.8660254037844387076, 1.000000000000000000, 0.8660254037844387076, 1.000000000000000000, 0.8660254037844387076, 1.000000000000000000, 0.8660254037844387076, 1.000000000000000000, 0.8660254037844387076, 1.000000000000000000, 0.8660254037844387076, 1.000000000000000000, 0.8660254037844387076, 1.000000000000000000, 0.8660254037844387076, 1.000000000000000000, 0.8660254037844387076, 1.000000000000000000, 0.8660254037844387076, 1.000000000000000000, 0.8660254037844387076, 1.000000000000000000, 0.8660254037844387076, 1.000000000000000000, 0.8660254037844387076, 1.000000000000000000, 0.8660254037844387076, 1.000000000000000000, 0.8660254037844387076, 1.000000000000000000, 0.8660254037844387076, 1.000000000000000000, 0.8660254037844387076, 1.000000000000000000, 0.8660254037844387076, 1.000000000000000000, 0.8660254037844387076, 1.000000000000000000, 0.8660254037844387076, 1.000000000000000000, 0.8660254037844387076, 1.000000000000000000, 0.8660254037844387076, 1.000000000000000000, 0.8660254037844387076, 1.000000000000000000, 0.8660254037844387076, 1.000000000000000000, 0.8660254037844387076, 1.000000000000000000, 0.8660254037844387076, 1.000000000000000000, 0.8660254037844387076, 1.000000000000000000, 0.8660254037844387076, 1.000000000000000000, 0.8660254037844387076, 1.000000000000000000, 0.8660254037844387076, 1.000000000000000000, 0.8660254037844387076, 1.000000000000000000, 0.8660254037844387076, 1.000000000000000000, 0.8660254037844387076, 1.000000000000000000, 0.8660254037844387076, 1.000000000000000000, 0.8660254037844387076, 1.000000000000000000, 0.8660254037844387076, 1.000000000000000000, 0.8660254037844387076, 1.000000000000000000, 0.8660254037844387076, 1.000000000000000000, 0.8660254037844387076, 1.000000000000000000, 0.8660254037844387076, 1.000000000000000000, 0.8660254037844387076, 1.000000000000000000, 0.8660254037844387076, 1.000000000000000000, 0.8660254037844387076, 1.000000000000000000, 0.8660254037844387076, 1.000000000000000000, 0.8660254037844387076, 1.000000000000000000, 0.8660254037844387076, 1.000000000000000000, 0.8660254037844387076, 1.000000000000000000, 0.8660254037844387076, 1.000000000000000000, 0.8660254037844387076, 1.000000000000000000, 0.8660254037844387076, 1.000000000000000000, 0.8660254037844387076, 1.000000000000000000, 0.8660254037844387076, 1.000000000000000000, 0.8660254037844387076, 1.000000000000000000, 0.8660254037844387076, 1.000000000000000000, 0.8660254037844387076, 1.000000000000000000, 0.8660254037844387076, 1.000000000000000000, 0.8660254037844387076, 1.000000000000000000, 0.8660254037844387076, 1.000000000000000000, 0.8660254037844387076, 1.000000000000000000, 0.8660254037844387076, 1.000000000000000000, 0.8660254037844387076, 1.000000000000000000, 0.8660254037844387076, 1.000000000000000000, 0.8660254037844387076, 1.000000000000000000, 0.8660254037844387076, 1.000000000000000000, 0.8660254037844387076, 1.000000000000000000, 0.8660254037844387076, 1.000000000000000000, 0.8660254037844387076, 1.000000000000000000, 0.8660254037844387076, 1.000000000000000000, 0.8660254037844387076, 1.000000000000000000, 0.8660254037844387076, 1.000000000000000000, 0.8660254037844387076, 1.000000000000000000, 0.8660254037844387076, 1.000000000000000000, 0.8660254037844387076, 1.000000000000000000, 0.8660254037844387076, 1.000000000000000000, 0.8660254037844387076, 1.000000000000000000, 0.8660254037844387076, 1.000000000000000000, 0.8660254037844387076, 1.000000000000000000, 0.8660254037844387076, 1.000000000000000000, 0.8660254037844387076, 1.000000000000000000, 0.8660254037844387076, 1.000000000000000000, 0.8660254037844387076, 1.000000000000000000, 0.8660254037844387076, 1.000000000000000000, 0.8660254037844387076, 1.000000000000000000, 0.8660254037844387076, 1.000000000000000000, 0.8660254037844387076, 1.000000000000000000, 0.8660254037844387076, 1.000000000000000000, 0.8660254037844387076, 1.000000000000000000, 0.8660254037844387076, 1.000000000000000000, 0.8660254037844387076, 1.000000000000000000, 0.8660254037844387076, 1.000000000000000000, 0.8660254037844387076, 1.000000000000000000, 0.8660254037844387076, 1.000000000000000000, 0.8660254037844387076, 1.000000000000000000, 0.8660254037844387076, 1.000000000000000000, 0.8660254037844387076, 1.000000000000000000, 0.8660254037844387076, 1.000000000000000000, 0.8660254037844387076, 1.000000000000000000, 0.8660254037844387076, 1.000000000000000000, 0.8660254037844387076, 1.000000000000000000, 0.8660254037844387076, 1.000000000000000000, 0.8660254037844387076, 1.000000000000000000, 0.8660254037844387076, 1.000000000000000000, 0.8660254037844387076, 1.000000000000000000, 0.8660254037844387076, 1.000000000000000000, 0.8660254037844387076, 1.000000000000000000, 0.8660254037844387076, 1.000000000000000000, 0.8660254037844387076, 1.000000000000000000, 0.8660254037844387076, 1.000000000000000000, 0.8660254037844387076, 1.000000000000000000, 0.8660254037844387076, 1.000000000000000000, 0.8660254037844387076, 1.000000000000000000, 0.8660254037844387076, 1.000000000000000000, 0.8660254037844387076, 1.000000000000000000, 0.8660254037844387076, 1.000000000000000000, 0.8660254037844387076, 1.000000000000000000, 0.8660254037844387076, 1.000000000000000000, 0.8660254037844387076, 1.000000000000000000, 0.8660254037844387076, 1.000000000000000000, 0.8660254037844387076, 1.000000000000000000, 0.8660254037844387076, 1.000000000000000000, 0.8660254037844387076, 1.000000000000000000, 0.8660254037844387076, 1.000000000000000000, 0.8660254037844387076, 1.000000000000000000, 0.8660254037844387076, 1.000000000000000000, 0.8660254037844387076, 1.000000000000000000, 0.8660254037844387076, 1.000000000000000000, 0.8660254037844387076, 1.000000000000000000, 0.8660254037844387076, 1.000000000000000000, 0.8660254037844387076, 1.000000000000000000, 0.8660254037844387076, 1.000000000000000000, 0.8660254037844387076, 1.000000000000000000, 0.8660254037844387076, 1.000000000000000000, 0.8660254037844387076, 1.000000000000000000, 0.8660254037844387076, 1.000000000000000000, 0.8660254037844387076, 1.000000000000000000, 0.8660254037844387076, 1.000000000000000000, 0.8660254037844387076, 1.000000000000000000, 0.8660254037844387076, 1.000000000000000000, 0.8660254037844387076, 1.000000000000000000, 0.8660254037844387076, 1.000000000000000000, 0.8660254037844387076, 1.000000000000000000, 0.8660254037844387076, 1.000000000000000000, 0.8660254037844387076, 1.000000000000000000, 0.8660254037844387076, 1.000000000000000000, 0.8660254037844387076, 1.000000000000000000, 0.8660254037844387076, 1.000000000000000000, 0.8660254037844387076, 1.000000000000000000, 0.8660254037844387076, 1.000000000000000000, 0.8660254037844387076, 1.000000000000000000, 0.8660254037844387076, 1.000000000000000000, 0.8660254037844387076, 1.000000000000000000, 0.8660254037844387076, 1.000000000000000000, 0.8660254037844387076, 1.000000000000000000, 0.8660254037844387076, 1.000000000000000000, 0.8660254037844387076, 1.000000000000000000, 0.8660254037844387076, 1.000000000000000000, 0.8660254037844387076, 1.000000000000000000, 0.8660254037844387076, 1.000000000000000000, 0.8660254037844387076, 1.000000000000000000, 0.8660254037844387076, 1.000000000000000000, 0.8660254037844387076, 1.000000000000000000, 0.8660254037844387076, 1.000000000000000000, 0.8660254037844387076, 1.000000000000000000, 0.8660254037844387076, 1.000000000000000000, 0.8660254037844387076, 1.000000000000000000, 0.8660254037844387076, 1.000000000000000000, 0.8660254037844387076, 1.000000000000000000, 0.8660254037844387076, 1.000000000000000000, 0.8660254037844387076, 1.000000000000000000, 0.8660254037844387076, 1.000000000000000000, 0.8660254037844387076, 1.000000000000000000, 0.8660254037844387076, 1.000000000000000000, 0.8660254037844387076, 1.000000000000000000, 0.8660254037844387076, 1.000000000000000000, 0.8660254037844387076, 1.000000000000000000, 0.8660254037844387076, 1.000000000000000000, 0.8660254037844387076, 1.000000000000000000, 0.8660254037844387076, 1.000000000000000000, 0.8660254037844387076, 1.000000000000000000, 0.8660254037844387076, 1.000000000000000000, 0.8660254037844387076, 1.000000000000000000, 0.8660254037844387076, 1.000000000000000000, 0.8660254037844387076, 1.000000000000000000, 0.8660254037844387076, 1.000000000000000000, 0.8660254037844387076, 1.000000000000000000, 0.8660254037844387076, 1.000000000000000000, 0.8660254037844387076, 1.000000000000000000, 0.8660254037844387076, 1.000000000000000000, 0.8660254037844387076, 1.000000000000000000, 0.8660254037844387076, 1.000000000000000000, 0.8660254037844387076, 1.000000000000000000, 0.8660254037844387076, 1.000000000000000000, 0.8660254037844387076, 1.000000000000000000, 0.8660254037844387076, 1.000000000000000000, 0.8660254037844387076, 1.000000000000000000, 0.8660254037844387076, 1.000000000000000000, 0.8660254037844387076, 1.000000000000000000, 0.8660254037844387076, 1.000000000000000000, 0.8660254037844387076, 1.000000000000000000, 0.8660254037844387076, 1.000000000000000000, 0.8660254037844387076, 1.000000000000000000, 0.8660254037844387076, 1.000000000000000000, 0.8660254037844387076, 1.000000000000000000, 0.8660254037844387076, 1.000000000000000000, 0.8660254037844387076, 1.000000000000000000, 0.8660254037844387076, 1.000000000000000000, 0.8660254037844387076, 1.000000000000000000, 0.8660254037844387076, 1.000000000000000000, 0.8660254037844387076, 1.000000000000000000, 0.8660254037844387076, 1.000000000000000000, 0.8660254037844387076, 1.000000000000000000, 0.8660254037844387076, 1.000000000000000000, 0.8660254037844387076, 1.000000000000000000, 0.8660254037844387076, 1.000000000000000000, 0.8660254037844387076, 1.000000000000000000, 0.8660254037844387076, 1.000000000000000000, 0.8660254037844387076, 1.000000000000000000, 0.8660254037844387076, 1.000000000000000000, 0.8660254037844387076, 1.000000000000000000, 0.8660254037844387076, 1.000000000000000000, 0.8660254037844387076, 1.000000000000000000, 0.8660254037844387076, 1.000000000000000000, 0.8660254037844387076, 1.000000000000000000, 0.8660254037844387076, 1.000000000000000000, 0.8660254037844387076, 1.000000000000000000, 0.8660254037844387076, 1.000000000000000000, 0.8660254037844387076, 1.000000000000000000),
 ( 1.000000000000000000, 0.8660254037844387076, 1.000000000000000000, 0.8660254037844387076, 1.000000000000000000, 0.8660254037844387076, 1.000000000000000000, 0.8660254037844387076, 1.000000000000000000, 0.8660254037844387076, 1.000000000000000000, 0.8660254037844387076, 1.000000000000000000, 0.8660254037844387076, 1.000000000000000000, 0.8660254037844387076, 1.000000000000000000, 0.8660254037844387076, 1.000000000000000000, 0.8660254037844387076, 1.000000000000000000, 0.8660254037844387076, 1.000000000000000000, 0.8660254037844387076, 1.000000000000000000, 0.8660254037844387076, 1.000000000000000000, 0.8660254037844387076, 1.000000000000000000, 0.8660254037844387076, 1.000000000000000000, 0.8660254037844387076, 1.000000000000000000, 0.8660254037844387076, 1.000000000000000000, 0.8660254037844387076, 1.000000000000000000, 0.8660254037844387076, 1.000000000000000000, 0.8660254037844387076, 1.000000000000000000, 0.8660254037844387076, 1.000000000000000000, 0.8660254037844387076, 1.000000000000000000, 0.8660254037844387076, 1.000000000000000000, 0.8660254037844387076, 1.000000000000000000, 0.8660254037844387076, 1.000000000000000000, 0.8660254037844387076, 1.000000000000000000, 0.8660254037844387076, 1.000000000000000000, 0.8660254037844387076, 1.000000000000000000, 0.8660254037844387076, 1.000000000000000000, 0.8660254037844387076, 1.000000000000000000, 0.8660254037844387076, 1.000000000000000000, 0.8660254037844387076, 1.000000000000000000, 0.8660254037844387076, 1.000000000000000000, 0.8660254037844387076, 1.000000000000000000, 0.8660254037844387076, 1.000000000000000000, 0.8660254037844387076, 1.000000000000000000, 0.8660254037844387076, 1.000000000000000000, 0.8660254037844387076, 1.000000000000000000, 0.8660254037844387076, 1.000000000000000000, 0.8660254037844387076, 1.000000000000000000, 0.8660254037844387076, 1.000000000000000000, 0.8660254037844387076, 1.000000000000000000, 0.8660254037844387076, 1.000000000000000000, 0.8660254037844387076, 1.000000000000000000, 0.8660254037844387076, 1.000000000000000000, 0.8660254037844387076, 1.000000000000000000, 0.8660254037844387076, 1.000000000000000000, 0.8660254037844387076, 1.000000000000000000, 0.8660254037844387076, 1.000000000000000000, 0.8660254037844387076, 1.000000000000000000, 0.8660254037844387076, 1.000000000000000000, 0.8660254037844387076, 1.000000000000000000, 0.8660254037844387076, 1.000000000000000000, 0.8660254037844387076, 1.000000000000000000, 0.8660254037844387076, 1.000000000000000000, 0.8660254037844387076, 1.000000000000000000, 0.8660254037844387076, 1.000000000000000000, 0.8660254037844387076, 1.000000000000000000, 0.8660254037844387076, 1.000000000000000000, 0.8660254037844387076, 1.000000000000000000, 0.8660254037844387076, 1.000000000000000000, 0.8660254037844387076, 1.000000000000000000, 0.8660254037844387076, 1.000000000000000000, 0.8660254037844387076, 1.000000000000000000, 0.8660254037844387076, 1.000000000000000000, 0.8660254037844387076, 1.000000000000000000, 0.8660254037844387076, 1.000000000000000000, 0.8660254037844387076, 1.000000000000000000, 0.8660254037844387076, 1.000000000000000000, 0.8660254037844387076, 1.000000000000000000, 0.8660254037844387076, 1.000000000000000000, 0.8660254037844387076, 1.000000000000000000, 0.8660254037844387076, 1.000000000000000000, 0.8660254037844387076, 1.000000000000000000, 0.8660254037844387076, 1.000000000000000000, 0.8660254037844387076, 1.000000000000000000, 0.8660254037844387076, 1.000000000000000000, 0.8660254037844387076, 1.000000000000000000, 0.8660254037844387076, 1.000000000000000000, 0.8660254037844387076, 1.000000000000000000, 0.8660254037844387076, 1.000000000000000000, 0.8660254037844387076, 1.000000000000000000, 0.8660254037844387076, 1.000000000000000000, 0.8660254037844387076, 1.000000000000000000, 0.8660254037844387076, 1.000000000000000000, 0.8660254037844387076, 1.000000000000000000, 0.8660254037844387076, 1.000000000000000000, 0.8660254037844387076, 1.000000000000000000, 0.8660254037844387076, 1.000000000000000000, 0.8660254037844387076, 1.000000000000000000, 0.8660254037844387076, 1.000000000000000000, 0.8660254037844387076, 1.000000000000000000, 0.8660254037844387076, 1.000000000000000000, 0.8660254037844387076, 1.000000000000000000, 0.8660254037844387076, 1.000000000000000000, 0.8660254037844387076, 1.000000000000000000, 0.8660254037844387076, 1.000000000000000000, 0.8660254037844387076, 1.000000000000000000, 0.8660254037844387076, 1.000000000000000000, 0.8660254037844387076, 1.000000000000000000, 0.8660254037844387076, 1.000000000000000000, 0.8660254037844387076, 1.000000000000000000, 0.8660254037844387076, 1.000000000000000000, 0.8660254037844387076, 1.000000000000000000, 0.8660254037844387076, 1.000000000000000000, 0.8660254037844387076, 1.000000000000000000, 0.8660254037844387076, 1.000000000000000000, 0.8660254037844387076, 1.000000000000000000, 0.8660254037844387076, 1.000000000000000000, 0.8660254037844387076, 1.000000000000000000, 0.8660254037844387076, 1.000000000000000000, 0.8660254037844387076, 1.000000000000000000, 0.8660254037844387076, 1.000000000000000000, 0.8660254037844387076, 1.000000000000000000, 0.8660254037844387076, 1.000000000000000000, 0.8660254037844387076, 1.000000000000000000, 0.8660254037844387076, 1.000000000000000000, 0.8660254037844387076, 1.000000000000000000, 0.8660254037844387076, 1.000000000000000000, 0.8660254037844387076, 1.000000000000000000, 0.8660254037844387076, 1.000000000000000000, 0.8660254037844387076, 1.000000000000000000, 0.8660254037844387076, 1.000000000000000000, 0.8660254037844387076, 1.000000000000000000, 0.8660254037844387076, 1.000000000000000000, 0.8660254037844387076, 1.000000000000000000, 0.8660254037844387076, 1.000000000000000000, 0.8660254037844387076, 1.000000000000000000, 0.8660254037844387076, 1.000000000000000000, 0.8660254037844387076, 1.000000000000000000, 0.8660254037844387076, 1.000000000000000000, 0.8660254037844387076, 1.000000000000000000, 0.8660254037844387076, 1.000000000000000000, 0.8660254037844387076, 1.000000000000000000, 0.8660254037844387076, 1.000000000000000000, 0.8660254037844387076, 1.000000000000000000, 0.8660254037844387076, 1.000000000000000000, 0.8660254037844387076, 1.000000000000000000, 0.8660254037844387076, 1.000000000000000000, 0.8660254037844387076, 1.000000000000000000, 0.8660254037844387076, 1.000000000000000000, 0.8660254037844387076, 1.000000000000000000, 0.8660254037844387076, 1.000000000000000000, 0.8660254037844387076, 1.000000000000000000, 0.8660254037844387076, 1.000000000000000000, 0.8660254037844387076, 1.000000000000000000, 0.8660254037844387076, 1.000000000000000000, 0.8660254037844387076, 1.000000000000000000, 0.8660254037844387076, 1.000000000000000000, 0.8660254037844387076, 1.000000000000000000, 0.8660254037844387076, 1.000000000000000000, 0.8660254037844387076, 1.000000000000000000, 0.8660254037844387076, 1.000000000000000000, 0.8660254037844387076, 1.000000000000000000, 0.8660254037844387076, 1.000000000000000000, 0.8660254037844387076, 1.000000000000000000, 0.8660254037844387076, 1.000000000000000000, 0.8660254037844387076, 1.000000000000000000, 0.8660254037844387076, 1.000000000000000000, 0.8660254037844387076, 1.000000000000000000, 0.8660254037844387076, 1.000000000000000000, 0.8660254037844387076, 1.000000000000000000, 0.8660254037844387076, 1.000000000000000000, 0.8660254037844387076, 1.000000000000000000, 0.8660254037844387076, 1.000000000000000000, 0.8660254037844387076, 1.000000000000000000, 0.8660254037844387076, 1.000000000000000000, 0.8660254037844387076, 1.000000000000000000, 0.8660254037844387076, 1.000000000000000000, 0.8660254037844387076, 1.000000000000000000, 0.8660254037844387076, 1.000000000000000000, 0.8660254037844387076, 1.000000000000000000, 0.8660254037844387076, 1.000000000000000000, 0.8660254037844387076, 1.000000000000000000, 0.8660254037844387076, 1.000000000000000000, 0.8660254037844387076, 1.000000000000000000, 0.8660254037844387076, 1.000000000000000000, 0.8660254037844387076, 1.000000000000000000, 0.8660254037844387076, 1.000000000000000000, 0.8660254037844387076, 1.000000000000000000, 0.8660254037844387076, 1.000000000000000000, 0.8660254037844387076, 1.000000000000000000, 0.8660254037844387076, 1.000000000000000000, 0.8660254037844387076, 1.000000000000000000, 0.8660254037844387076, 1.000000000000000000, 0.8660254037844387076, 1.000000000000000000, 0.8660254037844387076, 1.000000000000000000, 0.8660254037844387076, 1.000000000000000000, 0.8660254037844387076, 1.000000000000000000, 0.8660254037844387076, 1.000000000000000000, 0.8660254037844387076, 1.000000000000000000, 0.8660254037844387076, 1.000000000000000000, 0.8660254037844387076, 1.000000000000000000, 0.8660254037844387076, 1.000000000000000000, 0.8660254037844387076, 1.000000000000000000, 0.8660254037844387076, 1.000000000000000000, 0.8660254037844387076, 1.000000000000000000, 0.8660254037844387076, 1.000000000000000000, 0.8660254037844387076, 1.000000000000000000, 0.8660254037844387076, 1.000000000000000000, 0.8660254037844387076, 1.000000000000000000, 0.8660254037844387076, 1.000000000000000000, 0.8660254037844387076, 1.000000000000000000, 0.8660254037844387076, 1.000000000000000000, 0.8660254037844387076, 1.000000000000000000, 0.8660254037844387076, 1.000000000000000000, 0.8660254037844387076, 1.000000000000000000, 0.8660254037844387076, 1.000000000000000000, 0.8660254037844387076, 1.000000000000000000, 0.8660254037844387076, 1.000000000000000000, 0.8660254037844387076, 1.000000000000000000, 0.8660254037844387076, 1.000000000000000000, 0.8660254037844387076, 1.000000000000000000, 0.8660254037844387076, 1.000000000000000000, 0.8660254037844387076, 1.000000000000000000, 0.8660254037844387076, 1.000000000000000000, 0.8660254037844387076, 1.000000000000000000, 0.8660254037844387076, 1.000000000000000000, 0.8660254037844387076, 1.000000000000000000, 0.8660254037844387076, 1.000000000000000000, 0.8660254037844387076, 1.000000000000000000, 0.8660254037844387076, 1.000000000000000000, 0.8660254037844387076, 1.000000000000000000, 0.8660254037844387076, 1.000000000000000000, 0.8660254037844387076, 1.000000000000000000, 0.8660254037844387076, 1.000000000000000000, 0.8660254037844387076, 1.000000000000000000, 0.8660254037844387076, 1.000000000000000000, 0.8660254037844387076, 1.000000000000000000, 0.8660254037844387076, 1.000000000000000000, 0.8660254037844387076, 1.000000000000000000, 0.8660254037844387076, 1.000000000000000000, 0.8660254037844387076, 1.000000000000000000, 0.8660254037844387076, 1.000000000000000000, 0.8660254037844387076, 1.000000000000000000, 0.8660254037844387076, 1.000000000000000000, 0.8660254037844387076, 1.000000000000000000, 0.8660254037844387076, 1.000000000000000000, 0.8660254037844387076, 1.000000000000000000, 0.8660254037844387076, 1.000000000000000000, 0.8660254037844387076, 1.000000000000000000, 0.8660254037844387076, 1.000000000000000000, 0.8660254037844387076, 1.000000000000000000, 0.8660254037844387076, 1.000000000000000000, 0.8660254037844387076, 1.000000000000000000, 0.8660254037844387076, 1.000000000000000000, 0.8660254037844387076, 1.000000000000000000, 0.8660254037844387076, 1.000000000000000000, 0.8660254037844387076, 1.000000000000000000, 0.8660254037844387076, 1.000000000000000000, 0.8660254037844387076, 1.000000000000000000, 0.8660254037844387076, 1.000000000000000000, 0.8660254037844387076, 1.000000000000000000, 0.8660254037844387076, 1.000000000000000000, 0.8660254037844387076, 1.000000000000000000, 0.8660254037844387076, 1.000000000000000000, 0.8660254037844387076, 1.000000000000000000, 0.8660254037844387076, 1.000000000000000000, 0.8660254037844387076, 1.000000000000000000, 0.8660254037844387076, 1.000000000000000000, 0.8660254037844387076, 1.000000000000000000, 0.8660254037844387076, 1.000000000000000000, 0.8660254037844387076, 1.000000000000000000, 0.8660254037844387076, 1.000000000000000000, 0.8660254037844387076, 1.000000000000000000, 0.8660254037844387076, 1.000000000000000000, 0.8660254037844387076, 1.000000000000000000, 0.8660254037844387076, 1.000000000000000000, 0.8660254037844387076, 1.000000000000000000, 0.8660254037844387076, 1.000000000000000000, 0.8660254037844387076, 1.000000000000000000, 0.8660254037844387076, 1.000000000000000000, 0.8660254037844387076, 1.000000000000000000, 0.8660254037844387076, 1.000000000000000000, 0.8660254037844387076, 1.000000000000000000, 0.8660254037844387076, 1.000000000000000000, 0.8660254037844387076, 1.000000000000000000, 0.8660254037844387076, 1.000000000000000000, 0.8660254037844387076, 1.000000000000000000, 0.8660254037844387076, 1.000000000000000000, 0.8660254037844387076, 1.000000000000000000, 0.8660254037844387076, 1.000000000000000000, 0.8660254037844387076, 1.000000000000000000, 0.8660254037844387076, 1.000000000000000000, 0.8660254037844387076, 1.000000000000000000, 0.8660254037844387076, 1.000000000000000000, 0.8660254037844387076, 1.000000000000000000, 0.8660254037844387076, 1.000000000000000000, 0.8660254037844387076, 1.000000000000000000, 0.8660254037844387076, 1.000000000000000000, 0.8660254037844387076, 1.000000000000000000, 0.8660254037844387076, 1.000000000000000000, 0.8660254037844387076, 1.000000000000000000, 0.8660254037844387076, 1.000000000000000000, 0.8660254037844387076, 1.000000000000000000, 0.8660254037844387076, 1.000000000000000000, 0.8660254037844387076, 1.000000000000000000, 0.8660254037844387076, 1.000000000000000000, 0.8660254037844387076, 1.000000000000000000, 0.8660254037844387076, 1.000000000000000000, 0.8660254037844387076, 1.000000000000000000, 0.8660254037844387076, 1.000000000000000000, 0.8660254037844387076, 1.000000000000000000, 0.8660254037844387076, 1.000000000000000000, 0.8660254037844387076, 1.000000000000000000, 0.8660254037844387076, 1.000000000000000000, 0.8660254037844387076, 1.000000000000000000, 0.8660254037844387076, 1.000000000000000000, 0.8660254037844387076, 1.000000000000000000, 0.8660254037844387076, 1.000000000000000000, 0.8660254037844387076, 1.000000000000000000, 0.8660254037844387076, 1.000000000000000000, 0.8660254037844387076, 1.000000000000000000, 0.8660254037844387076, 1.000000000000000000, 0.8660254037844387076, 1.000000000000000000, 0.8660254037844387076, 1.000000000000000000, 0.8660254037844387076, 1.000000000000000000, 0.8660254037844387076, 1.000000000000000000, 0.8660254037844387076, 1.000000000000000000, 0.8660254037844387076, 1.000000000000000000, 0.8660254037844387076, 1.000000000000000000, 0.8660254037844387076, 1.000000000000000000, 0.8660254037844387076, 1.000000000000000000, 0.8660254037844387076, 1.000000000000000000, 0.8660254037844387076, 1.000000000000000000, 0.8660254037844387076, 1.000000000000000000, 0.8660254037844387076, 1.000000000000000000, 0.8660254037844387076, 1.000000000000000000, 0.8660254037844387076, 1.000000000000000000, 0.8660254037844387076, 1.000000000000000000, 0.8660254037844387076, 1.000000000000000000, 0.8660254037844387076, 1.000000000000000000, 0.8660254037844387076, 1.000000000000000000, 0.8660254037844387076, 1.000000000000000000, 0.8660254037844387076, 1.000000000000000000, 0.8660254037844387076, 1.000000000000000000, 0.8660254037844387076, 1.000000000000000000, 0.8660254037844387076, 1.000000000000000000, 0.8660254037844387076, 1.000000000000000000, 0.8660254037844387076, 1.000000000000000000, 0.8660254037844387076, 1.000000000000000000, 0.8660254037844387076, 1.000000000000000000, 0.8660254037844387076, 1.000000000000000000, 0.8660254037844387076, 1.000000000000000000, 0.8660254037844387076, 1.000000000000000000, 0.8660254037844387076, 1.000000000000000000, 0.8660254037844387076, 1.000000000000000000, 0.8660254037844387076, 1.000000000000000000, 0.8660254037844387076, 1.000000000000000000, 0.8660254037844387076, 1.000000000000000000, 0.8660254037844387076, 1.000000000000000000, 0.8660254037844387076, 1.000000000000000000, 0.8660254037844387076, 1.000000000000000000, 0.8660254037844387076, 1.000000000000000000, 0.8660254037844387076, 1.000000000000000000, 0.8660254037844387076, 1.000000000000000000, 0.8660254037844387076, 1.000000000000000000, 0.8660254037844387076, 1.000000000000000000, 0.8660254037844387076, 1.000000000000000000, 0.8660254037844387076, 1.000000000000000000) ) ) 
 REPRESENTATION_ITEM ( '' )  SURFACE ( )  );
#43418 = EDGE_CURVE ( 'NONE', #16810, #32393, #2888, .T. ) ;
#43419 = CARTESIAN_POINT ( 'NONE',  ( 19.87500000000000000, 6.123233995736764310E-16, -4.999999999999998224 ) ) ;
#43420 = CARTESIAN_POINT ( 'NONE',  ( 19.19062500061452070, -3.027376345333610441, -5.243569643749999898 ) ) ;
#43421 = CARTESIAN_POINT ( 'NONE',  ( 24.19687500061451857, -3.027376345333610441, -5.243569643749999898 ) ) ;
#43422 = CARTESIAN_POINT ( 'NONE',  ( -3.756430356250000102, 18.82812499938548356, 30.00000000000000000 ) ) ;
#43423 = DIRECTION ( 'NONE',  ( -0.000000000000000000, -1.000000000000000000, -0.000000000000000000 ) ) ;
#43424 = CARTESIAN_POINT ( 'NONE',  ( 27.79687500061451999, -3.027376345333610441, -5.243569643749999898 ) ) ;
#43425 = CARTESIAN_POINT ( 'NONE',  ( 5.484375000614518214, 4.541064518000418104, 2.621784821874999949 ) ) ;
#43426 = CARTESIAN_POINT ( 'NONE',  ( 14.69062500061451537, -3.027376345333610441, -5.243569643749999898 ) ) ;
#43427 = CARTESIAN_POINT ( 'NONE',  ( 12.57187500061451857, 3.027376345333613106, -5.243569643749998122 ) ) ;
#43428 = ORIENTED_EDGE ( 'NONE', *, *, #55179, .T. ) ;
#43429 = CYLINDRICAL_SURFACE ( 'NONE', #33675, 4.999999999999998224 ) ;
#43430 = CARTESIAN_POINT ( 'NONE',  ( 25.75312500061451715, 0.000000000000000000, 5.243569643749999010 ) ) ;
#43431 = CARTESIAN_POINT ( 'NONE',  ( 3.474966266584414321, 3.595135176884375117, -3.675031694903898138 ) ) ;
#43432 = CARTESIAN_POINT ( 'NONE',  ( 14.69999999999999929, 0.000000000000000000, 4.999999999999998224 ) ) ;
#43433 = CARTESIAN_POINT ( 'NONE',  ( 14.06250000000000000, 2.886751345948129099, -4.999999999999998224 ) ) ;
#43434 = CARTESIAN_POINT ( 'NONE',  ( 23.28750000122903430, 4.330127018922191873, 2.499999999999999556 ) ) ;
#43435 = CARTESIAN_POINT ( 'NONE',  ( 18.55312500061451431, 0.000000000000000000, 5.243569643749999010 ) ) ;
#43436 = ORIENTED_EDGE ( 'NONE', *, *, #23020, .F. ) ;
#43437 = CARTESIAN_POINT ( 'NONE',  ( 22.16250000000000142, 2.886751345948129099, -4.999999999999998224 ) ) ;
#43438 = CARTESIAN_POINT ( 'NONE',  ( 24.57187500061451502, -6.054752690667223547, -1.112240025338166033E-15 ) ) ;
#43439 = ORIENTED_EDGE ( 'NONE', *, *, #72495, .F. ) ;
#43440 = CARTESIAN_POINT ( 'NONE',  ( 20.10000000000000142, 0.000000000000000000, 4.999999999999998224 ) ) ;
#43441 = CARTESIAN_POINT ( 'NONE',  ( 11.76562500061451644, 3.027376345333611329, 5.243569643749999010 ) ) ;
#43442 = CARTESIAN_POINT ( 'NONE',  ( 3.290625000614516793, -3.027376345333614438, 5.243569643749998122 ) ) ;
#43443 = CARTESIAN_POINT ( 'NONE',  ( 13.17187500061451466, -4.119189519843968306, 2.378215178124996054 ) ) ;
#43444 = CARTESIAN_POINT ( 'NONE',  ( 26.31562500061451715, -6.054752690667223547, -1.112240025338166033E-15 ) ) ;
#43445 = CARTESIAN_POINT ( 'NONE',  ( 16.72500000000000142, 6.123233995736764310E-16, -4.999999999999998224 ) ) ;
#43446 = CARTESIAN_POINT ( 'NONE',  ( 25.01249999999999929, 2.886751345948126879, 4.999999999999999112 ) ) ;
#43447 = CARTESIAN_POINT ( 'NONE',  ( -4.243569643749999898, 19.35312500061451857, 30.00000000000000000 ) ) ;
#43448 = CARTESIAN_POINT ( 'NONE',  ( 7.096875000614517148, -3.027376345333610441, -5.243569643749999898 ) ) ;
#43449 = CARTESIAN_POINT ( 'NONE',  ( 16.69687500061451502, 6.054752690667223547, 3.707466751127219781E-16 ) ) ;
#43450 = CARTESIAN_POINT ( 'NONE',  ( 28.95937500061451431, 0.000000000000000000, 5.243569643749999010 ) ) ;
#43451 = ORIENTED_EDGE ( 'NONE', *, *, #25255, .T. ) ;
#43452 = CARTESIAN_POINT ( 'NONE',  ( 27.17812500061451786, -4.541064518000419881, 2.621784821874995952 ) ) ;
#43453 = CARTESIAN_POINT ( 'NONE',  ( 26.82187500061451857, -6.054752690667223547, -1.112240025338166033E-15 ) ) ;
#43454 = CARTESIAN_POINT ( 'NONE',  ( 20.78732959644809952, -2.499999999999999556, 3.499999999999999556 ) ) ;
#43455 = CARTESIAN_POINT ( 'NONE',  ( 13.76250000000000107, 2.886751345948126879, 4.999999999999999112 ) ) ;
#43456 = CARTESIAN_POINT ( 'NONE',  ( 12.29062500061451857, -3.027376345333614438, 5.243569643749998122 ) ) ;
#43457 = CARTESIAN_POINT ( 'NONE',  ( -2.000000000000001776, 19.54999999999999716, 33.46410161513775705 ) ) ;
#43458 = CARTESIAN_POINT ( 'NONE',  ( 29.65312500061451573, 4.541064518000418104, -2.621784821874998173 ) ) ;
#43459 = CARTESIAN_POINT ( 'NONE',  ( 17.13750000122903216, -4.330127018922194537, 2.499999999999995559 ) ) ;
#43460 = CARTESIAN_POINT ( 'NONE',  ( 14.67187500061451821, -5.492252693125287522, -1.008910452111647106E-15 ) ) ;
#43461 = CARTESIAN_POINT ( 'NONE',  ( 5.353125000614515905, 4.541064518000418104, -2.621784821874998173 ) ) ;
#43462 = CARTESIAN_POINT ( 'NONE',  ( 20.78437500061451715, 4.541064518000418104, 2.621784821874999949 ) ) ;
#43463 = CARTESIAN_POINT ( 'NONE',  ( -4.243569643749999898, 17.12187500061451573, 27.54997392385601529 ) ) ;
#43464 = CARTESIAN_POINT ( 'NONE',  ( 20.70937500061451786, 4.541064518000418104, -2.621784821874998173 ) ) ;
#43465 = CARTESIAN_POINT ( 'NONE',  ( 5.625000000000001776, 4.330127018922191873, 2.499999999999999556 ) ) ;
#43466 = CARTESIAN_POINT ( 'NONE',  ( -3.999999999999999112, 9.762500001229033941, 30.00000000000000000 ) ) ;
#43467 = CARTESIAN_POINT ( 'NONE',  ( 12.59062500061451573, 6.054752690667223547, 3.707466751127219781E-16 ) ) ;
#43468 = CARTESIAN_POINT ( 'NONE',  ( 4.237500001229036251, 6.123233995736764310E-16, -4.999999999999998224 ) ) ;
#43469 = CARTESIAN_POINT ( 'NONE',  ( 8.896875000614517859, -3.027376345333610441, -5.243569643749999898 ) ) ;
#43470 = CARTESIAN_POINT ( 'NONE',  ( -5.000000000000000000, 39.99999999999999289, 30.00000000000000000 ) ) ;
#43471 = CARTESIAN_POINT ( 'NONE',  ( 9.215625000614515727, -6.054752690667223547, -1.112240025338166033E-15 ) ) ;
#43472 = CARTESIAN_POINT ( 'NONE',  ( 15.49687500061451750, -3.027376345333614438, 5.243569643749998122 ) ) ;
#43473 = CARTESIAN_POINT ( 'NONE',  ( 3.464268450295128865, -3.605406963609541382, -3.807383367585859268 ) ) ;
#43474 = CARTESIAN_POINT ( 'NONE',  ( 21.22500000122903074, -5.773502691896255534, -1.060575238724906372E-15 ) ) ;
#43475 = CARTESIAN_POINT ( 'NONE',  ( 9.684375000614517504, -4.541064518000419881, 2.621784821874995952 ) ) ;
#43476 = CARTESIAN_POINT ( 'NONE',  ( 11.35312500061451679, 0.000000000000000000, 5.243569643749999010 ) ) ;
#43477 = CARTESIAN_POINT ( 'NONE',  ( 26.30625000122903145, 4.330127018922192761, -2.499999999999997780 ) ) ;
#43478 = CARTESIAN_POINT ( 'NONE',  ( 22.13437500061451502, 4.541064518000418104, 2.621784821874999949 ) ) ;
#43479 = FACE_OUTER_BOUND ( 'NONE', #14761, .T. ) ;
#43480 =( BOUNDED_CURVE ( )  B_SPLINE_CURVE ( 2, ( #39498, #44324, #67579, #66854, #72751, #33578, #11051 ),
 .UNSPECIFIED., .F., .F. ) 
 B_SPLINE_CURVE_WITH_KNOTS ( ( 3, 2, 2, 3 ),
 ( 0.5600000000000000533, 0.5633333333333333526, 0.5666666666666667629, 0.5700000000000000622 ),
 .UNSPECIFIED. ) 
 CURVE ( )  GEOMETRIC_REPRESENTATION_ITEM ( )  RATIONAL_B_SPLINE_CURVE ( ( 1.000000000000000000, 0.8660254037844387076, 1.000000000000000000, 0.8660254037844387076, 1.000000000000000000, 0.8660254037844342667, 1.000000000000004441 ) ) 
 REPRESENTATION_ITEM ( '' )  );
#43481 = CARTESIAN_POINT ( 'NONE',  ( -3.858979783667864982, 3.180598473748191157, 31.08663701263182233 ) ) ;
#43482 = DIRECTION ( 'NONE',  ( -0.000000000000000000, -1.000000000000000000, -0.000000000000000000 ) ) ;
#43483 = CARTESIAN_POINT ( 'NONE',  ( 2.121784821875001281, 11.90937500061451892, -26.32496088578401938 ) ) ;
#43484 = CARTESIAN_POINT ( 'NONE',  ( 15.82500000122903216, -5.773502691896255534, -1.060575238724906372E-15 ) ) ;
#43485 = CARTESIAN_POINT ( 'NONE',  ( 9.001249775931846008E-16, 17.21562500061451928, -25.09994784771203058 ) ) ;
#43486 = CARTESIAN_POINT ( 'NONE',  ( 17.25000000122903288, -2.886751345948125991, -5.000000000000000000 ) ) ;
#43487 = CARTESIAN_POINT ( 'NONE',  ( 9.290625000614515017, -3.027376345333610441, -5.243569643749999898 ) ) ;
#43488 = ORIENTED_EDGE ( 'NONE', *, *, #47179, .T. ) ;
#43489 = CARTESIAN_POINT ( 'NONE',  ( 16.23750000000000071, -2.886751345948125991, -5.000000000000000000 ) ) ;
#43490 = CARTESIAN_POINT ( 'NONE',  ( 5.100000001229031632, -2.886751345948193048, -4.999999999999883649 ) ) ;
#43491 = CARTESIAN_POINT ( 'NONE',  ( 10.43437500061451750, 4.541064518000418104, 2.621784821874999949 ) ) ;
#43492 = CARTESIAN_POINT ( 'NONE',  ( -3.137519842735245283E-14, 14.37500000122903288, 34.00000000000000000 ) ) ;
#43493 = CARTESIAN_POINT ( 'NONE',  ( 9.825000001229033941, 2.886751345948126879, 4.999999999999999112 ) ) ;
#43494 = CARTESIAN_POINT ( 'NONE',  ( 19.38750000122903216, -4.330127018922194537, 2.499999999999995559 ) ) ;
#43495 = CARTESIAN_POINT ( 'NONE',  ( 15.66562500061451857, 3.027376345333613106, -5.243569643749998122 ) ) ;
#43496 = CARTESIAN_POINT ( 'NONE',  ( 19.15312500061451573, -4.541064518000417216, -2.621784821875001281 ) ) ;
#43497 = CARTESIAN_POINT ( 'NONE',  ( 28.57500000122903572, 2.886751345948129099, -4.999999999999998224 ) ) ;
#43498 =( BOUNDED_CURVE ( )  B_SPLINE_CURVE ( 2, ( #51825, #1228, #29650, #17819, #41467, #23734, #18548 ),
 .UNSPECIFIED., .F., .F. ) 
 B_SPLINE_CURVE_WITH_KNOTS ( ( 3, 2, 2, 3 ),
 ( 0.06000000000000003941, 0.06333333333333336645, 0.06666666666666667962, 0.07000000000000000666 ),
 .UNSPECIFIED. ) 
 CURVE ( )  GEOMETRIC_REPRESENTATION_ITEM ( )  RATIONAL_B_SPLINE_CURVE ( ( 0.9999999999999983347, 0.8660254037844403729, 1.000000000000000000, 0.8660254037844387076, 1.000000000000000000, 0.8660254037844387076, 1.000000000000000000 ) ) 
 REPRESENTATION_ITEM ( '' )  );
#43499 = EDGE_CURVE ( 'NONE', #22787, #45851, #10448, .T. ) ;
#43500 = CARTESIAN_POINT ( 'NONE',  ( 29.47500000122903430, 2.886751345948129099, -4.999999999999998224 ) ) ;
#43501 = CARTESIAN_POINT ( 'NONE',  ( 24.67500000000000071, -4.330127018922194537, 2.499999999999995559 ) ) ;
#43502 = CARTESIAN_POINT ( 'NONE',  ( 3.756430356250000546, 13.12812499938548250, 27.83122392262697886 ) ) ;
#43503 = CARTESIAN_POINT ( 'NONE',  ( 26.63437500061451857, 4.541064518000418104, 2.621784821874999949 ) ) ;
#43504 = CARTESIAN_POINT ( 'NONE',  ( -3.999999999999999112, 15.91249999999999964, 27.69059892324149885 ) ) ;
#43505 = CARTESIAN_POINT ( 'NONE',  ( 13.46250000122903323, 0.000000000000000000, 4.999999999999998224 ) ) ;
#43506 = CARTESIAN_POINT ( 'NONE',  ( 3.675000000000001155, 6.123233995736764310E-16, -4.999999999999998224 ) ) ;
#43507 = EDGE_CURVE ( 'NONE', #68862, #51352, #63944, .T. ) ;
#43508 = PLANE ( 'NONE',  #6607 ) ;
#43509 = CARTESIAN_POINT ( 'NONE',  ( 7.021875000614518747, -6.054752690667223547, -1.112240025338166033E-15 ) ) ;
#43510 = CARTESIAN_POINT ( 'NONE',  ( 27.06562500061451004, 3.027376345333611329, 5.243569643749999010 ) ) ;
#43511 =( BOUNDED_CURVE ( )  B_SPLINE_CURVE ( 2, ( #47550, #52366, #70079, #30197, #24284, #18727, #12835 ),
 .UNSPECIFIED., .F., .F. ) 
 B_SPLINE_CURVE_WITH_KNOTS ( ( 3, 2, 2, 3 ),
 ( 0.9500000000000000666, 0.9533333333333334769, 0.9566666666666666652, 0.9599999999999999645 ),
 .UNSPECIFIED. ) 
 CURVE ( )  GEOMETRIC_REPRESENTATION_ITEM ( )  RATIONAL_B_SPLINE_CURVE ( ( 0.9999999999999955591, 0.8660254037844431485, 1.000000000000000000, 0.8660254037844387076, 1.000000000000000000, 0.8660254037844387076, 1.000000000000000000 ) ) 
 REPRESENTATION_ITEM ( '' )  );
#43512 = CARTESIAN_POINT ( 'NONE',  ( 0.000000000000000000, 20.00000000000000000, -33.99999999999999289 ) ) ;
#43513 = DIRECTION ( 'NONE',  ( -1.000000000000000000, -0.000000000000000000, -0.000000000000000000 ) ) ;
#43514 = CARTESIAN_POINT ( 'NONE',  ( 3.693371437524641365, -3.370391871118413540, 3.876951387445791930 ) ) ;
#43515 = CARTESIAN_POINT ( 'NONE',  ( 4.921875000614518214, 3.027376345333613106, -5.243569643749998122 ) ) ;
#43516 = CARTESIAN_POINT ( 'NONE',  ( 8.559375000614515727, 4.541064518000418104, -2.621784821874998173 ) ) ;
#43517 = CARTESIAN_POINT ( 'NONE',  ( 28.20937500061451786, -4.541064518000417216, -2.621784821875001281 ) ) ;
#43518 = CARTESIAN_POINT ( 'NONE',  ( -4.243569643749999898, 13.01562500061459637, 27.54997392385601529 ) ) ;
#43519 = CARTESIAN_POINT ( 'NONE',  ( 21.93750000000000000, -2.886751345948129988, 4.999999999999997335 ) ) ;
#43521 = ADVANCED_FACE ( 'NONE', ( #23335 ), #13329, .F. ) ;
#43520 = CARTESIAN_POINT ( 'NONE',  ( 20.81250000122903643, -4.330127018922190985, -2.500000000000001332 ) ) ;
#43522 = CARTESIAN_POINT ( 'NONE',  ( 4.575000000000002842, 6.123233995736764310E-16, -4.999999999999998224 ) ) ;
#43523 = EDGE_LOOP ( 'NONE', ( #13796, #18684, #68509, #41874 ) ) ;
#43524 = CARTESIAN_POINT ( 'NONE',  ( 18.96562500061451573, 3.027376345333611329, 5.243569643749999010 ) ) ;
#43525 = CARTESIAN_POINT ( 'NONE',  ( 10.49062500061451431, -3.027376345333614438, 5.243569643749998122 ) ) ;
#43526 = CARTESIAN_POINT ( 'NONE',  ( 20.25937500061451502, 2.746126346562643317, 4.756430356249998326 ) ) ;
#43527 = CARTESIAN_POINT ( 'NONE',  ( 7.921875000614517326, -6.054752690667223547, -1.112240025338166033E-15 ) ) ;
#43528 = CARTESIAN_POINT ( 'NONE',  ( 24.07499999999999929, 4.330127018922191873, 2.499999999999999556 ) ) ;
#43529 = CARTESIAN_POINT ( 'NONE',  ( 21.30000000122903359, -2.886751345948125991, -5.000000000000000000 ) ) ;
#43530 = CYLINDRICAL_SURFACE ( 'NONE', #2486, 3.999999999999996447 ) ;
#43531 = CARTESIAN_POINT ( 'NONE',  ( 9.984375000614518214, 4.541064518000418104, 2.621784821874999949 ) ) ;
#43532 = CARTESIAN_POINT ( 'NONE',  ( 13.43437500061451750, 6.421520780324663323E-16, -5.243569643749999010 ) ) ;
#43533 = CARTESIAN_POINT ( 'NONE',  ( 25.20937500061451431, 4.541064518000418104, -2.621784821874998173 ) ) ;
#43534 = CARTESIAN_POINT ( 'NONE',  ( 4.228125000614517681, -4.541064518000419881, 2.621784821874995952 ) ) ;
#43535 = ORIENTED_EDGE ( 'NONE', *, *, #60834, .T. ) ;
#43536 = CARTESIAN_POINT ( 'NONE',  ( 12.97499999999999964, -4.330127018922194537, 2.499999999999995559 ) ) ;
#43537 = CARTESIAN_POINT ( 'NONE',  ( 18.53437500061451715, 4.541064518000418104, 2.621784821874999949 ) ) ;
#43538 = CARTESIAN_POINT ( 'NONE',  ( 9.234375000614518214, -4.541064518000419881, 2.621784821874995952 ) ) ;
#43539 = CARTESIAN_POINT ( 'NONE',  ( -7.967954043666661671E-16, 13.87812499938548250, 34.33755215474603517 ) ) ;
#43540 = CARTESIAN_POINT ( 'NONE',  ( 20.69999999999999929, -4.330127018922190985, -2.500000000000001332 ) ) ;
#43541 = CARTESIAN_POINT ( 'NONE',  ( 2.000000000000000444, 16.17500000000000071, 26.53589838486224650 ) ) ;
#43542 = CARTESIAN_POINT ( 'NONE',  ( -2.121784821874996840, 10.03437500061451892, -26.32496088578401583 ) ) ;
#43543 = CARTESIAN_POINT ( 'NONE',  ( 23.52187500061451786, 2.746126346562643317, 4.756430356249998326 ) ) ;
#43544 = CARTESIAN_POINT ( 'NONE',  ( 11.91562500061451857, -6.054752690667223547, -1.112240025338166033E-15 ) ) ;
#43545 = CARTESIAN_POINT ( 'NONE',  ( 28.20937500061451786, -4.541064518000417216, -2.621784821875001281 ) ) ;
#43546 = DIRECTION ( 'NONE',  ( 1.000000000000000000, 0.000000000000000000, -0.000000000000000000 ) ) ;
#43547 = CARTESIAN_POINT ( 'NONE',  ( 12.75000000000000178, 4.330127018922192761, -2.499999999999997780 ) ) ;
#43548 = CARTESIAN_POINT ( 'NONE',  ( 1.999999999999998668, 19.06250000122903288, 26.53589838486224650 ) ) ;
#43549 = CARTESIAN_POINT ( 'NONE',  ( 11.96250000122903501, 4.330127018922192761, -2.499999999999997780 ) ) ;
#43550 = CARTESIAN_POINT ( 'NONE',  ( 22.88437500061451857, 6.421520780324663323E-16, -5.243569643749999010 ) ) ;
#43551 = CARTESIAN_POINT ( 'NONE',  ( 17.25937500061451502, 0.000000000000000000, 5.243569643749999010 ) ) ;
#43552 = CARTESIAN_POINT ( 'NONE',  ( 4.000000000000000000, 16.70000000122903216, 32.30940107675849760 ) ) ;
#43553 = ORIENTED_EDGE ( 'NONE', *, *, #27246, .T. ) ;
#43554 = CARTESIAN_POINT ( 'NONE',  ( 16.49062500061451786, -3.027376345333610441, -5.243569643749999898 ) ) ;
#43555 = CARTESIAN_POINT ( 'NONE',  ( 29.51250000122903216, 4.330127018922192761, -2.499999999999997780 ) ) ;
#43556 = CARTESIAN_POINT ( 'NONE',  ( 16.65937500061452070, 4.541064518000418104, -2.621784821874998173 ) ) ;
#43557 = CARTESIAN_POINT ( 'NONE',  ( 5.690625000614516260, -3.027376345333610441, -5.243569643749999898 ) ) ;
#43558 = CARTESIAN_POINT ( 'NONE',  ( 19.75312500061451360, 4.541064518000418104, -2.621784821874998173 ) ) ;
#43559 = CARTESIAN_POINT ( 'NONE',  ( 3.999999999999998668, 18.46249999999999858, -32.30940107675850470 ) ) ;
#43560 = CARTESIAN_POINT ( 'NONE',  ( 29.52187500061451431, -6.054752690667223547, -1.112240025338166033E-15 ) ) ;
#43561 = CARTESIAN_POINT ( 'NONE',  ( 2.121784821874999061, 12.90312500061451750, 26.32496088578401583 ) ) ;
#43562 = CARTESIAN_POINT ( 'NONE',  ( 16.92187500061451999, -6.054752690667223547, -1.112240025338166033E-15 ) ) ;
#43563 = CARTESIAN_POINT ( 'NONE',  ( 17.47500000122903430, 2.886751345948126879, 4.999999999999999112 ) ) ;
#43564 = CARTESIAN_POINT ( 'NONE',  ( 9.346875000614517148, -2.746126346562641984, -4.756430356249999214 ) ) ;
#43565 = CARTESIAN_POINT ( 'NONE',  ( 4.243569643749999898, 19.59687500061451360, -27.54997392385601529 ) ) ;
#43566 = EDGE_CURVE ( 'NONE', #46196, #6912, #22749, .T. ) ;
#43567 = CARTESIAN_POINT ( 'NONE',  ( 20.44687500061451857, -3.027376345333614438, 5.243569643749998122 ) ) ;
#43568 = CARTESIAN_POINT ( 'NONE',  ( 22.91250000122903430, 0.000000000000000000, 4.999999999999998224 ) ) ;
#43569 = CARTESIAN_POINT ( 'NONE',  ( 23.35312500061451857, 4.541064518000418104, -2.621784821874998173 ) ) ;
#43570 = CARTESIAN_POINT ( 'NONE',  ( 16.13437500061451502, 6.421520780324663323E-16, -5.243569643749999010 ) ) ;
#43571 = CARTESIAN_POINT ( 'NONE',  ( 11.31562500061451892, 3.027376345333611329, 5.243569643749999010 ) ) ;
#43572 = CARTESIAN_POINT ( 'NONE',  ( -4.243569643749997233, 13.59687500061451715, 32.45002607614398471 ) ) ;
#43573 = CARTESIAN_POINT ( 'NONE',  ( 17.80312500061451786, -4.541064518000417216, -2.621784821875001281 ) ) ;
#43574 = CARTESIAN_POINT ( 'NONE',  ( 26.12812500061451360, 4.541064518000418104, 2.621784821874999949 ) ) ;
#43575 = VERTEX_POINT ( 'NONE', #41072 ) ;
#43576 = VERTEX_POINT ( 'NONE', #58391 ) ;
#43577 = CARTESIAN_POINT ( 'NONE',  ( 22.19999999999999574, 4.330127018922192761, -2.499999999999997780 ) ) ;
#43578 = CARTESIAN_POINT ( 'NONE',  ( -2.121784821874999949, 19.33437500061451786, -33.67503911421598417 ) ) ;
#43579 = CARTESIAN_POINT ( 'NONE',  ( 3.809532709742158296, -3.238520787748959240, -3.970891474530591658 ) ) ;
#43580 = CARTESIAN_POINT ( 'NONE',  ( 24.96562500061451573, -6.054752690667223547, -1.112240025338166033E-15 ) ) ;
#43581 = CARTESIAN_POINT ( 'NONE',  ( 5.240625000614516971, -3.027376345333610441, -5.243569643749999898 ) ) ;
#43582 = CARTESIAN_POINT ( 'NONE',  ( 16.83750000122903145, 6.123233995736764310E-16, -4.999999999999998224 ) ) ;
#43583 = CARTESIAN_POINT ( 'NONE',  ( 21.85312500061451502, -4.541064518000417216, -2.621784821875001281 ) ) ;
#43584 = CARTESIAN_POINT ( 'NONE',  ( 23.47499999999999787, 6.123233995736764310E-16, -4.999999999999998224 ) ) ;
#43585 = CARTESIAN_POINT ( 'NONE',  ( 25.49062500061451786, -3.027376345333610441, -5.243569643749999898 ) ) ;
#43586 = CARTESIAN_POINT ( 'NONE',  ( 6.965625000614518392, -6.054752690667223547, -1.112240025338166033E-15 ) ) ;
#43587 = ORIENTED_EDGE ( 'NONE', *, *, #48200, .T. ) ;
#43588 = CARTESIAN_POINT ( 'NONE',  ( 22.82812500061451644, 6.421520780324663323E-16, -5.243569643749999010 ) ) ;
#43589 = LINE ( 'NONE', #38401, #37204 ) ;
#43590 = CARTESIAN_POINT ( 'NONE',  ( 10.69687500061451679, -2.746126346562642428, -4.756430356249999214 ) ) ;
#43591 = CARTESIAN_POINT ( 'NONE',  ( 11.13750000122903216, 4.330127018922191873, 2.499999999999999556 ) ) ;
#43592 = CARTESIAN_POINT ( 'NONE',  ( 3.999999999999998668, 14.52500000122903323, -32.30940107675850470 ) ) ;
#43593 = ADVANCED_FACE ( 'NONE', ( #41781 ), #7804, .F. ) ;
#43594 = CARTESIAN_POINT ( 'NONE',  ( -1.999999999999997113, 10.28750000122903430, 33.46410161513775705 ) ) ;
#43595 = CARTESIAN_POINT ( 'NONE',  ( 11.36250000000000071, 2.886751345948129099, -4.999999999999998224 ) ) ;
#43596 = CARTESIAN_POINT ( 'NONE',  ( 11.89687500061451608, -3.027376345333614438, 5.243569643749998122 ) ) ;
#43597 = CARTESIAN_POINT ( 'NONE',  ( 5.587500001229033231, 6.123233995736764310E-16, -4.999999999999998224 ) ) ;
#43598 = CARTESIAN_POINT ( 'NONE',  ( 13.84687500061451537, -3.027376345333610441, -5.243569643749999898 ) ) ;
#43599 = CARTESIAN_POINT ( 'NONE',  ( 6.121875000614517504, -6.054752690667223547, -1.112240025338166033E-15 ) ) ;
#43600 = CARTESIAN_POINT ( 'NONE',  ( 3.999999999999998668, 18.46249999999999858, 27.69059892324149530 ) ) ;
#43601 = CYLINDRICAL_SURFACE ( 'NONE', #7602, 3.999999999999996447 ) ;
#43602 = CARTESIAN_POINT ( 'NONE',  ( 11.40937500061451892, 0.000000000000000000, 5.243569643749999010 ) ) ;
#43603 = DIRECTION ( 'NONE',  ( 0.000000000000000000, 0.000000000000000000, 1.000000000000000000 ) ) ;
#43604 = CARTESIAN_POINT ( 'NONE',  ( 22.30312500061451431, -4.541064518000417216, -2.621784821875001281 ) ) ;
#43605 = CARTESIAN_POINT ( 'NONE',  ( 4.243569643749999898, 10.59687500061451715, 32.45002607614398471 ) ) ;
#43606 = CARTESIAN_POINT ( 'NONE',  ( 20.00625000122903430, 4.330127018922192761, -2.499999999999997780 ) ) ;
#43607 = CARTESIAN_POINT ( 'NONE',  ( 22.77187500061451786, -6.054752690667223547, -1.112240025338166033E-15 ) ) ;
#43608 = CARTESIAN_POINT ( 'NONE',  ( 4.154761151537816666, 2.781809049394522670, -4.180738899374664364 ) ) ;
#43609 = CARTESIAN_POINT ( 'NONE',  ( 28.53750000122903074, 6.123233995736764310E-16, -4.999999999999998224 ) ) ;
#43610 = CARTESIAN_POINT ( 'NONE',  ( 19.43437500061451573, -2.746126346562646425, 4.756430356249996549 ) ) ;
#43611 = CARTESIAN_POINT ( 'NONE',  ( 25.34062500061451217, -3.027376345333614438, 5.243569643749998122 ) ) ;
#43612 = CARTESIAN_POINT ( 'NONE',  ( 17.27812500061451217, -4.541064518000419881, 2.621784821874995952 ) ) ;
#43613 = CARTESIAN_POINT ( 'NONE',  ( 13.93125000122903323, -4.330127018922194537, 2.499999999999995559 ) ) ;
#43614 = CARTESIAN_POINT ( 'NONE',  ( 14.40937500061451715, 4.541064518000418104, -2.621784821874998173 ) ) ;
#43615 = CARTESIAN_POINT ( 'NONE',  ( -2.000000000000001776, 15.94999999999999929, 33.46410161513775705 ) ) ;
#43616 = CARTESIAN_POINT ( 'NONE',  ( 27.26250000122903216, 4.330127018922192761, -2.499999999999997780 ) ) ;
#43617 = CARTESIAN_POINT ( 'NONE',  ( 5.821875000614519458, 3.027376345333613106, -5.243569643749998122 ) ) ;
#43618 = CARTESIAN_POINT ( 'NONE',  ( 17.44687500061451857, -3.027376345333610441, -5.243569643749999898 ) ) ;
#43619 = CARTESIAN_POINT ( 'NONE',  ( 4.854383007807864026, -1.197900502339936502, -5.104905189653401010 ) ) ;
#43620 = CARTESIAN_POINT ( 'NONE',  ( 23.17500000000000071, 4.330127018922191873, 2.499999999999999556 ) ) ;
#43621 = CARTESIAN_POINT ( 'NONE',  ( 3.300000001229034918, -2.886751345948125991, -5.000000000000000000 ) ) ;
#43622 = CARTESIAN_POINT ( 'NONE',  ( 25.09687500061451715, -3.027376345333610441, -5.243569643749999898 ) ) ;
#43623 = CARTESIAN_POINT ( 'NONE',  ( 16.13437500061451502, 6.421520780324663323E-16, -5.243569643749999010 ) ) ;
#43624 = CARTESIAN_POINT ( 'NONE',  ( -3.756430356250000102, 14.32812499938548356, 30.00000000000000000 ) ) ;
#43625 = CARTESIAN_POINT ( 'NONE',  ( 29.02499999999999858, 4.330127018922191873, 2.499999999999999556 ) ) ;
#43626 = CARTESIAN_POINT ( 'NONE',  ( 6.562500000000001776, 2.886751345948126879, 4.999999999999999112 ) ) ;
#43627 = CARTESIAN_POINT ( 'NONE',  ( 10.28437500061451892, 5.492252693125287522, 3.363034840372157021E-16 ) ) ;
#43628 = CARTESIAN_POINT ( 'NONE',  ( 20.46562500061451928, -6.054752690667223547, -1.112240025338166033E-15 ) ) ;
#43629 = CARTESIAN_POINT ( 'NONE',  ( 9.449999999999999289, -4.330127018922190985, -2.500000000000001332 ) ) ;
#43630 = CARTESIAN_POINT ( 'NONE',  ( 4.190625000614518925, -3.027376345333614438, 5.243569643749998122 ) ) ;
#43631 = CARTESIAN_POINT ( 'NONE',  ( 20.02500000000000213, 4.330127018922191873, 2.499999999999999556 ) ) ;
#43632 = DIRECTION ( 'NONE',  ( 0.000000000000000000, 0.000000000000000000, -1.000000000000000000 ) ) ;
#43633 = CARTESIAN_POINT ( 'NONE',  ( 22.91250000122903430, 0.000000000000000000, 4.999999999999998224 ) ) ;
#43634 = CARTESIAN_POINT ( 'NONE',  ( 2.516032931661821959, 9.680092174376738967, 35.45051723330771409 ) ) ;
#43635 = CARTESIAN_POINT ( 'NONE',  ( 29.40937500061451715, 0.000000000000000000, 5.243569643749999010 ) ) ;
#43636 = VERTEX_POINT ( 'NONE', #34784 ) ;
#43637 = CARTESIAN_POINT ( 'NONE',  ( 16.37812500061451715, -4.541064518000419881, 2.621784821874995952 ) ) ;
#43638 = CARTESIAN_POINT ( 'NONE',  ( 23.46562500061451573, 3.027376345333611329, 5.243569643749999010 ) ) ;
#43639 = CARTESIAN_POINT ( 'NONE',  ( 25.99687500061451928, -3.027376345333610441, -5.243569643749999898 ) ) ;
#43640 = CARTESIAN_POINT ( 'NONE',  ( 8.849999999999999645, 0.000000000000000000, 4.999999999999998224 ) ) ;
#43641 = CARTESIAN_POINT ( 'NONE',  ( 12.44062500061451537, -3.027376345333610441, -5.243569643749999898 ) ) ;
#43642 = CARTESIAN_POINT ( 'NONE',  ( 27.81562500061452070, 3.027376345333613106, -5.243569643749998122 ) ) ;
#43643 = CARTESIAN_POINT ( 'NONE',  ( 14.44687500061451679, 6.054752690667223547, 3.707466751127219781E-16 ) ) ;
#43644 = CARTESIAN_POINT ( 'NONE',  ( 19.05937500061451928, 0.000000000000000000, 5.243569643749999010 ) ) ;
#43645 = CARTESIAN_POINT ( 'NONE',  ( 2.000000000000000444, 14.76874999877096606, 26.53589838486224650 ) ) ;
#43646 = CARTESIAN_POINT ( 'NONE',  ( -4.243569643749999898, 10.37187500061451750, 27.54997392385601529 ) ) ;
#43647 = CARTESIAN_POINT ( 'NONE',  ( 24.45000000122903572, -2.886751345948125991, -5.000000000000000000 ) ) ;
#43648 = CARTESIAN_POINT ( 'NONE',  ( 18.30937500061451928, -4.119189519843965641, -2.378215178125001383 ) ) ;
#43649 = CARTESIAN_POINT ( 'NONE',  ( 14.54062500061451679, -3.027376345333614438, 5.243569643749998122 ) ) ;
#43650 = CARTESIAN_POINT ( 'NONE',  ( 6.984375000614516438, -4.541064518000419881, 2.621784821874995952 ) ) ;
#43651 = CARTESIAN_POINT ( 'NONE',  ( 6.871875000614517504, 3.027376345333611329, 5.243569643749999010 ) ) ;
#43652 =( BOUNDED_CURVE ( )  B_SPLINE_CURVE ( 2, ( #54315, #3705, #9604, #14406, #48770, #37672, #60194, #48039, #15494 ),
 .UNSPECIFIED., .F., .F. ) 
 B_SPLINE_CURVE_WITH_KNOTS ( ( 3, 2, 2, 2, 3 ),
 ( 0.9021739130434782705, 0.9057971014492753881, 0.9130434782608695121, 0.9202898550724637472, 0.9239130434782608647 ),
 .UNSPECIFIED. ) 
 CURVE ( )  GEOMETRIC_REPRESENTATION_ITEM ( )  RATIONAL_B_SPLINE_CURVE ( ( 0.9330127018922194093, 0.9330127018922194093, 1.000000000000000000, 0.8660254037844387076, 1.000000000000000000, 0.8660254037844387076, 1.000000000000000000, 0.9330127018922194093, 0.9330127018922194093 ) ) 
 REPRESENTATION_ITEM ( '' )  );
#43653 = ORIENTED_EDGE ( 'NONE', *, *, #72942, .T. ) ;
#43654 = CARTESIAN_POINT ( 'NONE',  ( 28.39687500061452141, 6.054752690667223547, 3.707466751127219781E-16 ) ) ;
#43655 = CARTESIAN_POINT ( 'NONE',  ( 19.41562500061451146, 3.027376345333611329, 5.243569643749999010 ) ) ;
#43656 = EDGE_CURVE ( 'NONE', #56819, #35566, #35511, .T. ) ;
#43657 = CARTESIAN_POINT ( 'NONE',  ( 3.834375000614519635, -4.541064518000419881, 2.621784821874995952 ) ) ;
#43658 = CARTESIAN_POINT ( 'NONE',  ( 25.09687500061451715, -3.027376345333610441, -5.243569643749999898 ) ) ;
#43659 = CARTESIAN_POINT ( 'NONE',  ( 19.49062500061451431, -3.027376345333614438, 5.243569643749998122 ) ) ;
#43660 = CARTESIAN_POINT ( 'NONE',  ( -3.999999999999997335, 11.03750000000000142, 32.30940107675850470 ) ) ;
#43661 = CARTESIAN_POINT ( 'NONE',  ( 25.79062500061451502, -3.027376345333614438, 5.243569643749998122 ) ) ;
#43662 = CARTESIAN_POINT ( 'NONE',  ( 7.425000001229034474, 2.886751345948129099, -4.999999999999998224 ) ) ;
#43663 = EDGE_LOOP ( 'NONE', ( #38496, #47879, #63460, #51659 ) ) ;
#43664 = CARTESIAN_POINT ( 'NONE',  ( 3.000000001229032875, 5.773502691896255534, 3.535250795749688894E-16 ) ) ;
#43665 = CARTESIAN_POINT ( 'NONE',  ( 8.484601909799253346E-16, 14.26250000000000107, -25.38119784648299770 ) ) ;
#43666 = CARTESIAN_POINT ( 'NONE',  ( 22.27500000122903145, 2.886751345948129099, -4.999999999999998224 ) ) ;
#43667 = CARTESIAN_POINT ( 'NONE',  ( -7.967954043666661671E-16, 14.89062499938548179, 34.33755215474603517 ) ) ;
#43668 = CARTESIAN_POINT ( 'NONE',  ( 3.609375000614516882, 4.541064518000418104, -2.621784821874998173 ) ) ;
#43669 = CARTESIAN_POINT ( 'NONE',  ( 4.382503833126124348, 2.407183933188114189, -4.599998881930862815 ) ) ;
#43670 = CARTESIAN_POINT ( 'NONE',  ( 13.60312500061451679, 0.000000000000000000, 5.243569643749999010 ) ) ;
#43671 = CARTESIAN_POINT ( 'NONE',  ( 9.496875000614517504, 6.054752690667223547, 3.707466751127219781E-16 ) ) ;
#43672 = CARTESIAN_POINT ( 'NONE',  ( 23.73750000122903359, 4.330127018922191873, 2.499999999999999556 ) ) ;
#43673 = CARTESIAN_POINT ( 'NONE',  ( 14.37187500061451750, 3.027376345333612662, -5.243569643749998122 ) ) ;
#43674 = CARTESIAN_POINT ( 'NONE',  ( 29.24062500061451431, 6.054752690667223547, 3.707466751127219781E-16 ) ) ;
#43675 = CARTESIAN_POINT ( 'NONE',  ( 29.69999999999999574, -4.330127018922190985, -2.500000000000001332 ) ) ;
#43676 = CARTESIAN_POINT ( 'NONE',  ( 5.353125000614515905, 4.541064518000418104, -2.621784821874998173 ) ) ;
#43677 = CARTESIAN_POINT ( 'NONE',  ( 16.04062500061451857, -3.027376345333610441, -5.243569643749999898 ) ) ;
#43678 = ORIENTED_EDGE ( 'NONE', *, *, #31941, .T. ) ;
#43679 = CARTESIAN_POINT ( 'NONE',  ( 12.92812500061451786, 6.421520780324663323E-16, -5.243569643749999010 ) ) ;
#43680 = CARTESIAN_POINT ( 'NONE',  ( 7.528125000614515727, 6.421520780324663323E-16, -5.243569643749999010 ) ) ;
#43681 = CARTESIAN_POINT ( 'NONE',  ( 19.69687500061451857, -2.746126346562642428, -4.756430356249999214 ) ) ;
#43682 = CARTESIAN_POINT ( 'NONE',  ( 8.625000000000000000, 6.123233995736764310E-16, -4.999999999999998224 ) ) ;
#43683 = CARTESIAN_POINT ( 'NONE',  ( 5.325000001229033941, 2.886751345948126879, 4.999999999999999112 ) ) ;
#43684 = CARTESIAN_POINT ( 'NONE',  ( 18.63749999999999929, 5.773502691896255534, 3.535250795749688894E-16 ) ) ;
#43685 = CARTESIAN_POINT ( 'NONE',  ( 18.27187500061451431, -6.054752690667223547, -1.112240025338166033E-15 ) ) ;
#43686 = CARTESIAN_POINT ( 'NONE',  ( 14.21250000122903323, 4.330127018922192761, -2.499999999999997780 ) ) ;
#43687 = CARTESIAN_POINT ( 'NONE',  ( 21.86250000000000071, 2.886751345948126879, 4.999999999999999112 ) ) ;
#43688 = CARTESIAN_POINT ( 'NONE',  ( -4.243569643749997233, 17.59062500061451928, -27.54997392385601174 ) ) ;
#43689 = DIRECTION ( 'NONE',  ( -0.000000000000000000, -1.000000000000000000, -0.000000000000000000 ) ) ;
#43690 = CARTESIAN_POINT ( 'NONE',  ( 24.13125000122903074, 4.330127018922191873, 2.499999999999999556 ) ) ;
#43691 = DIRECTION ( 'NONE',  ( 0.000000000000000000, 0.000000000000000000, -1.000000000000000000 ) ) ;
#43692 = ADVANCED_FACE ( 'NONE', ( #19227 ), #64310, .F. ) ;
#43693 = DIRECTION ( 'NONE',  ( 1.000000000000000000, 0.000000000000000000, 0.000000000000000000 ) ) ;
#43694 = CARTESIAN_POINT ( 'NONE',  ( 24.29999999999999716, -4.330127018922190985, -2.500000000000001332 ) ) ;
#43695 = CARTESIAN_POINT ( 'NONE',  ( 13.09687500061451892, 6.054752690667223547, 3.707466751127219781E-16 ) ) ;
#43696 =( BOUNDED_CURVE ( )  B_SPLINE_CURVE ( 2, ( #32419, #70484, #25412, #32785, #54589, #3623, #59749 ),
 .UNSPECIFIED., .F., .F. ) 
 B_SPLINE_CURVE_WITH_KNOTS ( ( 3, 2, 2, 3 ),
 ( 0.9255912413769717961, 0.9277777777777778123, 0.9305555555555555802, 0.9324201688484926587 ),
 .UNSPECIFIED. ) 
 CURVE ( )  GEOMETRIC_REPRESENTATION_ITEM ( )  RATIONAL_B_SPLINE_CURVE ( ( 0.9551069630786563902, 0.8945414806928990714, 1.000000000000000000, 0.8660254037844387076, 1.000000000000000000, 0.9100681073130109100, 0.9408717204714907023 ) ) 
 REPRESENTATION_ITEM ( '' )  );
#43697 = CARTESIAN_POINT ( 'NONE',  ( 26.81250000000000000, 2.886751345948126879, 4.999999999999999112 ) ) ;
#43698 = CARTESIAN_POINT ( 'NONE',  ( 10.49062500061451431, -3.027376345333614438, 5.243569643749998122 ) ) ;
#43699 = CARTESIAN_POINT ( 'NONE',  ( 26.63437500061451146, -2.746126346562646425, 4.756430356249996549 ) ) ;
#43700 = CARTESIAN_POINT ( 'NONE',  ( 22.35937500061451644, -4.541064518000417216, -2.621784821875001281 ) ) ;
#43701 = CARTESIAN_POINT ( 'NONE',  ( 13.95937500061451431, 2.746126346562643317, 4.756430356249998326 ) ) ;
#43702 = CARTESIAN_POINT ( 'NONE',  ( 8.578125000614518214, 4.541064518000418104, 2.621784821874999949 ) ) ;
#43703 = CARTESIAN_POINT ( 'NONE',  ( 13.35937500061451821, -4.541064518000417216, -2.621784821875001281 ) ) ;
#43704 = ORIENTED_EDGE ( 'NONE', *, *, #45017, .T. ) ;
#43705 = CARTESIAN_POINT ( 'NONE',  ( 24.34687500061451715, 6.054752690667223547, 3.707466751127219781E-16 ) ) ;
#43706 = CARTESIAN_POINT ( 'NONE',  ( 0.5593513097472507800, 4.976037924071840202, -33.97015631813161463 ) ) ;
#43707 = DIRECTION ( 'NONE',  ( 0.000000000000000000, 0.000000000000000000, -1.000000000000000000 ) ) ;
#43708 = CARTESIAN_POINT ( 'NONE',  ( 4.650000000000001243, 4.330127018922192761, -2.499999999999997780 ) ) ;
#43709 = CARTESIAN_POINT ( 'NONE',  ( 16.31250000122903288, -4.330127018922190985, -2.500000000000001332 ) ) ;
#43710 = CARTESIAN_POINT ( 'NONE',  ( -4.000000000000000888, 19.90624999877096712, 32.30940107675850470 ) ) ;
#43711 = CARTESIAN_POINT ( 'NONE',  ( 7.771875000614516082, -4.119189519843968306, 2.378215178124996054 ) ) ;
#43712 = ORIENTED_EDGE ( 'NONE', *, *, #55693, .T. ) ;
#43713 = CARTESIAN_POINT ( 'NONE',  ( 15.29999999999999893, -4.330127018922190985, -2.500000000000001332 ) ) ;
#43714 = CARTESIAN_POINT ( 'NONE',  ( 15.78749999999999964, -2.886751345948125991, -5.000000000000000000 ) ) ;
#43715 = CARTESIAN_POINT ( 'NONE',  ( 11.80312500061451608, 0.000000000000000000, 5.243569643749999010 ) ) ;
#43716 = VERTEX_POINT ( 'NONE', #36243 ) ;
#43717 = CARTESIAN_POINT ( 'NONE',  ( 3.628170623289135754, -3.971039094590678165, 3.121958529326629428 ) ) ;
#43718 = CARTESIAN_POINT ( 'NONE',  ( -4.243569643749999898, 17.57187500061451502, -32.45002607614398471 ) ) ;
#43719 = CARTESIAN_POINT ( 'NONE',  ( 4.265625000614517326, -6.054752690667223547, -1.112240025338166033E-15 ) ) ;
#43720 = CARTESIAN_POINT ( 'NONE',  ( 3.756430356250000546, 14.92812499938548321, 27.83122392262697886 ) ) ;
#43721 = CARTESIAN_POINT ( 'NONE',  ( 9.525000000000002132, 6.123233995736764310E-16, -4.999999999999998224 ) ) ;
#43722 = CARTESIAN_POINT ( 'NONE',  ( 30.00000000000000000, 6.123233995736764310E-16, -4.999999999999998224 ) ) ;
#43723 = ORIENTED_EDGE ( 'NONE', *, *, #29408, .T. ) ;
#43724 = CARTESIAN_POINT ( 'NONE',  ( 23.50312500061451360, 0.000000000000000000, 5.243569643749999010 ) ) ;
#43725 = CARTESIAN_POINT ( 'NONE',  ( 4.229059543195655024, -2.667460491576031156, 4.514416570572414855 ) ) ;
#43726 = CARTESIAN_POINT ( 'NONE',  ( -3.756430356250001434, 19.65312499938548640, 32.16877607737301048 ) ) ;
#43727 = CARTESIAN_POINT ( 'NONE',  ( 22.32187500061451502, -6.054752690667223547, -1.112240025338166033E-15 ) ) ;
#43728 = CARTESIAN_POINT ( 'NONE',  ( 19.52812500061451573, -4.541064518000419881, 2.621784821874995952 ) ) ;
#43729 = CARTESIAN_POINT ( 'NONE',  ( 9.001249775931846008E-16, 13.61562500061459424, -25.09994784771203058 ) ) ;
#43730 = CARTESIAN_POINT ( 'NONE',  ( 24.45000000122903572, -2.886751345948125991, -5.000000000000000000 ) ) ;
#43731 = CARTESIAN_POINT ( 'NONE',  ( 4.228125000614517681, -4.541064518000419881, 2.621784821874995952 ) ) ;
#43732 = CARTESIAN_POINT ( 'NONE',  ( 24.45937500061451786, 0.000000000000000000, 4.756430356249998326 ) ) ;
#43733 = CARTESIAN_POINT ( 'NONE',  ( 22.22812500061451502, -4.541064518000419881, 2.621784821874995952 ) ) ;
#43734 = CARTESIAN_POINT ( 'NONE',  ( 8.746875000614515727, -2.746126346562646425, 4.756430356249996549 ) ) ;
#43735 = CARTESIAN_POINT ( 'NONE',  ( 1.878215178124997609, 17.96562499938548285, 33.25316411605952993 ) ) ;
#43736 = CARTESIAN_POINT ( 'NONE',  ( 15.83437500061451608, 4.541064518000418104, 2.621784821874999949 ) ) ;
#43737 = CARTESIAN_POINT ( 'NONE',  ( 15.60937500061451644, -4.541064518000417216, -2.621784821875001281 ) ) ;
#43738 = CARTESIAN_POINT ( 'NONE',  ( 22.47187500061451715, 3.027376345333613106, -5.243569643749998122 ) ) ;
#43739 = ORIENTED_EDGE ( 'NONE', *, *, #33984, .F. ) ;
#43740 = CARTESIAN_POINT ( 'NONE',  ( 2.121784821874999061, 11.60937500061451821, 26.32496088578401583 ) ) ;
#43741 = CARTESIAN_POINT ( 'NONE',  ( -1.999999999999997113, 14.78750000122903252, -26.53589838486224295 ) ) ;
#43742 = CARTESIAN_POINT ( 'NONE',  ( 26.61562500061451786, 3.027376345333611329, 5.243569643749999010 ) ) ;
#43743 = CARTESIAN_POINT ( 'NONE',  ( 27.66562500061451146, -6.054752690667223547, -1.112240025338166033E-15 ) ) ;
#43744 = CARTESIAN_POINT ( 'NONE',  ( 8.512500001229033941, 0.000000000000000000, 4.999999999999998224 ) ) ;
#43745 = CARTESIAN_POINT ( 'NONE',  ( 3.999999999999999112, 17.97500000000000142, 30.00000000000000000 ) ) ;
#43746 = CARTESIAN_POINT ( 'NONE',  ( 7.171875000614517326, 3.027376345333613106, -5.243569643749998122 ) ) ;
#43747 =( NAMED_UNIT ( * ) SI_UNIT ( $, .STERADIAN. ) SOLID_ANGLE_UNIT ( ) );
#43748 = CARTESIAN_POINT ( 'NONE',  ( 13.42500000122903536, 2.886751345948126879, 4.999999999999999112 ) ) ;
#43749 = CARTESIAN_POINT ( 'NONE',  ( 10.01250000122903394, -4.330127018922190985, -2.500000000000001332 ) ) ;
#43750 = CARTESIAN_POINT ( 'NONE',  ( 2.878125000614517592, -4.541064518000419881, 2.621784821874995952 ) ) ;
#43751 = CARTESIAN_POINT ( 'NONE',  ( 4.000000000000000000, 15.59374999877096535, 30.00000000000000000 ) ) ;
#43752 = CARTESIAN_POINT ( 'NONE',  ( 17.75625000122903074, 4.330127018922192761, -2.499999999999997780 ) ) ;
#43753 = CARTESIAN_POINT ( 'NONE',  ( 13.05937500061451750, 4.541064518000418104, -2.621784821874998173 ) ) ;
#43754 = CARTESIAN_POINT ( 'NONE',  ( 0.000000000000000000, 20.00000000000000000, 30.00000000000000000 ) ) ;
#43755 = ORIENTED_EDGE ( 'NONE', *, *, #72282, .T. ) ;
#43756 = CARTESIAN_POINT ( 'NONE',  ( 20.54062500061451502, -3.027376345333610441, -5.243569643749999898 ) ) ;
#43757 = CARTESIAN_POINT ( 'NONE',  ( 15.04687500061451644, -3.027376345333614438, 5.243569643749998122 ) ) ;
#43758 = CARTESIAN_POINT ( 'NONE',  ( 5.278125000614516615, 6.421520780324663323E-16, -5.243569643749999010 ) ) ;
#43759 = CARTESIAN_POINT ( 'NONE',  ( 21.49687500061451573, -3.027376345333610441, -5.243569643749999898 ) ) ;
#43760 = CARTESIAN_POINT ( 'NONE',  ( 4.903125000614516615, 4.541064518000418104, -2.621784821874998173 ) ) ;
#43761 = FACE_OUTER_BOUND ( 'NONE', #65958, .T. ) ;
#43763 = EDGE_CURVE ( 'NONE', #25000, #50521, #41094, .T. ) ;
#43762 = CARTESIAN_POINT ( 'NONE',  ( 6.975000001229032520, 2.886751345948129099, -4.999999999999998224 ) ) ;
#43764 = CARTESIAN_POINT ( 'NONE',  ( 22.19062500061451715, -3.027376345333614438, 5.243569643749998122 ) ) ;
#43765 = CARTESIAN_POINT ( 'NONE',  ( 4.000000000000000000, 17.15000000122903145, -27.69059892324149530 ) ) ;
#43766 = CARTESIAN_POINT ( 'NONE',  ( 7.725000001229034297, -5.773502691896255534, -1.060575238724906372E-15 ) ) ;
#43767 = CARTESIAN_POINT ( 'NONE',  ( 18.59062500061451573, -3.027376345333614438, 5.243569643749998122 ) ) ;
#43768 = CARTESIAN_POINT ( 'NONE',  ( 15.89062500061451289, -3.027376345333614438, 5.243569643749998122 ) ) ;
#43769 = CARTESIAN_POINT ( 'NONE',  ( 29.33437500061451431, 4.119189519843966529, 2.378215178124999607 ) ) ;
#43770 = CARTESIAN_POINT ( 'NONE',  ( 16.61250000000000426, -5.773502691896255534, -1.060575238724906372E-15 ) ) ;
#43771 = CARTESIAN_POINT ( 'NONE',  ( 11.77500000122903501, -5.773502691896255534, -1.060575238724906372E-15 ) ) ;
#43772 = CARTESIAN_POINT ( 'NONE',  ( 7.603125000614517681, 4.541064518000418104, -2.621784821874998173 ) ) ;
#43773 = CARTESIAN_POINT ( 'NONE',  ( 12.02812500061451573, 6.421520780324663323E-16, -5.243569643749999010 ) ) ;
#43774 = CARTESIAN_POINT ( 'NONE',  ( 21.60000000122903430, -2.886751345948129988, 4.999999999999997335 ) ) ;
#43775 = CARTESIAN_POINT ( 'NONE',  ( 2.121784821874999061, 14.75937500061451679, -33.67503911421598417 ) ) ;
#43776 = CARTESIAN_POINT ( 'NONE',  ( 18.27187500061451431, -6.054752690667223547, -1.112240025338166033E-15 ) ) ;
#43777 = CARTESIAN_POINT ( 'NONE',  ( 7.443750001229033408, 5.773502691896255534, 3.535250795749688401E-16 ) ) ;
#43778 = CARTESIAN_POINT ( 'NONE',  ( 5.250000001229035540, 5.773502691896255534, 3.535250795749688894E-16 ) ) ;
#43779 = CARTESIAN_POINT ( 'NONE',  ( 3.759375000614517681, 0.000000000000000000, 5.243569643749999010 ) ) ;
#43780 = CARTESIAN_POINT ( 'NONE',  ( 20.07187500061451857, -6.054752690667223547, -1.112240025338166033E-15 ) ) ;
#43781 = CARTESIAN_POINT ( 'NONE',  ( -3.999999999999997335, 15.08750000000000036, 32.30940107675850470 ) ) ;
#43782 = CARTESIAN_POINT ( 'NONE',  ( 18.66562500061451146, -6.054752690667223547, -1.112240025338166033E-15 ) ) ;
#43783 = CARTESIAN_POINT ( 'NONE',  ( 11.90625000122903465, 4.330127018922192761, -2.499999999999997780 ) ) ;
#43784 = CARTESIAN_POINT ( 'NONE',  ( -1.878215178124999163, 18.75312499938548427, 26.74683588394047007 ) ) ;
#43785 = CYLINDRICAL_SURFACE ( 'NONE', #64176, 4.000000000000000000 ) ;
#43786 = CARTESIAN_POINT ( 'NONE',  ( 27.68437500061451573, -4.541064518000419881, 2.621784821874995952 ) ) ;
#43787 = CARTESIAN_POINT ( 'NONE',  ( 20.14687500061451786, 4.119189519843966529, -2.378215178124998275 ) ) ;
#43788 = CARTESIAN_POINT ( 'NONE',  ( 15.55312500061451608, -4.541064518000417216, -2.621784821875001281 ) ) ;
#43789 = CARTESIAN_POINT ( 'NONE',  ( 13.95937500061451786, 4.541064518000418104, -2.621784821874998173 ) ) ;
#43790 = ORIENTED_EDGE ( 'NONE', *, *, #15195, .F. ) ;
#43791 = FACE_OUTER_BOUND ( 'NONE', #55527, .T. ) ;
#43792 = CARTESIAN_POINT ( 'NONE',  ( 23.91562500061451502, 3.027376345333611329, 5.243569643749999010 ) ) ;
#43793 = CYLINDRICAL_SURFACE ( 'NONE', #64008, 4.000000000000000000 ) ;
#43794 = CARTESIAN_POINT ( 'NONE',  ( 28.53750000122903074, 6.123233995736764310E-16, -4.999999999999998224 ) ) ;
#43795 = ADVANCED_FACE ( 'NONE', ( #31060 ), #17975, .T. ) ;
#43796 = CARTESIAN_POINT ( 'NONE',  ( 11.81250000000000000, 2.886751345948129099, -4.999999999999998224 ) ) ;
#43797 = ADVANCED_FACE ( 'NONE', ( #71063 ), #20438, .T. ) ;
#43798 = CARTESIAN_POINT ( 'NONE',  ( 23.36250000122903359, 0.000000000000000000, 4.999999999999998224 ) ) ;
#43799 = CARTESIAN_POINT ( 'NONE',  ( 17.99062500061451786, 6.054752690667223547, 3.707466751127219781E-16 ) ) ;
#43800 = ORIENTED_EDGE ( 'NONE', *, *, #45083, .T. ) ;
#43801 = CARTESIAN_POINT ( 'NONE',  ( 21.86250000000000071, 2.886751345948126879, 4.999999999999999112 ) ) ;
#43802 = CARTESIAN_POINT ( 'NONE',  ( 23.74687500061451573, -3.027376345333610441, -5.243569643749999898 ) ) ;
#43803 = VERTEX_POINT ( 'NONE', #3842 ) ;
#43804 = CARTESIAN_POINT ( 'NONE',  ( 2.000000000000000444, 19.32500000000000284, 26.53589838486224650 ) ) ;
#43805 = CARTESIAN_POINT ( 'NONE',  ( 10.67812500061451608, 6.421520780324663323E-16, -5.243569643749999010 ) ) ;
#43806 = CARTESIAN_POINT ( 'NONE',  ( 12.26249999999999751, 2.886751345948073588, -5.000000000000094147 ) ) ;
#43807 = CARTESIAN_POINT ( 'NONE',  ( 14.55937500061451750, -5.492252693125287522, -1.008910452111647106E-15 ) ) ;
#43808 = CARTESIAN_POINT ( 'NONE',  ( 18.26249999999999929, 2.886751345948126879, 4.999999999999999112 ) ) ;
#43809 = CARTESIAN_POINT ( 'NONE',  ( 24.82499999999999929, 6.123233995736764310E-16, -4.999999999999998224 ) ) ;
#43810 = CARTESIAN_POINT ( 'NONE',  ( -2.121784821874996840, 18.97812500061451857, 33.67503911421598417 ) ) ;
#43811 = CARTESIAN_POINT ( 'NONE',  ( 5.259375000614518569, -4.541064518000417216, -2.621784821875001281 ) ) ;
#43812 = CARTESIAN_POINT ( 'NONE',  ( 16.43437500061451573, -4.541064518000419881, 2.621784821874995952 ) ) ;
#43813 = CARTESIAN_POINT ( 'NONE',  ( 27.83437500061451786, 6.421520780324663323E-16, -5.243569643749999010 ) ) ;
#43814 = ORIENTED_EDGE ( 'NONE', *, *, #25568, .F. ) ;
#43815 = COLOUR_RGB ( '',0.8941176470588234615, 0.8941176470588234615, 0.8941176470588234615 ) ;
#43816 = CARTESIAN_POINT ( 'NONE',  ( 25.41562500061451146, -6.054752690667223547, -1.112240025338166033E-15 ) ) ;
#43817 = CARTESIAN_POINT ( 'NONE',  ( 27.19687500061451857, -3.027376345333614438, 5.243569643749998122 ) ) ;
#43818 = CARTESIAN_POINT ( 'NONE',  ( 45.00000000000000000, -8.874999999999998224, 1.494782592887687667 ) ) ;
#43819 = CARTESIAN_POINT ( 'NONE',  ( 14.77500000000000036, -4.330127018922194537, 2.499999999999995559 ) ) ;
#43820 = CARTESIAN_POINT ( 'NONE',  ( 11.42812500061451608, -4.541064518000419881, 2.621784821874995952 ) ) ;
#43821 = LINE ( 'NONE', #50457, #30409 ) ;
#43822 = CARTESIAN_POINT ( 'NONE',  ( 1.999999999999998668, 19.40000000000000213, -33.46410161513775705 ) ) ;
#43823 = CARTESIAN_POINT ( 'NONE',  ( 28.97812500061451502, -4.541064518000419881, 2.621784821874995952 ) ) ;
#43824 = CARTESIAN_POINT ( 'NONE',  ( 15.86250000122903181, -4.330127018922190985, -2.500000000000001332 ) ) ;
#43825 = LINE ( 'NONE', #64881, #40678 ) ;
#43826 = CARTESIAN_POINT ( 'NONE',  ( 14.97187500061451892, 2.746126346562643317, 4.756430356249998326 ) ) ;
#43827 = CARTESIAN_POINT ( 'NONE',  ( 5.053125000614517859, 0.000000000000000000, 5.243569643749999010 ) ) ;
#43828 = CARTESIAN_POINT ( 'NONE',  ( 21.98437500061451644, 6.421520780324663323E-16, -5.243569643749999010 ) ) ;
#43829 = CARTESIAN_POINT ( 'NONE',  ( 2.121784821875001281, 16.85937500061451999, 33.67503911421598417 ) ) ;
#43830 = CARTESIAN_POINT ( 'NONE',  ( 20.44687500061451857, -3.027376345333614438, 5.243569643749998122 ) ) ;
#43831 = CARTESIAN_POINT ( 'NONE',  ( 28.84687500061452070, 6.054752690667223547, 3.707466751127219781E-16 ) ) ;
#43832 = CARTESIAN_POINT ( 'NONE',  ( -3.000416591977282496E-16, 18.39687500061451786, 25.09994784771203058 ) ) ;
#43833 = CARTESIAN_POINT ( 'NONE',  ( 11.65312500061451573, 4.541064518000418104, -2.621784821874998173 ) ) ;
#43834 = CARTESIAN_POINT ( 'NONE',  ( 1.626862140677534273E-15, 15.27500000122903501, 34.00000000000000000 ) ) ;
#43835 = CARTESIAN_POINT ( 'NONE',  ( 8.071875000614518569, 3.027376345333613106, -5.243569643749998122 ) ) ;
#43836 = CARTESIAN_POINT ( 'NONE',  ( -5.810221930991193690E-16, 15.83749999999999680, -34.00000000000000000 ) ) ;
#43837 = CARTESIAN_POINT ( 'NONE',  ( 8.915625000614515017, 3.027376345333613106, -5.243569643749998122 ) ) ;
#43838 = CARTESIAN_POINT ( 'NONE',  ( 13.39687500061451608, -3.027376345333610441, -5.243569643749999898 ) ) ;
#43839 = CARTESIAN_POINT ( 'NONE',  ( 24.54375000122903216, 5.773502691896255534, 3.535250795749688401E-16 ) ) ;
#43840 = CARTESIAN_POINT ( 'NONE',  ( 21.63750000122903572, -4.330127018922194537, 2.499999999999995559 ) ) ;
#43841 = CARTESIAN_POINT ( 'NONE',  ( 7.659375000614518036, 4.541064518000418104, -2.621784821874998173 ) ) ;
#43842 = CARTESIAN_POINT ( 'NONE',  ( 9.553125000614517859, 0.000000000000000000, 5.243569643749999010 ) ) ;
#43843 = CARTESIAN_POINT ( 'NONE',  ( 24.69375000122903074, -2.886751345948129988, 4.999999999999997335 ) ) ;
#43844 = CARTESIAN_POINT ( 'NONE',  ( 21.30937500061451573, 0.000000000000000000, 5.243569643749999010 ) ) ;
#43845 = DIRECTION ( 'NONE',  ( 1.000000000000000000, 0.000000000000000000, 0.000000000000000000 ) ) ;
#43846 = CARTESIAN_POINT ( 'NONE',  ( -1.839935159944502630, 4.656359355287978730, 33.56177517597544835 ) ) ;
#43847 = DIRECTION ( 'NONE',  ( -1.000000000000000000, -0.000000000000000000, -0.000000000000000000 ) ) ;
#43848 = ADVANCED_FACE ( 'NONE', ( #26363 ), #71433, .F. ) ;
#43849 = CARTESIAN_POINT ( 'NONE',  ( 4.243569643749999898, 12.43437500061451750, -30.00000000000000000 ) ) ;
#43850 = CARTESIAN_POINT ( 'NONE',  ( 14.32500000122903394, 2.886751345948126879, 4.999999999999999112 ) ) ;
#43851 = B_SPLINE_CURVE_WITH_KNOTS ( 'NONE', 3,
 ( #29627, #11561, #29272, #57693, #34440, #56617, #51442, #50723, #28904, #24077 ),
 .UNSPECIFIED., .F., .F.,
 ( 4, 3, 3, 4 ),
 ( 0.000000000000000000, 0.0001572271610493928607, 0.0003144542605825271630, 0.0005320905539976019533 ),
 .UNSPECIFIED. ) ;
#43852 = CARTESIAN_POINT ( 'NONE',  ( 9.001249775931846008E-16, 15.41562500061451679, -25.09994784771203058 ) ) ;
#43853 = CARTESIAN_POINT ( 'NONE',  ( 18.26250000122903216, 4.330127018922192761, -2.499999999999997780 ) ) ;
#43854 = CARTESIAN_POINT ( 'NONE',  ( 9.965625000614517504, 3.027376345333611329, 5.243569643749999010 ) ) ;
#43855 = EDGE_LOOP ( 'NONE', ( #7806, #71888, #16796, #48163, #28104, #15756, #15392, #62455, #188, #61857, #66700, #39366, #53451, #69955, #46717, #68886, #51923, #50278, #23030 ) ) ;
#43856 = CARTESIAN_POINT ( 'NONE',  ( 14.02499999999999858, 6.123233995736764310E-16, -4.999999999999998224 ) ) ;
#43857 = CARTESIAN_POINT ( 'NONE',  ( 10.44375000122903252, -2.886751345948237457, -4.999999999999807265 ) ) ;
#43858 = CARTESIAN_POINT ( 'NONE',  ( 22.79062500061451502, -3.027376345333610441, -5.243569643749999898 ) ) ;
#43859 = CARTESIAN_POINT ( 'NONE',  ( 11.18437500061451928, 6.421520780324663323E-16, -5.243569643749999010 ) ) ;
#43860 = CARTESIAN_POINT ( 'NONE',  ( -1.999999999999997113, 14.33750000122903323, 33.46410161513775705 ) ) ;
#43861 = CARTESIAN_POINT ( 'NONE',  ( 9.075000001229033941, -5.773502691896255534, -1.060575238724906372E-15 ) ) ;
#43862 = CARTESIAN_POINT ( 'NONE',  ( 18.75000000122903288, 5.773502691896255534, 3.535250795749688894E-16 ) ) ;
#43863 = CARTESIAN_POINT ( 'NONE',  ( 15.70312500061451644, 4.541064518000418104, -2.621784821874998173 ) ) ;
#43864 =( BOUNDED_CURVE ( )  B_SPLINE_CURVE ( 2, ( #38583, #65921, #26772, #32303, #60360, #31939, #21577, #32672, #4606 ),
 .UNSPECIFIED., .F., .F. ) 
 B_SPLINE_CURVE_WITH_KNOTS ( ( 3, 2, 2, 2, 3 ),
 ( 0.4027777777777777901, 0.4074074074074073848, 0.4166666666666666852, 0.4259259259259259300, 0.4305555555555555802 ),
 .UNSPECIFIED. ) 
 CURVE ( )  GEOMETRIC_REPRESENTATION_ITEM ( )  RATIONAL_B_SPLINE_CURVE ( ( 0.9330127018922194093, 0.9330127018922197424, 1.000000000000000000, 0.8660254037844387076, 1.000000000000000000, 0.8660254037844387076, 1.000000000000000000, 0.9330127018922189652, 0.9330127018922194093 ) ) 
 REPRESENTATION_ITEM ( '' )  );
#43865 = CARTESIAN_POINT ( 'NONE',  ( 17.91562500061451502, 3.027376345333613106, -5.243569643749998122 ) ) ;
#43866 = CARTESIAN_POINT ( 'NONE',  ( 25.53750000122903074, 4.330127018922191873, 2.499999999999999556 ) ) ;
#43867 = CARTESIAN_POINT ( 'NONE',  ( 27.52500000122903145, -5.773502691896255534, -1.060575238724906372E-15 ) ) ;
#43868 = CARTESIAN_POINT ( 'NONE',  ( 22.01249999999999574, -5.773502691896255534, -1.060575238724906372E-15 ) ) ;
#43869 = CARTESIAN_POINT ( 'NONE',  ( 1.878215178124997609, 13.46562499938548285, 33.25316411605952993 ) ) ;
#43870 = CARTESIAN_POINT ( 'NONE',  ( 24.72187500061451360, 3.027376345333613106, -5.243569643749998122 ) ) ;
#43871 = CARTESIAN_POINT ( 'NONE',  ( -3.999999999999997335, 15.98750000000000249, 32.30940107675850470 ) ) ;
#43872 = CARTESIAN_POINT ( 'NONE',  ( 12.97500000122903252, 2.886751345948126879, 4.999999999999999112 ) ) ;
#43873 = CARTESIAN_POINT ( 'NONE',  ( 3.337499999999999911, 5.773502691896255534, 3.535250795749688894E-16 ) ) ;
#43874 = DIRECTION ( 'NONE',  ( -0.000000000000000000, -1.000000000000000000, -0.000000000000000000 ) ) ;
#43875 = CARTESIAN_POINT ( 'NONE',  ( 5.859375000614519102, 4.541064518000418104, -2.621784821874998173 ) ) ;
#43876 = CARTESIAN_POINT ( 'NONE',  ( 27.14062500061451644, -3.027376345333614438, 5.243569643749998122 ) ) ;
#43877 = CARTESIAN_POINT ( 'NONE',  ( -3.756430356249999214, 12.94062499938548427, 27.83122392262697176 ) ) ;
#43878 = CARTESIAN_POINT ( 'NONE',  ( -5.810221930991193690E-16, 10.55000000122903359, 26.00000000000000355 ) ) ;
#43879 = CARTESIAN_POINT ( 'NONE',  ( 10.88437500061451679, 4.541064518000418104, 2.621784821874999949 ) ) ;
#43880 = CARTESIAN_POINT ( 'NONE',  ( 4.294292190751133553, -2.561165899037177507, 4.480540752805964644 ) ) ;
#43881 = CARTESIAN_POINT ( 'NONE',  ( 28.82812500061451644, 4.541064518000418104, 2.621784821874999949 ) ) ;
#43882 = CARTESIAN_POINT ( 'NONE',  ( 8.409375000614518925, -4.541064518000417216, -2.621784821875001281 ) ) ;
#43883 = CARTESIAN_POINT ( 'NONE',  ( 29.25937500061451502, 4.541064518000418104, -2.621784821874998173 ) ) ;
#43884 = CARTESIAN_POINT ( 'NONE',  ( -4.243569643749998122, 13.09062500061459389, 32.45002607614398471 ) ) ;
#43885 = CARTESIAN_POINT ( 'NONE',  ( 23.02499999999999858, 6.123233995736764310E-16, -4.999999999999998224 ) ) ;
#43886 = ORIENTED_EDGE ( 'NONE', *, *, #31085, .F. ) ;
#43887 = CARTESIAN_POINT ( 'NONE',  ( 29.96250000000000213, 2.886751345948126879, 4.999999999999999112 ) ) ;
#43888 = EDGE_CURVE ( 'NONE', #33565, #28698, #25547, .T. ) ;
#43889 = CARTESIAN_POINT ( 'NONE',  ( 4.537500000000000533, -2.886751345948125991, -5.000000000000000000 ) ) ;
#43890 = ORIENTED_EDGE ( 'NONE', *, *, #59196, .F. ) ;
#43891 = VECTOR ( 'NONE', #42206, 1000.000000000000000 ) ;
#43892 = CARTESIAN_POINT ( 'NONE',  ( 17.76562500061451644, -6.054752690667223547, -1.112240025338166033E-15 ) ) ;
#43893 = CARTESIAN_POINT ( 'NONE',  ( 11.80312500061451608, 0.000000000000000000, 5.243569643749999010 ) ) ;
#43894 = CARTESIAN_POINT ( 'NONE',  ( 21.00937500061451857, 2.746126346562645981, -4.756430356249997438 ) ) ;
#43895 = CARTESIAN_POINT ( 'NONE',  ( 6.609375000614519102, -4.541064518000417216, -2.621784821875001281 ) ) ;
#43896 = CARTESIAN_POINT ( 'NONE',  ( 19.27500000122903145, 2.886751345948126879, 4.999999999999999112 ) ) ;
#43897 = CARTESIAN_POINT ( 'NONE',  ( 7.950000000000001954, 0.000000000000000000, 4.999999999999998224 ) ) ;
#43898 = CARTESIAN_POINT ( 'NONE',  ( 6.271875000614517859, 3.027376345333613106, -5.243569643749998122 ) ) ;
#43899 = CARTESIAN_POINT ( 'NONE',  ( 14.59687500061452070, -3.027376345333614438, 5.243569643749998122 ) ) ;
#43900 = CARTESIAN_POINT ( 'NONE',  ( 24.87187500061451573, 3.027376345333611329, 5.243569643749999010 ) ) ;
#43901 = CARTESIAN_POINT ( 'NONE',  ( 3.999999999999999112, 15.83750000122903501, -30.00000000000000000 ) ) ;
#43902 = ORIENTED_EDGE ( 'NONE', *, *, #70232, .F. ) ;
#43903 = CARTESIAN_POINT ( 'NONE',  ( 12.11250000000000249, -5.773502691896255534, -1.060575238724906372E-15 ) ) ;
#43904 = CARTESIAN_POINT ( 'NONE',  ( 17.40937500061451715, -4.541064518000417216, -2.621784821875001281 ) ) ;
#43905 =( BOUNDED_CURVE ( )  B_SPLINE_CURVE ( 2, ( #56410, #56757, #5801, #267, #39425, #10980, #57487, #998, #634 ),
 .UNSPECIFIED., .F., .F. ) 
 B_SPLINE_CURVE_WITH_KNOTS ( ( 3, 2, 2, 2, 3 ),
 ( 0.7065217391304348116, 0.7101449275362319291, 0.7173913043478260532, 0.7246376811594202882, 0.7282608695652174058 ),
 .UNSPECIFIED. ) 
 CURVE ( )  GEOMETRIC_REPRESENTATION_ITEM ( )  RATIONAL_B_SPLINE_CURVE ( ( 0.9330127018922194093, 0.9330127018922194093, 1.000000000000000000, 0.8660254037844387076, 1.000000000000000000, 0.8660254037844387076, 1.000000000000000000, 0.9330127018922194093, 0.9330127018922194093 ) ) 
 REPRESENTATION_ITEM ( '' )  );
#43906 = CARTESIAN_POINT ( 'NONE',  ( 10.58437500061451964, -4.541064518000419881, 2.621784821874995952 ) ) ;
#43907 = CARTESIAN_POINT ( 'NONE',  ( -1.878215178124999163, 15.49062499938548321, 26.74683588394047007 ) ) ;
#43908 = CARTESIAN_POINT ( 'NONE',  ( 20.92500000000000071, 4.330127018922191873, 2.499999999999999556 ) ) ;
#43909 = CARTESIAN_POINT ( 'NONE',  ( -3.999999999999999556, 16.28749999999999787, 27.69059892324149175 ) ) ;
#43910 = CARTESIAN_POINT ( 'NONE',  ( 22.80937500061451573, -4.119189519843965641, -2.378215178125001383 ) ) ;
#43911 = CARTESIAN_POINT ( 'NONE',  ( 12.59062500061451573, 6.054752690667223547, 3.707466751127219781E-16 ) ) ;
#43912 = CARTESIAN_POINT ( 'NONE',  ( 3.149999999999999911, -4.330127018922190985, -2.500000000000001332 ) ) ;
#43913 = CARTESIAN_POINT ( 'NONE',  ( 28.88437500061451502, 4.541064518000418104, 2.621784821874999949 ) ) ;
#43914 = CARTESIAN_POINT ( 'NONE',  ( 10.80000000000000071, -4.330127018922190985, -2.500000000000001332 ) ) ;
#43915 = CARTESIAN_POINT ( 'NONE',  ( -3.999999999999997335, 15.65000000122903501, 32.30940107675850470 ) ) ;
#43916 = CARTESIAN_POINT ( 'NONE',  ( 10.87500000122903288, -5.773502691896255534, -1.060575238724906372E-15 ) ) ;
#43917 = CARTESIAN_POINT ( 'NONE',  ( 23.44687500061451502, 6.054752690667223547, 3.707466751127219781E-16 ) ) ;
#43918 = CARTESIAN_POINT ( 'NONE',  ( 14.29687500061451821, -3.027376345333610441, -5.243569643749999898 ) ) ;
#43919 = CYLINDRICAL_SURFACE ( 'NONE', #4182, 4.000000000000000000 ) ;
#43920 = ORIENTED_EDGE ( 'NONE', *, *, #15421, .F. ) ;
#43921 = CARTESIAN_POINT ( 'NONE',  ( 18.14062500061451644, -3.027376345333614438, 5.243569643749998122 ) ) ;
#43922 = CARTESIAN_POINT ( 'NONE',  ( 28.61250000122903359, 4.330127018922192761, -2.499999999999997780 ) ) ;
#43923 = CARTESIAN_POINT ( 'NONE',  ( 15.08437500061451786, -4.541064518000419881, 2.621784821874995952 ) ) ;
#43924 = CARTESIAN_POINT ( 'NONE',  ( 2.803125000614518747, 0.000000000000000000, 5.243569643749999010 ) ) ;
#43925 = CARTESIAN_POINT ( 'NONE',  ( 20.57812500061451644, 6.421520780324663323E-16, -5.243569643749999010 ) ) ;
#43926 = CARTESIAN_POINT ( 'NONE',  ( 1.071796769724497445, 16.71740381056766367, -33.99999999999998579 ) ) ;
#43927 = CARTESIAN_POINT ( 'NONE',  ( 29.37187500061451928, 3.027376345333611329, 5.243569643749999010 ) ) ;
#43928 = CARTESIAN_POINT ( 'NONE',  ( -4.243569643749997233, 13.99062500061451786, 32.45002607614398471 ) ) ;
#43929 = CARTESIAN_POINT ( 'NONE',  ( 16.50937500061451502, -4.541064518000417216, -2.621784821875001281 ) ) ;
#43930 = CARTESIAN_POINT ( 'NONE',  ( 14.43750000122903288, -4.330127018922194537, 2.499999999999995559 ) ) ;
#43931 = CARTESIAN_POINT ( 'NONE',  ( 10.39687500061451786, 5.492252693125287522, 3.363034840372157021E-16 ) ) ;
#43932 = CARTESIAN_POINT ( 'NONE',  ( -4.243569643749999898, 19.85937500061451644, -30.00000000000000000 ) ) ;
#43933 = CARTESIAN_POINT ( 'NONE',  ( 20.89687500061452141, -3.027376345333614438, 5.243569643749998122 ) ) ;
#43934 = CARTESIAN_POINT ( 'NONE',  ( 23.62500000122902932, 2.886751345948129099, -4.999999999999998224 ) ) ;
#43935 = EDGE_CURVE ( 'NONE', #36605, #33656, #11562, .T. ) ;
#43936 =( BOUNDED_CURVE ( )  B_SPLINE_CURVE ( 2, ( #52880, #24433, #53239, #46982, #48073, #2278, #2636 ),
 .UNSPECIFIED., .F., .F. ) 
 B_SPLINE_CURVE_WITH_KNOTS ( ( 3, 2, 2, 3 ),
 ( 0.6583333333333334370, 0.6611111111111112049, 0.6638888888888888618, 0.6666666666666666297 ),
 .UNSPECIFIED. ) 
 CURVE ( )  GEOMETRIC_REPRESENTATION_ITEM ( )  RATIONAL_B_SPLINE_CURVE ( ( 0.9999999999999946709, 0.8660254037844440367, 1.000000000000000000, 0.8660254037844387076, 1.000000000000000000, 0.8660254037844387076, 1.000000000000000000 ) ) 
 REPRESENTATION_ITEM ( '' )  );
#43937 = CARTESIAN_POINT ( 'NONE',  ( 17.18437500061451573, 4.541064518000418104, 2.621784821874999949 ) ) ;
#43938 = CARTESIAN_POINT ( 'NONE',  ( 12.21562500061451573, 3.027376345333611329, 5.243569643749999010 ) ) ;
#43939 = CARTESIAN_POINT ( 'NONE',  ( -2.121784821874996840, 11.83437500061451786, 33.67503911421598417 ) ) ;
#43940 = CARTESIAN_POINT ( 'NONE',  ( 17.72812500061451502, -4.541064518000419881, 2.621784821874995952 ) ) ;
#43941 = ORIENTED_EDGE ( 'NONE', *, *, #32035, .T. ) ;
#43942 = ORIENTED_EDGE ( 'NONE', *, *, #31318, .F. ) ;
#43943 = CARTESIAN_POINT ( 'NONE',  ( 24.14999999999999858, 0.000000000000000000, 4.999999999999998224 ) ) ;
#43944 = CARTESIAN_POINT ( 'NONE',  ( -4.243569643749999898, 18.95937500061451431, -30.00000000000000000 ) ) ;
#43945 = DIRECTION ( 'NONE',  ( 0.000000000000000000, 0.000000000000000000, 1.000000000000000000 ) ) ;
#43946 = CARTESIAN_POINT ( 'NONE',  ( 24.55312500061451786, -4.541064518000417216, -2.621784821875001281 ) ) ;
#43947 = CARTESIAN_POINT ( 'NONE',  ( 6.140625000614516438, -3.027376345333610441, -5.243569643749999898 ) ) ;
#43948 = CARTESIAN_POINT ( 'NONE',  ( 17.40000000122903145, 5.773502691896255534, 3.535250795749688894E-16 ) ) ;
#43949 = CARTESIAN_POINT ( 'NONE',  ( 22.56562500061451715, 3.027376345333611329, 5.243569643749999010 ) ) ;
#43950 = CARTESIAN_POINT ( 'NONE',  ( 22.80000000000000071, 0.000000000000000000, 4.999999999999998224 ) ) ;
#43951 = CARTESIAN_POINT ( 'NONE',  ( 25.11562500061451431, 3.027376345333613106, -5.243569643749998122 ) ) ;
#43952 = CARTESIAN_POINT ( 'NONE',  ( 6.440625000614517148, -3.027376345333614438, 5.243569643749998122 ) ) ;
#43953 = VERTEX_POINT ( 'NONE', #17797 ) ;
#43954 = VECTOR ( 'NONE', #9978, 1000.000000000000000 ) ;
#43955 = CARTESIAN_POINT ( 'NONE',  ( 24.32812500061451289, 4.541064518000418104, 2.621784821874999949 ) ) ;
#43956 = CARTESIAN_POINT ( 'NONE',  ( -3.486133158594716510E-16, 13.00624999877096855, 26.00000000000000355 ) ) ;
#43957 =( BOUNDED_CURVE ( )  B_SPLINE_CURVE ( 2, ( #23202, #1059, #56817, #38112, #61010, #51657, #27045 ),
 .UNSPECIFIED., .F., .F. ) 
 B_SPLINE_CURVE_WITH_KNOTS ( ( 3, 2, 2, 3 ),
 ( 0.1666666666666666852, 0.1694444444444444808, 0.1722222222222222487, 0.1750000000000000167 ),
 .UNSPECIFIED. ) 
 CURVE ( )  GEOMETRIC_REPRESENTATION_ITEM ( )  RATIONAL_B_SPLINE_CURVE ( ( 0.9999999999999986677, 0.8660254037844400399, 1.000000000000000000, 0.8660254037844387076, 1.000000000000000000, 0.8660254037844373753, 1.000000000000001332 ) ) 
 REPRESENTATION_ITEM ( '' )  );
#43958 = CARTESIAN_POINT ( 'NONE',  ( 12.53437500061451537, 5.824947211148865298E-16, -4.756430356249998326 ) ) ;
#43959 = CARTESIAN_POINT ( 'NONE',  ( 30.00000000000000000, 0.000000000000000000, 0.000000000000000000 ) ) ;
#43960 = CARTESIAN_POINT ( 'NONE',  ( 8.484601909799253346E-16, 14.82500000122903216, -25.38119784648299770 ) ) ;
#43961 = CARTESIAN_POINT ( 'NONE',  ( 4.243569643749999010, 19.67187500061451644, -32.45002607614398471 ) ) ;
#43962 = CARTESIAN_POINT ( 'NONE',  ( 10.61250000000000071, 2.886751345948126879, 4.999999999999999112 ) ) ;
#43963 = CARTESIAN_POINT ( 'NONE',  ( 12.00937500061451857, -4.541064518000417216, -2.621784821875001281 ) ) ;
#43964 = CARTESIAN_POINT ( 'NONE',  ( 7.200000001229035718, -2.886751345948129988, 4.999999999999997335 ) ) ;
#43965 = CARTESIAN_POINT ( 'NONE',  ( 14.40937500061451715, 4.541064518000418104, -2.621784821874998173 ) ) ;
#43966 = CARTESIAN_POINT ( 'NONE',  ( 5.784375000614517148, 6.421520780324663323E-16, -5.243569643749999010 ) ) ;
#43967 = DIRECTION ( 'NONE',  ( -1.000000000000000000, -0.000000000000000000, -0.000000000000000000 ) ) ;
#43968 = CARTESIAN_POINT ( 'NONE',  ( -2.000000000000000000, 10.58750000122903323, 26.53589838486224650 ) ) ;
#43969 = CARTESIAN_POINT ( 'NONE',  ( 12.60937500061451821, 4.541064518000418104, -2.621784821874998173 ) ) ;
#43970 = LINE ( 'NONE', #9976, #61862 ) ;
#43971 = CARTESIAN_POINT ( 'NONE',  ( 22.79062500061451502, -3.027376345333610441, -5.243569643749999898 ) ) ;
#43972 = CARTESIAN_POINT ( 'NONE',  ( 0.000000000000000000, 27.50000000000000000, 30.00000000000000000 ) ) ;
#43973 = CARTESIAN_POINT ( 'NONE',  ( 29.66250000122903074, 0.000000000000000000, 4.999999999999998224 ) ) ;
#43974 = CARTESIAN_POINT ( 'NONE',  ( 24.83437500061451431, 4.541064518000418104, 2.621784821874999949 ) ) ;
#43975 = CARTESIAN_POINT ( 'NONE',  ( 3.999999999999998668, 19.36249999999999716, 27.69059892324149530 ) ) ;
#43976 = CARTESIAN_POINT ( 'NONE',  ( 29.36250000122903003, -4.330127018922190985, -2.500000000000001332 ) ) ;
#43977 = CARTESIAN_POINT ( 'NONE',  ( 19.77187500061451786, 4.119189519843966529, 2.378215178124999607 ) ) ;
#43978 = CARTESIAN_POINT ( 'NONE',  ( 24.17812500061451786, 6.421520780324663323E-16, -5.243569643749999010 ) ) ;
#43979 = CARTESIAN_POINT ( 'NONE',  ( 17.76562500061451644, -6.054752690667223547, -1.112240025338166033E-15 ) ) ;
#43980 = CARTESIAN_POINT ( 'NONE',  ( 14.68125000122903323, 4.330127018922191873, 2.499999999999999556 ) ) ;
#43981 = CARTESIAN_POINT ( 'NONE',  ( 13.95937500061451786, 4.541064518000418104, -2.621784821874998173 ) ) ;
#43982 = CARTESIAN_POINT ( 'NONE',  ( 16.76249999999999929, 2.886751345948129099, -4.999999999999997335 ) ) ;
#43983 = CARTESIAN_POINT ( 'NONE',  ( 26.96250000122903145, 0.000000000000000000, 4.999999999999998224 ) ) ;
#43984 = CARTESIAN_POINT ( 'NONE',  ( 4.629056002857023344, -1.889931353889065413, 4.891133006415133266 ) ) ;
#43985 = CARTESIAN_POINT ( 'NONE',  ( 13.28437500061451715, -4.541064518000419881, 2.621784821874995952 ) ) ;
#43986 = CARTESIAN_POINT ( 'NONE',  ( 2.000000000000000444, 17.91874999877096641, 26.53589838486224650 ) ) ;
#43987 = CARTESIAN_POINT ( 'NONE',  ( -2.000000000000000000, 11.37500000000000178, 26.53589838486224650 ) ) ;
#43988 = CARTESIAN_POINT ( 'NONE',  ( 3.825000001229032609, 2.886751345948129099, -4.999999999999998224 ) ) ;
#43989 = CARTESIAN_POINT ( 'NONE',  ( 25.28437500061451715, 4.541064518000418104, 2.621784821874999949 ) ) ;
#43990 = CARTESIAN_POINT ( 'NONE',  ( 16.99687500061451573, -3.027376345333610441, -5.243569643749999898 ) ) ;
#43991 = CARTESIAN_POINT ( 'NONE',  ( 3.756430356250000102, 15.00312499938548427, 30.00000000000000000 ) ) ;
#43992 = CARTESIAN_POINT ( 'NONE',  ( 28.49999999999999645, 4.330127018922192761, -2.499999999999997780 ) ) ;
#43993 = CARTESIAN_POINT ( 'NONE',  ( 6.487499999999999822, 5.773502691896255534, 3.535250795749688894E-16 ) ) ;
#43994 = CARTESIAN_POINT ( 'NONE',  ( 29.67187500061451644, 2.746126346562645981, -4.756430356249997438 ) ) ;
#43995 = CARTESIAN_POINT ( 'NONE',  ( 20.72812500061451502, 4.541064518000418104, 2.621784821874999949 ) ) ;
#43996 = CARTESIAN_POINT ( 'NONE',  ( 9.412499999999999645, -5.773502691896255534, -1.060575238724906372E-15 ) ) ;
#43997 = CARTESIAN_POINT ( 'NONE',  ( 4.490625000614516971, 6.054752690667223547, 3.707466751127219781E-16 ) ) ;
#43998 = CARTESIAN_POINT ( 'NONE',  ( 20.36249999999999716, 2.886751345948129099, -4.999999999999998224 ) ) ;
#43999 = CARTESIAN_POINT ( 'NONE',  ( 19.20000000000000284, 0.000000000000000000, 4.999999999999998224 ) ) ;
#44000 = CARTESIAN_POINT ( 'NONE',  ( 24.30000000122903359, -2.886751345948129988, 4.999999999999997335 ) ) ;
#44001 = DIRECTION ( 'NONE',  ( 0.000000000000000000, 0.000000000000000000, 1.000000000000000000 ) ) ;
#44002 = CARTESIAN_POINT ( 'NONE',  ( 3.825000000000001954, 4.330127018922191873, 2.499999999999999556 ) ) ;
#44003 = EDGE_LOOP ( 'NONE', ( #40163, #71832, #46173, #62322 ) ) ;
#44004 = CARTESIAN_POINT ( 'NONE',  ( 18.06562500061451715, 3.027376345333611329, 5.243569643749999010 ) ) ;
#44005 = CARTESIAN_POINT ( 'NONE',  ( 24.66562500061451502, 3.027376345333613106, -5.243569643749998122 ) ) ;
#44006 = CARTESIAN_POINT ( 'NONE',  ( 25.43437500061451573, -4.541064518000419881, 2.621784821874995952 ) ) ;
#44007 = CARTESIAN_POINT ( 'NONE',  ( 7.650000000000000355, -4.330127018922190985, -2.500000000000001332 ) ) ;
#44008 = CARTESIAN_POINT ( 'NONE',  ( 9.515625000614518214, 3.027376345333611329, 5.243569643749999010 ) ) ;
#44009 = CARTESIAN_POINT ( 'NONE',  ( 27.14062500061451644, -3.027376345333614438, 5.243569643749998122 ) ) ;
#44010 = CARTESIAN_POINT ( 'NONE',  ( 14.55937500061451573, 0.000000000000000000, 5.243569643749999010 ) ) ;
#44011 = CARTESIAN_POINT ( 'NONE',  ( 18.79687500061451644, -3.027376345333610441, -5.243569643749999898 ) ) ;
#44012 = CARTESIAN_POINT ( 'NONE',  ( 4.450256264752916024, 2.279367318176788615, -4.722266026914592629 ) ) ;
#44013 = CARTESIAN_POINT ( 'NONE',  ( -2.121784821874996840, 10.03437500061451892, 33.67503911421598417 ) ) ;
#44014 = CARTESIAN_POINT ( 'NONE',  ( 21.26250000122903572, -4.330127018922190985, -2.500000000000001332 ) ) ;
#44015 = CARTESIAN_POINT ( 'NONE',  ( 16.62187500061451573, 2.746126346562645981, -4.756430356249997438 ) ) ;
#44016 = CARTESIAN_POINT ( 'NONE',  ( 11.31562500061451892, 3.027376345333611329, 5.243569643749999010 ) ) ;
#44017 = CARTESIAN_POINT ( 'NONE',  ( 8.259375000614518569, 0.000000000000000000, 5.243569643749999010 ) ) ;
#44018 = CARTESIAN_POINT ( 'NONE',  ( 7.696875000614516793, 6.054752690667223547, 3.707466751127219781E-16 ) ) ;
#44019 = ORIENTED_EDGE ( 'NONE', *, *, #71436, .T. ) ;
#44020 = CARTESIAN_POINT ( 'NONE',  ( 26.67187500061451644, 3.027376345333611329, 5.243569643749999010 ) ) ;
#44021 = CARTESIAN_POINT ( 'NONE',  ( 18.62812500061451715, -4.541064518000419881, 2.621784821874995952 ) ) ;
#44022 = CARTESIAN_POINT ( 'NONE',  ( 28.76250000122903216, 0.000000000000000000, 4.999999999999998224 ) ) ;
#44023 = ADVANCED_FACE ( 'NONE', ( #28548 ), #40357, .F. ) ;
#44024 = CARTESIAN_POINT ( 'NONE',  ( 29.20312500061451644, 4.541064518000418104, -2.621784821874998173 ) ) ;
#44025 = CARTESIAN_POINT ( 'NONE',  ( 23.48437500061451644, 4.541064518000418104, 2.621784821874999949 ) ) ;
#44026 = CARTESIAN_POINT ( 'NONE',  ( 20.57812500061451644, 6.421520780324663323E-16, -5.243569643749999010 ) ) ;
#44027 = CARTESIAN_POINT ( 'NONE',  ( 8.484601909799253346E-16, 12.91249999999999964, 34.61880215351700230 ) ) ;
#44028 = CARTESIAN_POINT ( 'NONE',  ( 23.80312500061451786, 4.541064518000418104, -2.621784821874998173 ) ) ;
#44029 = CARTESIAN_POINT ( 'NONE',  ( 4.687500001229034652, 6.123233995736764310E-16, -4.999999999999998224 ) ) ;
#44030 = ORIENTED_EDGE ( 'NONE', *, *, #36869, .F. ) ;
#44031 = CARTESIAN_POINT ( 'NONE',  ( 29.17500000000000071, -4.330127018922194537, 2.499999999999995559 ) ) ;
#44032 = CARTESIAN_POINT ( 'NONE',  ( -3.999999999999999556, 15.01250000000000107, -32.30940107675850470 ) ) ;
#44033 = CARTESIAN_POINT ( 'NONE',  ( -3.756430356250001434, 14.81562499938548250, 32.16877607737301048 ) ) ;
#44034 = CARTESIAN_POINT ( 'NONE',  ( 4.434375000614519280, 6.421520780324663323E-16, -5.243569643749999010 ) ) ;
#44035 = CARTESIAN_POINT ( 'NONE',  ( 29.24062500061451431, 6.054752690667223547, 3.707466751127219781E-16 ) ) ;
#44036 = CARTESIAN_POINT ( 'NONE',  ( 12.85312500061451502, -4.541064518000417216, -2.621784821875001281 ) ) ;
#44037 = CARTESIAN_POINT ( 'NONE',  ( 5.596875000614516260, -3.027376345333614438, 5.243569643749998122 ) ) ;
#44038 = CARTESIAN_POINT ( 'NONE',  ( 24.52500000122903145, 2.886751345948129099, -4.999999999999998224 ) ) ;
#44039 = CARTESIAN_POINT ( 'NONE',  ( 15.98437500061451821, -4.541064518000419881, 2.621784821874995952 ) ) ;
#44040 = CARTESIAN_POINT ( 'NONE',  ( 28.67812500061451431, 6.421520780324663323E-16, -5.243569643749999010 ) ) ;
#44041 = CARTESIAN_POINT ( 'NONE',  ( -3.999999999999999112, 10.96250000000000213, 27.69059892324149885 ) ) ;
#44042 = CARTESIAN_POINT ( 'NONE',  ( 26.97187500061451360, 3.027376345333613106, -5.243569643749998122 ) ) ;
#44043 = CARTESIAN_POINT ( 'NONE',  ( 3.740625000614516527, -3.027376345333614438, 5.243569643749998122 ) ) ;
#44044 = CARTESIAN_POINT ( 'NONE',  ( 13.15312500061451750, 0.000000000000000000, 5.243569643749999010 ) ) ;
#44045 = VERTEX_POINT ( 'NONE', #16725 ) ;
#44046 = CARTESIAN_POINT ( 'NONE',  ( 9.478125000614515017, 4.541064518000418104, 2.621784821874999949 ) ) ;
#44047 = CARTESIAN_POINT ( 'NONE',  ( 7.640625000614517326, 6.054752690667223547, 3.707466751127219781E-16 ) ) ;
#44048 = CARTESIAN_POINT ( 'NONE',  ( 19.62187500061451573, -5.492252693125287522, -1.008910452111647106E-15 ) ) ;
#44049 = CARTESIAN_POINT ( 'NONE',  ( 9.562500000000001776, 2.886751345948129099, -4.999999999999998224 ) ) ;
#44050 = CARTESIAN_POINT ( 'NONE',  ( 4.275000001229035895, 2.886751345948129099, -4.999999999999998224 ) ) ;
#44051 = CARTESIAN_POINT ( 'NONE',  ( 17.88749999999999929, -2.886751345948129988, 4.999999999999997335 ) ) ;
#44052 = CARTESIAN_POINT ( 'NONE',  ( 18.57187500061451857, 3.027376345333611329, 5.243569643749999010 ) ) ;
#44053 = CARTESIAN_POINT ( 'NONE',  ( 13.53750000122903430, -4.330127018922194537, 2.499999999999995559 ) ) ;
#44054 = CARTESIAN_POINT ( 'NONE',  ( 20.73750000000000071, -2.886751345948125991, -5.000000000000000000 ) ) ;
#44055 = CARTESIAN_POINT ( 'NONE',  ( -2.121784821874999949, 17.47812500061451502, -33.67503911421598417 ) ) ;
#44056 = CARTESIAN_POINT ( 'NONE',  ( 20.58749999999999858, -2.886751345948074920, 5.000000000000092371 ) ) ;
#44057 = CARTESIAN_POINT ( 'NONE',  ( 20.78732959644809952, -2.499999999999999556, -3.499999999999999556 ) ) ;
#44058 = CARTESIAN_POINT ( 'NONE',  ( 28.49062500061451431, -3.027376345333614438, 5.243569643749998122 ) ) ;
#44059 = DIRECTION ( 'NONE',  ( -1.000000000000000000, -0.000000000000000000, -0.000000000000000000 ) ) ;
#44060 = CARTESIAN_POINT ( 'NONE',  ( 12.83437500061451786, -4.541064518000419881, 2.621784821874995952 ) ) ;
#44061 = CARTESIAN_POINT ( 'NONE',  ( 26.39999999999999858, 0.000000000000000000, 4.999999999999998224 ) ) ;
#44062 = EDGE_CURVE ( 'NONE', #27832, #48021, #62876, .T. ) ;
#44063 = CARTESIAN_POINT ( 'NONE',  ( 10.45312500061451644, 0.000000000000000000, 5.243569643749999010 ) ) ;
#44064 = CARTESIAN_POINT ( 'NONE',  ( 26.82187500061451502, 5.824947211148865298E-16, -4.756430356249998326 ) ) ;
#44065 = CARTESIAN_POINT ( 'NONE',  ( 21.94687500061451857, -3.027376345333610441, -5.243569643749999898 ) ) ;
#44066 = CARTESIAN_POINT ( 'NONE',  ( 12.72187500061451537, -4.119189519843968306, 2.378215178124996054 ) ) ;
#44067 = ADVANCED_FACE ( 'NONE', ( #27836 ), #55765, .T. ) ;
#44068 = CARTESIAN_POINT ( 'NONE',  ( 7.378125000614518036, -4.541064518000419881, 2.621784821874995952 ) ) ;
#44069 = CARTESIAN_POINT ( 'NONE',  ( 12.79687500061451821, -3.027376345333614438, 5.243569643749998122 ) ) ;
#44070 = ORIENTED_EDGE ( 'NONE', *, *, #16880, .T. ) ;
#44071 = CARTESIAN_POINT ( 'NONE',  ( 24.49687500061451573, -3.027376345333614438, 5.243569643749998122 ) ) ;
#44072 = CARTESIAN_POINT ( 'NONE',  ( 0.2791130135581331162, 5.000000000000003553, -34.00000000000001421 ) ) ;
#44073 = CARTESIAN_POINT ( 'NONE',  ( 8.812500000000000000, 2.886751345948193936, 4.999999999999883649 ) ) ;
#44074 = CARTESIAN_POINT ( 'NONE',  ( 4.462500000000001243, -5.773502691896255534, -1.060575238724906372E-15 ) ) ;
#44075 = CARTESIAN_POINT ( 'NONE',  ( 14.25000000122903465, 5.773502691896255534, 3.535250795749688894E-16 ) ) ;
#44076 = CARTESIAN_POINT ( 'NONE',  ( 20.60625000122902861, 0.000000000000000000, 4.999999999999998224 ) ) ;
#44077 = CARTESIAN_POINT ( 'NONE',  ( 17.28750000000000142, 5.773502691896255534, 3.535250795749688401E-16 ) ) ;
#44078 = ORIENTED_EDGE ( 'NONE', *, *, #44436, .F. ) ;
#44079 = CARTESIAN_POINT ( 'NONE',  ( 13.95000000000000107, -4.330127018922190985, -2.500000000000001332 ) ) ;
#44080 = CARTESIAN_POINT ( 'NONE',  ( 15.56250000000000000, 2.886751345948126879, 4.999999999999999112 ) ) ;
#44081 = ADVANCED_FACE ( 'NONE', ( #11094 ), #72795, .T. ) ;
#44082 = CARTESIAN_POINT ( 'NONE',  ( 12.75000000122903643, -2.886751345948125991, -5.000000000000000000 ) ) ;
#44083 = CARTESIAN_POINT ( 'NONE',  ( 12.47812500061451502, 6.421520780324663323E-16, -5.243569643749999010 ) ) ;
#44084 = VERTEX_POINT ( 'NONE', #45446 ) ;
#44085 = CARTESIAN_POINT ( 'NONE',  ( 8.437500000000000000, -2.886751345948129988, 4.999999999999997335 ) ) ;
#44086 = CARTESIAN_POINT ( 'NONE',  ( -1.487416814333745711E-14, 15.72500000122903430, 34.00000000000000000 ) ) ;
#44087 = CARTESIAN_POINT ( 'NONE',  ( 4.243569643749999898, 14.64687500061451964, -27.54997392385601529 ) ) ;
#44088 = CARTESIAN_POINT ( 'NONE',  ( 3.628125000614518036, 4.541064518000418104, 2.621784821874999949 ) ) ;
#44089 = CARTESIAN_POINT ( 'NONE',  ( 1.878215178124997609, 15.26562499938548179, 33.25316411605952993 ) ) ;
#44090 = CARTESIAN_POINT ( 'NONE',  ( 9.000000000000001776, -4.330127018922190985, -2.500000000000001332 ) ) ;
#44091 = CARTESIAN_POINT ( 'NONE',  ( 3.837848076843223932, 3.204827942194517387, -3.837848076843223932 ) ) ;
#44092 = ORIENTED_EDGE ( 'NONE', *, *, #10704, .F. ) ;
#44093 = CARTESIAN_POINT ( 'NONE',  ( 25.19062500061451715, 6.054752690667223547, 3.707466751127219781E-16 ) ) ;
#44094 = CARTESIAN_POINT ( 'NONE',  ( 29.43750000122903288, 6.123233995736764310E-16, -4.999999999999998224 ) ) ;
#44095 = CARTESIAN_POINT ( 'NONE',  ( -1.878215178124999163, 19.54062499938548214, 26.74683588394047007 ) ) ;
#44096 = CARTESIAN_POINT ( 'NONE',  ( 22.09687500061451715, 6.054752690667223547, 3.707466751127219781E-16 ) ) ;
#44097 = EDGE_CURVE ( 'NONE', #65143, #67926, #52938, .T. ) ;
#44098 = CARTESIAN_POINT ( 'NONE',  ( 19.37812500061451715, 4.541064518000418104, 2.621784821874999949 ) ) ;
#44099 = CARTESIAN_POINT ( 'NONE',  ( 4.243569643749999010, 11.06562500061459353, -32.45002607614398471 ) ) ;
#44100 = CARTESIAN_POINT ( 'NONE',  ( 7.153125000614518392, 4.541064518000418104, -2.621784821874998173 ) ) ;
#44101 = CARTESIAN_POINT ( 'NONE',  ( 3.365625000614516082, -6.054752690667223547, -1.112240025338166033E-15 ) ) ;
#44102 = CARTESIAN_POINT ( 'NONE',  ( 23.59687500061451715, -2.746126346562646425, 4.756430356249996549 ) ) ;
#44103 = CARTESIAN_POINT ( 'NONE',  ( 20.57812500061451644, 6.421520780324663323E-16, -5.243569643749999010 ) ) ;
#44104 = CARTESIAN_POINT ( 'NONE',  ( 8.446875000614518569, -2.746126346562642428, -4.756430356249999214 ) ) ;
#44105 = CARTESIAN_POINT ( 'NONE',  ( -3.756430356250001434, 17.40312499938548285, 32.16877607737301048 ) ) ;
#44106 = CARTESIAN_POINT ( 'NONE',  ( 16.24687500061451573, 6.054752690667223547, 3.707466751127219781E-16 ) ) ;
#44107 = CARTESIAN_POINT ( 'NONE',  ( 14.25937500061451679, -4.541064518000417216, -2.621784821875001281 ) ) ;
#44108 = CARTESIAN_POINT ( 'NONE',  ( 22.05937500061451573, 4.541064518000418104, -2.621784821874998173 ) ) ;
#44109 = ORIENTED_EDGE ( 'NONE', *, *, #44978, .F. ) ;
#44110 = CARTESIAN_POINT ( 'NONE',  ( 2.121784821874999061, 12.95937500061451786, 26.32496088578401583 ) ) ;
#44111 = CARTESIAN_POINT ( 'NONE',  ( 20.02500000000000213, 4.330127018922191873, 2.499999999999999556 ) ) ;
#44112 = CARTESIAN_POINT ( 'NONE',  ( 26.01562500061451289, 3.027376345333613106, -5.243569643749998122 ) ) ;
#44113 = CARTESIAN_POINT ( 'NONE',  ( 26.09062500061451573, 6.054752690667223547, 3.707466751127219781E-16 ) ) ;
#44114 = DIRECTION ( 'NONE',  ( 0.000000000000000000, 0.7071067811865535679, 0.7071067811865414665 ) ) ;
#44115 = CARTESIAN_POINT ( 'NONE',  ( 2.000000000000001332, 18.35000000000000142, 33.46410161513774995 ) ) ;
#44116 = CARTESIAN_POINT ( 'NONE',  ( 5.859375000614519102, 4.541064518000418104, -2.621784821874998173 ) ) ;
#44117 = ITEM_DEFINED_TRANSFORMATION ( 'NONE', 'NONE', #22614,  #23765 ) ;
#44118 = CARTESIAN_POINT ( 'NONE',  ( 12.41250000122903430, 4.330127018922192761, -2.499999999999997780 ) ) ;
#44119 = CARTESIAN_POINT ( 'NONE',  ( 9.412500001229034297, 0.000000000000000000, 4.999999999999998224 ) ) ;
#44120 = CARTESIAN_POINT ( 'NONE',  ( 28.87500000122902932, -5.773502691896255534, -1.060575238724906372E-15 ) ) ;
#44121 = CARTESIAN_POINT ( 'NONE',  ( 4.000000000000000000, 16.98124999877096641, 27.69059892324149530 ) ) ;
#44122 = CARTESIAN_POINT ( 'NONE',  ( 18.09375000122903288, -2.886751345948125991, -5.000000000000000000 ) ) ;
#44123 = CARTESIAN_POINT ( 'NONE',  ( 10.92187500061451644, 3.027376345333611329, 5.243569643749999010 ) ) ;
#44124 = FACE_OUTER_BOUND ( 'NONE', #19101, .T. ) ;
#44125 = EDGE_LOOP ( 'NONE', ( #28004, #69892, #64312, #22082 ) ) ;
#44126 = CARTESIAN_POINT ( 'NONE',  ( 18.66562500061451146, -6.054752690667223547, -1.112240025338166033E-15 ) ) ;
#44127 = CARTESIAN_POINT ( 'NONE',  ( 12.68437500061451573, 4.541064518000418104, 2.621784821874999949 ) ) ;
#44128 = CARTESIAN_POINT ( 'NONE',  ( 4.040625000614517681, 6.054752690667223547, 3.707466751127219781E-16 ) ) ;
#44129 = CARTESIAN_POINT ( 'NONE',  ( 21.83437500061451786, -4.541064518000419881, 2.621784821874995952 ) ) ;
#44130 = CARTESIAN_POINT ( 'NONE',  ( 6.065625000614516260, -6.054752690667223547, -1.112240025338166033E-15 ) ) ;
#44131 = DIRECTION ( 'NONE',  ( -1.000000000000000000, -0.000000000000000000, -0.000000000000000000 ) ) ;
#44132 = CARTESIAN_POINT ( 'NONE',  ( 6.787500001229032520, -4.330127018922194537, 2.499999999999995559 ) ) ;
#44133 = CARTESIAN_POINT ( 'NONE',  ( 21.55312500061451431, 4.541064518000418104, -2.621784821874998173 ) ) ;
#44134 = CARTESIAN_POINT ( 'NONE',  ( -3.999999999999999112, 16.96250000122903145, -30.00000000000000000 ) ) ;
#44135 = CARTESIAN_POINT ( 'NONE',  ( 8.025000001229035007, 2.886751345948126879, 4.999999999999999112 ) ) ;
#44136 = CARTESIAN_POINT ( 'NONE',  ( 16.45312500061451289, -4.541064518000417216, -2.621784821875001281 ) ) ;
#44137 = CARTESIAN_POINT ( 'NONE',  ( 15.40312500061451573, 0.000000000000000000, 5.243569643749999010 ) ) ;
#44138 = CARTESIAN_POINT ( 'NONE',  ( 26.44687500061451502, -2.746126346562642428, -4.756430356249999214 ) ) ;
#44139 = CARTESIAN_POINT ( 'NONE',  ( 15.71250000000000213, -5.773502691896255534, -1.060575238724906372E-15 ) ) ;
#44140 = CARTESIAN_POINT ( 'NONE',  ( 12.52500000122903145, 2.886751345948126879, 4.999999999999999112 ) ) ;
#44141 = CARTESIAN_POINT ( 'NONE',  ( 7.303125000614516082, 0.000000000000000000, 5.243569643749999010 ) ) ;
#44142 = CARTESIAN_POINT ( 'NONE',  ( 10.45312500061451644, 0.000000000000000000, 5.243569643749999010 ) ) ;
#44143 =( BOUNDED_CURVE ( )  B_SPLINE_CURVE ( 2, ( #15072, #37609, #8806, #37247, #42431, #64952, #14344 ),
 .UNSPECIFIED., .F., .F. ) 
 B_SPLINE_CURVE_WITH_KNOTS ( ( 3, 2, 2, 3 ),
 ( 0.6400000000000001243, 0.6433333333333334236, 0.6466666666666666119, 0.6500000000000000222 ),
 .UNSPECIFIED. ) 
 CURVE ( )  GEOMETRIC_REPRESENTATION_ITEM ( )  RATIONAL_B_SPLINE_CURVE ( ( 0.9999999999999955591, 0.8660254037844431485, 1.000000000000000000, 0.8660254037844387076, 1.000000000000000000, 0.8660254037844387076, 1.000000000000000000 ) ) 
 REPRESENTATION_ITEM ( '' )  );
#44144 = CARTESIAN_POINT ( 'NONE',  ( 19.72500000122903074, 2.886751345948126879, 4.999999999999999112 ) ) ;
#44145 = CARTESIAN_POINT ( 'NONE',  ( -4.243569643749997233, 12.69687500061451857, -27.54997392385601174 ) ) ;
#44146 = CARTESIAN_POINT ( 'NONE',  ( 18.87187500061451573, 3.027376345333613106, -5.243569643749998122 ) ) ;
#44147 = CARTESIAN_POINT ( 'NONE',  ( 9.899999999999998579, -4.330127018922190985, -2.500000000000001332 ) ) ;
#44148 = CARTESIAN_POINT ( 'NONE',  ( 5.812500001229035540, 0.000000000000000000, 4.999999999999998224 ) ) ;
#44149 = CARTESIAN_POINT ( 'NONE',  ( 3.084375000614519191, 6.421520780324663323E-16, -5.243569643749999010 ) ) ;
#44150 = CARTESIAN_POINT ( 'NONE',  ( 21.12187500061451573, 3.027376345333613106, -5.243569643749998122 ) ) ;
#44151 = CARTESIAN_POINT ( 'NONE',  ( 12.33750000000000213, 5.773502691896255534, 3.535250795749688401E-16 ) ) ;
#44152 = CARTESIAN_POINT ( 'NONE',  ( 15.89062500061451289, -3.027376345333614438, 5.243569643749998122 ) ) ;
#44153 = CARTESIAN_POINT ( 'NONE',  ( 10.70625000122903536, 0.000000000000000000, 4.999999999999998224 ) ) ;
#44154 = CARTESIAN_POINT ( 'NONE',  ( -3.999999999999997335, 14.75000000122903288, 32.30940107675850470 ) ) ;
#44155 = CARTESIAN_POINT ( 'NONE',  ( 4.462500000000001243, -5.773502691896255534, -1.060575238724906372E-15 ) ) ;
#44156 = CARTESIAN_POINT ( 'NONE',  ( 29.03437500061451715, -4.541064518000419881, 2.621784821874995952 ) ) ;
#44157 = CARTESIAN_POINT ( 'NONE',  ( 20.33437500061451786, -2.746126346562646425, 4.756430356249996549 ) ) ;
#44158 = AXIS2_PLACEMENT_3D ( 'NONE', #33581, #61654, #66480 ) ;
#44159 = CARTESIAN_POINT ( 'NONE',  ( 15.17812500061451608, 6.421520780324663323E-16, -5.243569643749999010 ) ) ;
#44160 = CARTESIAN_POINT ( 'NONE',  ( 13.39687500061451608, -3.027376345333610441, -5.243569643749999898 ) ) ;
#44161 = ORIENTED_EDGE ( 'NONE', *, *, #46859, .T. ) ;
#44162 = CARTESIAN_POINT ( 'NONE',  ( 10.51875000122903181, 2.886751345948018077, -5.000000000000190070 ) ) ;
#44163 = CARTESIAN_POINT ( 'NONE',  ( 23.09062500061451573, -3.027376345333614438, 5.243569643749998122 ) ) ;
#44164 = FACE_OUTER_BOUND ( 'NONE', #49987, .T. ) ;
#44165 = CARTESIAN_POINT ( 'NONE',  ( 28.76250000122903216, 0.000000000000000000, 4.999999999999998224 ) ) ;
#44166 = CARTESIAN_POINT ( 'NONE',  ( 13.31250000000000178, 2.886751345948126879, 4.999999999999999112 ) ) ;
#44167 = CARTESIAN_POINT ( 'NONE',  ( 24.00000000122902932, -2.886751345948125991, -5.000000000000000000 ) ) ;
#44168 = CARTESIAN_POINT ( 'NONE',  ( 17.84062500061451573, -3.027376345333610441, -5.243569643749999898 ) ) ;
#44169 = VERTEX_POINT ( 'NONE', #16985 ) ;
#44170 = CARTESIAN_POINT ( 'NONE',  ( 19.94999999999999929, 4.330127018922192761, -2.499999999999997780 ) ) ;
#44171 = EDGE_CURVE ( 'NONE', #65514, #50573, #11823, .T. ) ;
#44172 = CARTESIAN_POINT ( 'NONE',  ( 21.49687500061451573, -3.027376345333610441, -5.243569643749999898 ) ) ;
#44173 = CARTESIAN_POINT ( 'NONE',  ( 28.22812500061451502, 6.421520780324663323E-16, -5.243569643749999010 ) ) ;
#44174 = ORIENTED_EDGE ( 'NONE', *, *, #32854, .T. ) ;
#44175 = CARTESIAN_POINT ( 'NONE',  ( 2.955228467731844333, 4.033190387708875946, -2.955228467731844333 ) ) ;
#44176 = CARTESIAN_POINT ( 'NONE',  ( 11.84062500061451750, -3.027376345333614438, 5.243569643749998122 ) ) ;
#44177 = CARTESIAN_POINT ( 'NONE',  ( 17.51250000122903216, 0.000000000000000000, 4.999999999999998224 ) ) ;
#44178 = CARTESIAN_POINT ( 'NONE',  ( 12.98437500061451289, 5.492252693125287522, 3.363034840372157021E-16 ) ) ;
#44179 = CARTESIAN_POINT ( 'NONE',  ( 15.93750000000000000, 5.773502691896255534, 3.535250795749688894E-16 ) ) ;
#44180 = CARTESIAN_POINT ( 'NONE',  ( 23.96249999999999858, 2.886751345948129099, -4.999999999999998224 ) ) ;
#44181 = CARTESIAN_POINT ( 'NONE',  ( -4.243569643749999898, 19.31562500061451715, 27.54997392385601529 ) ) ;
#44182 = CARTESIAN_POINT ( 'NONE',  ( 3.684375000614518836, 4.541064518000418104, 2.621784821874999949 ) ) ;
#44183 = CARTESIAN_POINT ( 'NONE',  ( 28.84687500061452070, 6.054752690667223547, 3.707466751127219781E-16 ) ) ;
#44184 = VERTEX_POINT ( 'NONE', #44732 ) ;
#44185 = CARTESIAN_POINT ( 'NONE',  ( 25.34062500061451217, -3.027376345333614438, 5.243569643749998122 ) ) ;
#44186 = CARTESIAN_POINT ( 'NONE',  ( 27.68437500061451573, -4.541064518000419881, 2.621784821874995952 ) ) ;
#44187 = CARTESIAN_POINT ( 'NONE',  ( -2.000000000000001776, 14.99374999877096570, 33.46410161513775705 ) ) ;
#44188 = CARTESIAN_POINT ( 'NONE',  ( 13.83749999999999858, -2.886751345948129988, 4.999999999999997335 ) ) ;
#44189 = CARTESIAN_POINT ( 'NONE',  ( 11.57812500061451644, 6.421520780324663323E-16, -5.243569643749999010 ) ) ;
#44190 = CARTESIAN_POINT ( 'NONE',  ( 3.748487153055565457, 3.308903755532668356, 3.979558567872137687 ) ) ;
#44191 = DIRECTION ( 'NONE',  ( -0.000000000000000000, -1.000000000000000000, -0.000000000000000000 ) ) ;
#44192 = CARTESIAN_POINT ( 'NONE',  ( 28.79062500061451502, 6.054752690667223547, 3.707466751127219781E-16 ) ) ;
#44193 = CARTESIAN_POINT ( 'NONE',  ( 15.48750000122903359, 6.123233995736764310E-16, -4.999999999999998224 ) ) ;
#44194 = CARTESIAN_POINT ( 'NONE',  ( 28.95937500061451431, -5.492252693125287522, -1.008910452111647106E-15 ) ) ;
#44195 = CARTESIAN_POINT ( 'NONE',  ( 14.33437500061451786, 5.824947211148865298E-16, -4.756430356249998326 ) ) ;
#44196 = CARTESIAN_POINT ( 'NONE',  ( 6.215625000614517504, 3.027376345333613106, -5.243569643749998122 ) ) ;
#44197 = CARTESIAN_POINT ( 'NONE',  ( 22.77187500061451786, -6.054752690667223547, -1.112240025338166033E-15 ) ) ;
#44198 = CARTESIAN_POINT ( 'NONE',  ( 4.243569643749999010, 14.27187500061451964, 27.54997392385601174 ) ) ;
#44199 = CARTESIAN_POINT ( 'NONE',  ( 21.38437500061451502, -4.541064518000419881, 2.621784821874995952 ) ) ;
#44200 = CARTESIAN_POINT ( 'NONE',  ( 28.80937500061451573, 4.541064518000418104, -2.621784821874998173 ) ) ;
#44201 = CARTESIAN_POINT ( 'NONE',  ( -3.000416591977282496E-16, 17.94687500061451502, 25.09994784771203058 ) ) ;
#44202 = CARTESIAN_POINT ( 'NONE',  ( 10.11562500061451608, -6.054752690667223547, -1.112240025338166033E-15 ) ) ;
#44203 = CARTESIAN_POINT ( 'NONE',  ( 7.320879633048903241E-15, 17.30000000122903003, 26.00000000000000355 ) ) ;
#44204 = CARTESIAN_POINT ( 'NONE',  ( 6.496875000614517504, -3.027376345333614438, 5.243569643749998122 ) ) ;
#44205 = CARTESIAN_POINT ( 'NONE',  ( 3.972658874145789110, 3.036112888163414514, -4.275165627105516286 ) ) ;
#44206 = CARTESIAN_POINT ( 'NONE',  ( 6.778125000614518392, 4.541064518000418104, 2.621784821874999949 ) ) ;
#44207 = CARTESIAN_POINT ( 'NONE',  ( 12.75937500061451857, 0.000000000000000000, 5.243569643749999010 ) ) ;
#44208 = CARTESIAN_POINT ( 'NONE',  ( -1.626862140677534273E-15, 19.13749999999999929, 34.00000000000000000 ) ) ;
#44209 = CARTESIAN_POINT ( 'NONE',  ( 21.00000000122903288, 5.773502691896255534, 3.535250795749688894E-16 ) ) ;
#44210 = CARTESIAN_POINT ( 'NONE',  ( 8.259375000614518569, 0.000000000000000000, 5.243569643749999010 ) ) ;
#44211 = CARTESIAN_POINT ( 'NONE',  ( 10.60312500061451679, -4.541064518000417216, -2.621784821875001281 ) ) ;
#44212 = CARTESIAN_POINT ( 'NONE',  ( 6.928125000614516082, -4.541064518000419881, 2.621784821874995952 ) ) ;
#44213 = CARTESIAN_POINT ( 'NONE',  ( 25.03125000122903288, 4.330127018922191873, 2.499999999999999556 ) ) ;
#44214 = CARTESIAN_POINT ( 'NONE',  ( 20.18437500061451573, 6.421520780324663323E-16, -5.243569643749999010 ) ) ;
#44215 = CARTESIAN_POINT ( 'NONE',  ( 18.18750000000000355, 5.773502691896255534, 3.535250795749688401E-16 ) ) ;
#44216 = CARTESIAN_POINT ( 'NONE',  ( 11.57812500061451644, 6.421520780324663323E-16, -5.243569643749999010 ) ) ;
#44217 = EDGE_CURVE ( 'NONE', #46571, #51638, #18405, .T. ) ;
#44218 = CARTESIAN_POINT ( 'NONE',  ( 4.243569643749999898, 12.84687500061451715, -27.54997392385601529 ) ) ;
#44219 = CARTESIAN_POINT ( 'NONE',  ( 14.17500000122903536, 2.886751345948129099, -4.999999999999998224 ) ) ;
#44220 = CARTESIAN_POINT ( 'NONE',  ( -2.121784821874999949, 14.32812500061451644, -33.67503911421598417 ) ) ;
#44221 = CARTESIAN_POINT ( 'NONE',  ( 15.63750000122903216, 4.330127018922191873, 2.499999999999999556 ) ) ;
#44222 = CARTESIAN_POINT ( 'NONE',  ( 10.64062500061451644, -3.027376345333610441, -5.243569643749999898 ) ) ;
#44223 = VERTEX_POINT ( 'NONE', #11461 ) ;
#44224 = CARTESIAN_POINT ( 'NONE',  ( 13.57500000000000107, 6.123233995736764310E-16, -4.999999999999998224 ) ) ;
#44225 = CARTESIAN_POINT ( 'NONE',  ( -0.6945881563830144101, 20.00000000000000000, 26.06076818491061076 ) ) ;
#44226 = CARTESIAN_POINT ( 'NONE',  ( 23.84062500061451928, 6.054752690667223547, 3.707466751127219781E-16 ) ) ;
#44227 = CARTESIAN_POINT ( 'NONE',  ( 7.059375000614518392, -4.541064518000417216, -2.621784821875001281 ) ) ;
#44228 = ADVANCED_FACE ( 'NONE', ( #33622 ), #56874, .F. ) ;
#44229 = CARTESIAN_POINT ( 'NONE',  ( 10.23750000122903359, 4.330127018922191873, 2.499999999999999556 ) ) ;
#44230 = CARTESIAN_POINT ( 'NONE',  ( 19.35000000122903430, -2.886751345948129988, 4.999999999999997335 ) ) ;
#44231 = CARTESIAN_POINT ( 'NONE',  ( 14.61562500061451608, -6.054752690667223547, -1.112240025338166033E-15 ) ) ;
#44232 = CARTESIAN_POINT ( 'NONE',  ( 18.10312500061451502, 0.000000000000000000, 5.243569643749999010 ) ) ;
#44233 = CARTESIAN_POINT ( 'NONE',  ( 25.98750000122903003, 4.330127018922191873, 2.499999999999999556 ) ) ;
#44234 = CIRCLE ( 'NONE', #52438, 4.999999999999998224 ) ;
#44235 = CARTESIAN_POINT ( 'NONE',  ( 27.33750000122903145, 4.330127018922191873, 2.499999999999999556 ) ) ;
#44236 = CARTESIAN_POINT ( 'NONE',  ( 23.81250000000000000, -5.773502691896255534, -1.060575238724906372E-15 ) ) ;
#44237 = CARTESIAN_POINT ( 'NONE',  ( -3.756430356250001434, 12.90312499938548463, 32.16877607737301048 ) ) ;
#44238 = VECTOR ( 'NONE', #61945, 1000.000000000000000 ) ;
#44239 = CARTESIAN_POINT ( 'NONE',  ( 25.77187500061451075, 3.027376345333611329, 5.243569643749999010 ) ) ;
#44240 = CARTESIAN_POINT ( 'NONE',  ( 4.898587196589411843E-16, 20.00000000000000000, 33.99999999999999289 ) ) ;
#44241 = CARTESIAN_POINT ( 'NONE',  ( 13.68750000122903288, 6.123233995736764310E-16, -4.999999999999998224 ) ) ;
#44242 = CARTESIAN_POINT ( 'NONE',  ( 29.03437500061451715, -4.541064518000419881, 2.621784821874995952 ) ) ;
#44243 = CARTESIAN_POINT ( 'NONE',  ( 2.393811435568372112E-14, 18.63124999877096855, 34.00000000000000000 ) ) ;
#44244 = CARTESIAN_POINT ( 'NONE',  ( 4.396875000614516971, -3.027376345333610441, -5.243569643749999898 ) ) ;
#44245 = CARTESIAN_POINT ( 'NONE',  ( 25.79062500061451502, -3.027376345333614438, 5.243569643749998122 ) ) ;
#44246 = CARTESIAN_POINT ( 'NONE',  ( 1.878215178125000495, 14.62812499938548427, 26.74683588394047007 ) ) ;
#44247 = CARTESIAN_POINT ( 'NONE',  ( -1.071796769724496334, 15.27634618820330026, 26.00000000000000355 ) ) ;
#44248 = CARTESIAN_POINT ( 'NONE',  ( 11.18437500061451928, 6.421520780324663323E-16, -5.243569643749999010 ) ) ;
#44249 = CARTESIAN_POINT ( 'NONE',  ( 22.05000000122903003, -2.886751345948096681, 5.000000000000054179 ) ) ;
#44250 = CARTESIAN_POINT ( 'NONE',  ( 29.76562500061451644, 3.027376345333611329, 5.243569643749999010 ) ) ;
#44251 = CARTESIAN_POINT ( 'NONE',  ( 9.459375000614517859, 4.541064518000418104, -2.621784821874998173 ) ) ;
#44252 = CARTESIAN_POINT ( 'NONE',  ( 27.87187500061451573, 3.027376345333613106, -5.243569643749998122 ) ) ;
#44253 = CARTESIAN_POINT ( 'NONE',  ( 29.00625000122903074, 4.330127018922192761, -2.499999999999997780 ) ) ;
#44254 = CARTESIAN_POINT ( 'NONE',  ( 19.23749999999999716, -2.886751345948129988, 4.999999999999997335 ) ) ;
#44255 = ORIENTED_EDGE ( 'NONE', *, *, #12948, .F. ) ;
#44256 = CARTESIAN_POINT ( 'NONE',  ( 28.68749999999999645, -2.886751345948129988, 4.999999999999997335 ) ) ;
#44257 = CARTESIAN_POINT ( 'NONE',  ( 3.600000000000002309, -4.330127018922190985, -2.500000000000001332 ) ) ;
#44258 = VERTEX_POINT ( 'NONE', #50983 ) ;
#44259 = CARTESIAN_POINT ( 'NONE',  ( 16.82812500061451644, -4.541064518000419881, 2.621784821874995952 ) ) ;
#44260 = CARTESIAN_POINT ( 'NONE',  ( 8.015625000614518214, 3.027376345333613106, -5.243569643749998122 ) ) ;
#44261 = CARTESIAN_POINT ( 'NONE',  ( 22.05937500061451217, 2.746126346562643317, 4.756430356249998326 ) ) ;
#44262 = CARTESIAN_POINT ( 'NONE',  ( 6.496875000614517504, -3.027376345333614438, 5.243569643749998122 ) ) ;
#44263 = CARTESIAN_POINT ( 'NONE',  ( 18.30000000122903359, 5.773502691896255534, 3.535250795749688894E-16 ) ) ;
#44264 = VECTOR ( 'NONE', #70889, 1000.000000000000000 ) ;
#44265 = CARTESIAN_POINT ( 'NONE',  ( 15.67500000000000071, -4.330127018922194537, 2.499999999999995559 ) ) ;
#44266 = CARTESIAN_POINT ( 'NONE',  ( 6.159375000614517148, -4.541064518000417216, -2.621784821875001281 ) ) ;
#44267 = CARTESIAN_POINT ( 'NONE',  ( 11.55937500061451928, -4.541064518000417216, -2.621784821875001281 ) ) ;
#44268 = CARTESIAN_POINT ( 'NONE',  ( 24.60937500061451644, -4.541064518000417216, -2.621784821875001281 ) ) ;
#44269 = CARTESIAN_POINT ( 'NONE',  ( -3.999999999999999112, 16.36250000000000071, 27.69059892324149885 ) ) ;
#44270 = ORIENTED_EDGE ( 'NONE', *, *, #446, .F. ) ;
#44271 = CARTESIAN_POINT ( 'NONE',  ( 11.25000000000000000, -4.330127018922190985, -2.500000000000001332 ) ) ;
#44272 = CARTESIAN_POINT ( 'NONE',  ( 17.48437500061451999, 6.421520780324663323E-16, -5.243569643749999010 ) ) ;
#44273 = VECTOR ( 'NONE', #71494, 1000.000000000000000 ) ;
#44274 = CARTESIAN_POINT ( 'NONE',  ( 8.446875000614518569, -3.027376345333610441, -5.243569643749999898 ) ) ;
#44275 = CARTESIAN_POINT ( 'NONE',  ( -3.756430356250000102, 15.56562499938548427, 30.00000000000000000 ) ) ;
#44276 = CARTESIAN_POINT ( 'NONE',  ( 19.79999999999999716, -4.330127018922190985, -2.500000000000001332 ) ) ;
#44277 = CARTESIAN_POINT ( 'NONE',  ( -1.999999999999999112, 16.69999999999999929, 26.53589838486224650 ) ) ;
#44278 = CARTESIAN_POINT ( 'NONE',  ( 9.001249775931846008E-16, 10.97187500061451715, -25.09994784771203058 ) ) ;
#44279 = CARTESIAN_POINT ( 'NONE',  ( 22.62187500061451573, 2.746126346562643317, 4.756430356249998326 ) ) ;
#44280 = CARTESIAN_POINT ( 'NONE',  ( 12.44062500061451537, -3.027376345333610441, -5.243569643749999898 ) ) ;
#44281 = CARTESIAN_POINT ( 'NONE',  ( 28.43437500061451573, 4.541064518000418104, 2.621784821874999949 ) ) ;
#44282 = CARTESIAN_POINT ( 'NONE',  ( 16.94999999999999929, 0.000000000000000000, 4.999999999999998224 ) ) ;
#44283 = CARTESIAN_POINT ( 'NONE',  ( 28.17187500061451644, -6.054752690667223547, -1.112240025338166033E-15 ) ) ;
#44284 = CARTESIAN_POINT ( 'NONE',  ( 10.57500000000000107, 4.330127018922191873, 2.499999999999999556 ) ) ;
#44285 = CARTESIAN_POINT ( 'NONE',  ( -2.000000000000000000, 15.08750000122903501, 26.53589838486224650 ) ) ;
#44286 = CARTESIAN_POINT ( 'NONE',  ( 9.825000001229033941, 2.886751345948126879, 4.999999999999999112 ) ) ;
#44287 = AXIS2_PLACEMENT_3D ( 'NONE', #30199, #47192, #19092 ) ;
#44288 = CARTESIAN_POINT ( 'NONE',  ( 19.69687500061451857, -3.027376345333610441, -5.243569643749999898 ) ) ;
#44289 = CARTESIAN_POINT ( 'NONE',  ( 15.19687500061451857, -3.027376345333610441, -5.243569643749999898 ) ) ;
#44290 = DIRECTION ( 'NONE',  ( -0.000000000000000000, -1.000000000000000000, -0.000000000000000000 ) ) ;
#44291 = VERTEX_POINT ( 'NONE', #39543 ) ;
#44292 = CARTESIAN_POINT ( 'NONE',  ( 17.99062500061451786, 6.054752690667223547, 3.707466751127219781E-16 ) ) ;
#44293 = CIRCLE ( 'NONE', #54867, 9.000000000000000000 ) ;
#44294 = CARTESIAN_POINT ( 'NONE',  ( 2.953125000614516438, -4.541064518000417216, -2.621784821875001281 ) ) ;
#44295 = CARTESIAN_POINT ( 'NONE',  ( 16.09687500061452070, -3.027376345333610441, -5.243569643749999898 ) ) ;
#44296 = CARTESIAN_POINT ( 'NONE',  ( 5.603843221884248216, 8.282830004122001100, -27.84704757573690870 ) ) ;
#44297 = CARTESIAN_POINT ( 'NONE',  ( 17.76562500061451644, -6.054752690667223547, -1.112240025338166033E-15 ) ) ;
#44298 = CARTESIAN_POINT ( 'NONE',  ( 0.000000000000000000, 20.00000000000000000, 30.00000000000000000 ) ) ;
#44299 = CARTESIAN_POINT ( 'NONE',  ( 25.28437500061451715, 4.541064518000418104, 2.621784821874999949 ) ) ;
#44300 = CARTESIAN_POINT ( 'NONE',  ( -4.243569643749999898, 13.95312500061451821, 30.00000000000000000 ) ) ;
#44301 = CARTESIAN_POINT ( 'NONE',  ( 14.59687500061452070, -3.027376345333614438, 5.243569643749998122 ) ) ;
#44302 = CARTESIAN_POINT ( 'NONE',  ( 13.31250000122903288, 4.330127018922192761, -2.499999999999997780 ) ) ;
#44303 = CARTESIAN_POINT ( 'NONE',  ( 9.534375000614517148, 4.119189519843966529, 2.378215178124999607 ) ) ;
#44304 = CARTESIAN_POINT ( 'NONE',  ( 4.243569643749999898, 19.63437500061451857, -30.00000000000000000 ) ) ;
#44305 =( BOUNDED_CURVE ( )  B_SPLINE_CURVE ( 2, ( #46009, #46734, #58514, #59614, #24906, #24547, #47817, #59246, #8654 ),
 .UNSPECIFIED., .F., .F. ) 
 B_SPLINE_CURVE_WITH_KNOTS ( ( 3, 2, 2, 2, 3 ),
 ( 0.1250000000000000000, 0.1296296296296296224, 0.1388888888888888951, 0.1481481481481481399, 0.1527777777777777901 ),
 .UNSPECIFIED. ) 
 CURVE ( )  GEOMETRIC_REPRESENTATION_ITEM ( )  RATIONAL_B_SPLINE_CURVE ( ( 0.9330127018922192983, 0.9330127018922194093, 1.000000000000000000, 0.8660254037844387076, 1.000000000000000000, 0.8660254037844387076, 1.000000000000000000, 0.9330127018922191873, 0.9330127018922194093 ) ) 
 REPRESENTATION_ITEM ( '' )  );
#44306 = CARTESIAN_POINT ( 'NONE',  ( 21.60937500061451644, 4.541064518000418104, -2.621784821874998173 ) ) ;
#44307 = CARTESIAN_POINT ( 'NONE',  ( 22.83750000122903501, 4.330127018922191873, 2.499999999999999556 ) ) ;
#44308 = CARTESIAN_POINT ( 'NONE',  ( 17.33437500061451431, -4.541064518000419881, 2.621784821874995952 ) ) ;
#44309 = CARTESIAN_POINT ( 'NONE',  ( -4.243569643749999898, 13.10937500061451821, 30.00000000000000000 ) ) ;
#44310 = CARTESIAN_POINT ( 'NONE',  ( 18.17812500061451786, -4.541064518000419881, 2.621784821874995952 ) ) ;
#44311 = ORIENTED_EDGE ( 'NONE', *, *, #47391, .F. ) ;
#44312 = ORIENTED_EDGE ( 'NONE', *, *, #35309, .T. ) ;
#44313 = CARTESIAN_POINT ( 'NONE',  ( 21.30000000000000071, 4.330127018922192761, -2.499999999999997780 ) ) ;
#44314 = CARTESIAN_POINT ( 'NONE',  ( 17.39999999999999858, 0.000000000000000000, 4.999999999999998224 ) ) ;
#44315 = CARTESIAN_POINT ( 'NONE',  ( 24.92812500061451431, -4.541064518000419881, 2.621784821874995952 ) ) ;
#44316 = CARTESIAN_POINT ( 'NONE',  ( 4.753125000614515372, -4.541064518000417216, -2.621784821875001281 ) ) ;
#44317 = CARTESIAN_POINT ( 'NONE',  ( 16.95000000122903216, 5.773502691896255534, 3.535250795749688894E-16 ) ) ;
#44318 = CARTESIAN_POINT ( 'NONE',  ( 22.82812500061451644, 6.421520780324663323E-16, -5.243569643749999010 ) ) ;
#44319 = CARTESIAN_POINT ( 'NONE',  ( 22.57499999999999929, 6.123233995736764310E-16, -4.999999999999998224 ) ) ;
#44320 = CARTESIAN_POINT ( 'NONE',  ( 25.56562500061452070, 3.027376345333613106, -5.243569643749998122 ) ) ;
#44321 = CARTESIAN_POINT ( 'NONE',  ( 6.778125000614518392, 4.541064518000418104, 2.621784821874999949 ) ) ;
#44322 = ORIENTED_EDGE ( 'NONE', *, *, #4477, .F. ) ;
#44323 = CARTESIAN_POINT ( 'NONE',  ( -4.000000000000000888, 20.35624999877096641, 32.30940107675850470 ) ) ;
#44324 = CARTESIAN_POINT ( 'NONE',  ( 17.36250000000000071, 2.886751345948126879, 4.999999999999998224 ) ) ;
#44325 = CIRCLE ( 'NONE', #12443, 1.500000000000000444 ) ;
#44326 = CARTESIAN_POINT ( 'NONE',  ( 10.50937500061451679, 0.000000000000000000, 4.756430356249998326 ) ) ;
#44327 = CARTESIAN_POINT ( 'NONE',  ( 3.999999999999999112, 18.87500000000000000, 30.00000000000000000 ) ) ;
#44328 = CARTESIAN_POINT ( 'NONE',  ( -2.000000000000000000, 14.63750000122903394, -33.46410161513775705 ) ) ;
#44329 = CARTESIAN_POINT ( 'NONE',  ( -3.000416591977282496E-16, 17.49687500061451573, -34.90005215228797653 ) ) ;
#44330 = VECTOR ( 'NONE', #16628, 1000.000000000000000 ) ;
#44331 = CARTESIAN_POINT ( 'NONE',  ( 8.474999999999999645, -4.330127018922194537, 2.499999999999995559 ) ) ;
#44333 = CARTESIAN_POINT ( 'NONE',  ( 8.821875000614518569, -6.054752690667223547, -1.112240025338166033E-15 ) ) ;
#44332 = CIRCLE ( 'NONE', #40783, 9.000000000000000000 ) ;
#44334 = CARTESIAN_POINT ( 'NONE',  ( 7.387500001229032165, 6.123233995736764310E-16, -4.999999999999998224 ) ) ;
#44335 = CARTESIAN_POINT ( 'NONE',  ( 11.59687500061451892, -3.027376345333610441, -5.243569643749999898 ) ) ;
#44336 = LINE ( 'NONE', #1084, #32690 ) ;
#44337 = DIRECTION ( 'NONE',  ( -1.000000000000000000, -0.000000000000000000, -0.000000000000000000 ) ) ;
#44338 = VECTOR ( 'NONE', #7170, 1000.000000000000000 ) ;
#44339 = CARTESIAN_POINT ( 'NONE',  ( 19.68750000000000355, -2.886751345948163738, 4.999999999999939604 ) ) ;
#44340 = CARTESIAN_POINT ( 'NONE',  ( 10.39687500061451786, 6.054752690667223547, 3.707466751127219781E-16 ) ) ;
#44341 = CARTESIAN_POINT ( 'NONE',  ( 13.16250000000000142, 2.886751345948129099, -4.999999999999997335 ) ) ;
#44342 = CARTESIAN_POINT ( 'NONE',  ( 20.54062500061451502, -3.027376345333610441, -5.243569643749999898 ) ) ;
#44343 = DIRECTION ( 'NONE',  ( 1.000000000000000000, 0.000000000000000000, 0.000000000000000000 ) ) ;
#44344 =( BOUNDED_CURVE ( )  B_SPLINE_CURVE ( 2, ( #13873, #3170, #19399, #25322, #63396, #47867, #24953 ),
 .UNSPECIFIED., .F., .F. ) 
 B_SPLINE_CURVE_WITH_KNOTS ( ( 3, 2, 2, 3 ),
 ( 0.6833333333333333481, 0.6861111111111111160, 0.6888888888888888840, 0.6916666666666666519 ),
 .UNSPECIFIED. ) 
 CURVE ( )  GEOMETRIC_REPRESENTATION_ITEM ( )  RATIONAL_B_SPLINE_CURVE ( ( 1.000000000000000000, 0.8660254037844387076, 1.000000000000000000, 0.8660254037844387076, 1.000000000000000000, 0.8660254037844387076, 1.000000000000000000 ) ) 
 REPRESENTATION_ITEM ( '' )  );
#44345 = DIRECTION ( 'NONE',  ( -1.000000000000000000, -0.000000000000000000, -0.000000000000000000 ) ) ;
#44346 = CARTESIAN_POINT ( 'NONE',  ( 23.25937500061451857, -4.541064518000417216, -2.621784821875001281 ) ) ;
#44347 = CYLINDRICAL_SURFACE ( 'NONE', #15480, 4.999999999999998224 ) ;
#44348 =( BOUNDED_CURVE ( )  B_SPLINE_CURVE ( 3, ( #11321, #5776, #56021, #16477 ),
 .UNSPECIFIED., .F., .F. ) 
 B_SPLINE_CURVE_WITH_KNOTS ( ( 4, 4 ),
 ( 1.570796326794896780, 3.141592653589793116 ),
 .UNSPECIFIED. ) 
 CURVE ( )  GEOMETRIC_REPRESENTATION_ITEM ( )  RATIONAL_B_SPLINE_CURVE ( ( 1.000000000000000000, 0.8047378541243650485, 0.8047378541243650485, 1.000000000000000000 ) ) 
 REPRESENTATION_ITEM ( '' )  );
#44349 = EDGE_CURVE ( 'NONE', #30207, #8622, #5268, .T. ) ;
#44350 = CARTESIAN_POINT ( 'NONE',  ( 28.83750000122903145, -4.330127018922194537, 2.499999999999995559 ) ) ;
#44351 = CARTESIAN_POINT ( 'NONE',  ( 20.74687500061451217, 0.000000000000000000, 4.756430356249998326 ) ) ;
#44352 = CARTESIAN_POINT ( 'NONE',  ( 26.27812500061451573, -4.541064518000419881, 2.621784821874995952 ) ) ;
#44353 = CARTESIAN_POINT ( 'NONE',  ( 15.21562500061451750, 3.027376345333613106, -5.243569643749998122 ) ) ;
#44354 = CARTESIAN_POINT ( 'NONE',  ( 14.11875000122903323, 2.886751345948129099, -4.999999999999998224 ) ) ;
#44355 = CARTESIAN_POINT ( 'NONE',  ( 14.10937500061451644, 0.000000000000000000, 5.243569643749999010 ) ) ;
#44356 = CARTESIAN_POINT ( 'NONE',  ( 7.584375000614516082, 5.492252693125287522, 3.363034840372157021E-16 ) ) ;
#44357 = CARTESIAN_POINT ( 'NONE',  ( 24.00000000122902932, -2.886751345948125991, -5.000000000000000000 ) ) ;
#44358 = CARTESIAN_POINT ( 'NONE',  ( 2.971875000614517592, -6.054752690667223547, -1.112240025338166033E-15 ) ) ;
#44359 = CARTESIAN_POINT ( 'NONE',  ( 14.97187500061451892, 3.027376345333611329, 5.243569643749999010 ) ) ;
#44360 = CARTESIAN_POINT ( 'NONE',  ( 4.000000000000000000, 17.88124999877096855, 27.69059892324149885 ) ) ;
#44361 = DIRECTION ( 'NONE',  ( -1.000000000000000000, -0.000000000000000000, -0.000000000000000000 ) ) ;
#44362 = CARTESIAN_POINT ( 'NONE',  ( 23.59687500061451715, -3.027376345333614438, 5.243569643749998122 ) ) ;
#44363 = CARTESIAN_POINT ( 'NONE',  ( 16.05937500061451573, -4.541064518000417216, -2.621784821875001281 ) ) ;
#44364 = CARTESIAN_POINT ( 'NONE',  ( -1.878215178125001827, 15.75312499938548427, 33.25316411605952283 ) ) ;
#44365 = CARTESIAN_POINT ( 'NONE',  ( 27.37500000000000000, -4.330127018922194537, 2.499999999999995559 ) ) ;
#44366 = CARTESIAN_POINT ( 'NONE',  ( 3.262500001229035718, -4.330127018922190985, -2.500000000000001332 ) ) ;
#44367 = CARTESIAN_POINT ( 'NONE',  ( 4.650000000000001243, 4.330127018922192761, -2.499999999999997780 ) ) ;
#44368 = CARTESIAN_POINT ( 'NONE',  ( 29.82187500061451502, 2.746126346562643317, 4.756430356249998326 ) ) ;
#44369 = CARTESIAN_POINT ( 'NONE',  ( 19.04062500061451146, -3.027376345333614438, 5.243569643749998122 ) ) ;
#44370 = CARTESIAN_POINT ( 'NONE',  ( 10.20000000000000107, 0.000000000000000000, 4.999999999999998224 ) ) ;
#44371 = CARTESIAN_POINT ( 'NONE',  ( 4.565625000614516260, 3.027376345333611329, 5.243569643749999010 ) ) ;
#44372 = CARTESIAN_POINT ( 'NONE',  ( 17.36249999999999716, 2.886751345948126879, 4.999999999999999112 ) ) ;
#44373 =( BOUNDED_CURVE ( )  B_SPLINE_CURVE ( 2, ( #47492, #14232, #30861, #41955, #19768, #65575, #8331, #53770, #64476 ),
 .UNSPECIFIED., .F., .T. ) 
 B_SPLINE_CURVE_WITH_KNOTS ( ( 3, 2, 2, 2, 3 ),
 ( 0.4021739130434782705, 0.4057971014492753881, 0.4130434782608695676, 0.4202898550724637472, 0.4239130434782608647 ),
 .UNSPECIFIED. ) 
 CURVE ( )  GEOMETRIC_REPRESENTATION_ITEM ( )  RATIONAL_B_SPLINE_CURVE ( ( 0.9330127018922194093, 0.9330127018922194093, 1.000000000000000000, 0.8660254037844387076, 1.000000000000000000, 0.8660254037844387076, 1.000000000000000000, 0.9330127018922194093, 0.9330127018922194093 ) ) 
 REPRESENTATION_ITEM ( '' )  );
#44374 = DIRECTION ( 'NONE',  ( -1.000000000000000000, -0.000000000000000000, -0.000000000000000000 ) ) ;
#44375 = CARTESIAN_POINT ( 'NONE',  ( 21.30000000122903359, -2.886751345948125991, -5.000000000000000000 ) ) ;
#44376 = FACE_OUTER_BOUND ( 'NONE', #60541, .T. ) ;
#44377 = CARTESIAN_POINT ( 'NONE',  ( 25.99687500061451928, -3.027376345333610441, -5.243569643749999898 ) ) ;
#44378 = VECTOR ( 'NONE', #32052, 1000.000000000000000 ) ;
#44379 = EDGE_LOOP ( 'NONE', ( #13062, #10739, #476, #20063 ) ) ;
#44380 = CARTESIAN_POINT ( 'NONE',  ( 16.19062500061451715, 6.054752690667223547, 3.707466751127219781E-16 ) ) ;
#44381 = CARTESIAN_POINT ( 'NONE',  ( 24.29062500061451502, 6.054752690667223547, 3.707466751127219781E-16 ) ) ;
#44382 = CARTESIAN_POINT ( 'NONE',  ( 21.34687500061451715, -3.027376345333614438, 5.243569643749998122 ) ) ;
#44383 = CARTESIAN_POINT ( 'NONE',  ( 7.312500000000000000, 2.886751345948129099, -4.999999999999998224 ) ) ;
#44384 = CARTESIAN_POINT ( 'NONE',  ( 10.04062500061451502, -3.027376345333614438, 5.243569643749998122 ) ) ;
#44385 = CARTESIAN_POINT ( 'NONE',  ( 23.69062500061451004, -3.027376345333610441, -5.243569643749999898 ) ) ;
#44386 = CARTESIAN_POINT ( 'NONE',  ( 15.45937500061451608, 0.000000000000000000, 5.243569643749999010 ) ) ;
#44387 = CARTESIAN_POINT ( 'NONE',  ( 18.98437500061451644, 4.541064518000418104, 2.621784821874999949 ) ) ;
#44388 = CARTESIAN_POINT ( 'NONE',  ( 19.38750000000000284, -2.886751345948193048, -4.999999999999883649 ) ) ;
#44389 = CARTESIAN_POINT ( 'NONE',  ( 4.243569643749999898, 19.57812500061451644, 30.00000000000000000 ) ) ;
#44390 = CARTESIAN_POINT ( 'NONE',  ( 21.67500000122903359, -5.773502691896255534, -1.060575238724906372E-15 ) ) ;
#44391 = CARTESIAN_POINT ( 'NONE',  ( 17.22187500061451715, 2.746126346562643317, 4.756430356249998326 ) ) ;
#44392 = CARTESIAN_POINT ( 'NONE',  ( 12.10312500061451857, 4.541064518000418104, -2.621784821874998173 ) ) ;
#44393 = CARTESIAN_POINT ( 'NONE',  ( 8.971875000614515372, 3.027376345333613106, -5.243569643749998122 ) ) ;
#44394 = CARTESIAN_POINT ( 'NONE',  ( 6.759375000614516793, 4.541064518000418104, -2.621784821874998173 ) ) ;
#44395 = ORIENTED_EDGE ( 'NONE', *, *, #18491, .F. ) ;
#44396 = CARTESIAN_POINT ( 'NONE',  ( 27.38437500061451857, 6.421520780324663323E-16, -5.243569643749999010 ) ) ;
#44397 = CARTESIAN_POINT ( 'NONE',  ( 20.09062500061451573, -3.027376345333610441, -5.243569643749999898 ) ) ;
#44398 = CARTESIAN_POINT ( 'NONE',  ( 28.61250000122903359, 4.330127018922192761, -2.499999999999997780 ) ) ;
#44399 = CARTESIAN_POINT ( 'NONE',  ( 27.25312500061451360, -4.541064518000417216, -2.621784821875001281 ) ) ;
#44400 = CARTESIAN_POINT ( 'NONE',  ( 23.93437500061451573, 4.541064518000418104, 2.621784821874999949 ) ) ;
#44401 = CARTESIAN_POINT ( 'NONE',  ( 20.54062500061451502, -3.027376345333610441, -5.243569643749999898 ) ) ;
#44402 = CARTESIAN_POINT ( 'NONE',  ( 2.121784821875001281, 18.65937500061451715, 33.67503911421598417 ) ) ;
#44403 = CARTESIAN_POINT ( 'NONE',  ( 25.64062500061451644, 6.054752690667223547, 3.707466751127219781E-16 ) ) ;
#44404 = CARTESIAN_POINT ( 'NONE',  ( 3.600000001229033408, -2.886751345948129988, 4.999999999999997335 ) ) ;
#44405 = ORIENTED_EDGE ( 'NONE', *, *, #43499, .T. ) ;
#44406 = CARTESIAN_POINT ( 'NONE',  ( 27.41250000000000142, -5.773502691896255534, -1.060575238724906372E-15 ) ) ;
#44407 = CARTESIAN_POINT ( 'NONE',  ( -3.999999999999997335, 15.53749999999999964, -27.69059892324149175 ) ) ;
#44408 = CARTESIAN_POINT ( 'NONE',  ( 3.756430356249998770, 18.56562499938548427, 32.16877607737302469 ) ) ;
#44409 = CARTESIAN_POINT ( 'NONE',  ( 5.671875000614519102, -6.054752690667223547, -1.112240025338166033E-15 ) ) ;
#44410 = CARTESIAN_POINT ( 'NONE',  ( 13.15312500061451750, 0.000000000000000000, 5.243569643749999010 ) ) ;
#44411 = CARTESIAN_POINT ( 'NONE',  ( 6.984375000614516438, -4.541064518000419881, 2.621784821874995952 ) ) ;
#44412 = CARTESIAN_POINT ( 'NONE',  ( 25.53750000122903074, 4.330127018922191873, 2.499999999999999556 ) ) ;
#44413 = CARTESIAN_POINT ( 'NONE',  ( 14.25937500061451679, -4.541064518000417216, -2.621784821875001281 ) ) ;
#44414 = CARTESIAN_POINT ( 'NONE',  ( 3.496875000614518836, -3.027376345333610441, -5.243569643749999898 ) ) ;
#44415 = CARTESIAN_POINT ( 'NONE',  ( 28.98750000000000071, 5.773502691896255534, 3.535250795749688894E-16 ) ) ;
#44416 = CARTESIAN_POINT ( 'NONE',  ( 27.60937500061451644, 0.000000000000000000, 5.243569643749999010 ) ) ;
#44417 = CARTESIAN_POINT ( 'NONE',  ( 3.628125000614518036, 4.541064518000418104, 2.621784821874999949 ) ) ;
#44418 = CARTESIAN_POINT ( 'NONE',  ( 13.07812500061451821, 4.541064518000418104, 2.621784821874999949 ) ) ;
#44419 = ORIENTED_EDGE ( 'NONE', *, *, #30054, .F. ) ;
#44420 = CARTESIAN_POINT ( 'NONE',  ( 10.41562500061451679, 3.027376345333611329, 5.243569643749999010 ) ) ;
#44421 = CARTESIAN_POINT ( 'NONE',  ( 7.453125000614516438, -4.541064518000417216, -2.621784821875001281 ) ) ;
#44422 = CARTESIAN_POINT ( 'NONE',  ( 18.00937500061451502, 4.119189519843966529, -2.378215178124998275 ) ) ;
#44423 = CARTESIAN_POINT ( 'NONE',  ( 7.950000000000001954, 0.000000000000000000, 4.999999999999998224 ) ) ;
#44424 = DIRECTION ( 'NONE',  ( -1.000000000000000000, -0.000000000000000000, -0.000000000000000000 ) ) ;
#44425 = CARTESIAN_POINT ( 'NONE',  ( 18.67500000000000071, 4.330127018922191873, 2.499999999999999556 ) ) ;
#44426 = CARTESIAN_POINT ( 'NONE',  ( 18.79687500061451644, -3.027376345333610441, -5.243569643749999898 ) ) ;
#44427 = CARTESIAN_POINT ( 'NONE',  ( 14.02500000122903323, -5.773502691896255534, -1.060575238724906372E-15 ) ) ;
#44428 = CARTESIAN_POINT ( 'NONE',  ( 20.10000000000000142, 0.000000000000000000, 4.999999999999998224 ) ) ;
#44429 = VECTOR ( 'NONE', #61760, 1000.000000000000000 ) ;
#44430 = CARTESIAN_POINT ( 'NONE',  ( -2.121784821874996840, 15.37812500061451892, -26.32496088578401583 ) ) ;
#44431 = CARTESIAN_POINT ( 'NONE',  ( -4.000000000000000000, 13.56874999877096677, 30.00000000000000000 ) ) ;
#44432 = CARTESIAN_POINT ( 'NONE',  ( 25.28437500061451360, -2.746126346562646425, 4.756430356249996549 ) ) ;
#44433 = CARTESIAN_POINT ( 'NONE',  ( 16.78125000122903288, 6.123233995736764310E-16, -4.999999999999998224 ) ) ;
#44434 = CARTESIAN_POINT ( 'NONE',  ( 27.25312500061451360, -4.541064518000417216, -2.621784821875001281 ) ) ;
#44435 = CARTESIAN_POINT ( 'NONE',  ( 27.41250000000000142, -5.773502691896255534, -1.060575238724906372E-15 ) ) ;
#44436 = EDGE_CURVE ( 'NONE', #16881, #12792, #63292, .T. ) ;
#44437 = CARTESIAN_POINT ( 'NONE',  ( 8.765625000614518214, -6.054752690667223547, -1.112240025338166033E-15 ) ) ;
#44438 = CARTESIAN_POINT ( 'NONE',  ( 26.67187500061451289, -4.119189519843968306, 2.378215178124996054 ) ) ;
#44439 = CARTESIAN_POINT ( 'NONE',  ( 21.57187500061451502, 3.027376345333613106, -5.243569643749998122 ) ) ;
#44440 = CARTESIAN_POINT ( 'NONE',  ( 13.99687500061451395, 0.000000000000000000, 4.756430356249998326 ) ) ;
#44441 = CARTESIAN_POINT ( 'NONE',  ( 6.890625000614516438, -3.027376345333614438, 5.243569643749998122 ) ) ;
#44442 = CARTESIAN_POINT ( 'NONE',  ( 9.609375000614518214, 0.000000000000000000, 5.243569643749999010 ) ) ;
#44443 = ORIENTED_EDGE ( 'NONE', *, *, #18286, .T. ) ;
#44444 = CARTESIAN_POINT ( 'NONE',  ( 21.49687500061451573, -3.027376345333610441, -5.243569643749999898 ) ) ;
#44445 = CARTESIAN_POINT ( 'NONE',  ( -1.626862140677534273E-15, 15.93124999877096748, 34.00000000000000000 ) ) ;
#44446 = CARTESIAN_POINT ( 'NONE',  ( 28.98750000000000071, 5.773502691896255534, 3.535250795749688894E-16 ) ) ;
#44447 = CARTESIAN_POINT ( 'NONE',  ( 4.050000000000001599, -4.330127018922190985, -2.500000000000001332 ) ) ;
#44448 = CARTESIAN_POINT ( 'NONE',  ( 14.02500000122903323, -5.773502691896255534, -1.060575238724906372E-15 ) ) ;
#44449 = LINE ( 'NONE', #56599, #50240 ) ;
#44450 = CARTESIAN_POINT ( 'NONE',  ( 3.807538167735159185, -3.240779705755961526, 4.122180188640082399 ) ) ;
#44451 = VERTEX_POINT ( 'NONE', #57236 ) ;
#44452 = CARTESIAN_POINT ( 'NONE',  ( 11.88749999999999751, 5.773502691896255534, 3.535250795749688894E-16 ) ) ;
#44453 = CARTESIAN_POINT ( 'NONE',  ( 15.71250000000000213, -5.773502691896255534, -1.060575238724906372E-15 ) ) ;
#44454 = CARTESIAN_POINT ( 'NONE',  ( 12.67500000122903536, -5.773502691896255534, -1.060575238724906372E-15 ) ) ;
#44455 = CARTESIAN_POINT ( 'NONE',  ( 11.01562500061451821, -6.054752690667223547, -1.112240025338166033E-15 ) ) ;
#44456 = ORIENTED_EDGE ( 'NONE', *, *, #40764, .F. ) ;
#44457 = CARTESIAN_POINT ( 'NONE',  ( 10.01250000000000107, 2.886751345948129099, -4.999999999999998224 ) ) ;
#44458 = CARTESIAN_POINT ( 'NONE',  ( 18.52500000122903145, -5.773502691896255534, -1.060575238724906372E-15 ) ) ;
#44459 = CARTESIAN_POINT ( 'NONE',  ( -2.121784821874999949, 15.73437500061451644, -33.67503911421598417 ) ) ;
#44460 = CARTESIAN_POINT ( 'NONE',  ( 28.87500000122902932, -5.773502691896255534, -1.060575238724906372E-15 ) ) ;
#44461 = CARTESIAN_POINT ( 'NONE',  ( -3.756430356250000102, 15.11562499938548321, 30.00000000000000000 ) ) ;
#44462 = CARTESIAN_POINT ( 'NONE',  ( 10.57500000000000107, 4.330127018922191873, 2.499999999999999556 ) ) ;
#44463 = CARTESIAN_POINT ( 'NONE',  ( 3.114784886354099669, 3.911322423985381658, 3.293568724887664168 ) ) ;
#44464 = ORIENTED_EDGE ( 'NONE', *, *, #14707, .F. ) ;
#44465 = CARTESIAN_POINT ( 'NONE',  ( 25.15312500061451217, 4.541064518000418104, -2.621784821874998173 ) ) ;
#44466 = CARTESIAN_POINT ( 'NONE',  ( 25.63125000122903074, -4.330127018922194537, 2.499999999999995559 ) ) ;
#44467 = VECTOR ( 'NONE', #28756, 1000.000000000000000 ) ;
#44468 = CARTESIAN_POINT ( 'NONE',  ( 29.07187500061451502, -6.054752690667223547, -1.112240025338166033E-15 ) ) ;
#44469 = CARTESIAN_POINT ( 'NONE',  ( 20.44687500061451857, -3.027376345333614438, 5.243569643749998122 ) ) ;
#44470 = CARTESIAN_POINT ( 'NONE',  ( 17.91562500061451502, 3.027376345333613106, -5.243569643749998122 ) ) ;
#44471 = CARTESIAN_POINT ( 'NONE',  ( -3.000416591977282496E-16, 11.14062500061459637, -34.90005215228797653 ) ) ;
#44472 = CARTESIAN_POINT ( 'NONE',  ( 5.465625000614517504, 3.027376345333611329, 5.243569643749999010 ) ) ;
#44473 = CARTESIAN_POINT ( 'NONE',  ( 28.65000000122903145, 5.773502691896255534, 3.535250795749688894E-16 ) ) ;
#44474 = CARTESIAN_POINT ( 'NONE',  ( 24.75937500061451502, 4.119189519843966529, -2.378215178124998275 ) ) ;
#44475 = CARTESIAN_POINT ( 'NONE',  ( 20.20312500061451644, 4.541064518000418104, -2.621784821874998173 ) ) ;
#44476 = CARTESIAN_POINT ( 'NONE',  ( 8.334375000614516082, -4.119189519843968306, 2.378215178124996054 ) ) ;
#44477 = CARTESIAN_POINT ( 'NONE',  ( -3.756430356249999214, 18.22812499938548214, 27.83122392262697531 ) ) ;
#44478 = CARTESIAN_POINT ( 'NONE',  ( 15.49687500061451750, -3.027376345333614438, 5.243569643749998122 ) ) ;
#44479 = CARTESIAN_POINT ( 'NONE',  ( 15.42187500061451821, 3.027376345333611329, 5.243569643749999010 ) ) ;
#44480 = CARTESIAN_POINT ( 'NONE',  ( 21.68437500061451573, 4.541064518000418104, 2.621784821874999949 ) ) ;
#44481 = ORIENTED_EDGE ( 'NONE', *, *, #17040, .T. ) ;
#44482 = CARTESIAN_POINT ( 'NONE',  ( -3.000416591977282496E-16, 12.54687500061451999, 25.09994784771203058 ) ) ;
#44483 = DIRECTION ( 'NONE',  ( -1.000000000000000000, -0.000000000000000000, -0.000000000000000000 ) ) ;
#44484 = CARTESIAN_POINT ( 'NONE',  ( 26.05312500061451431, 4.541064518000418104, -2.621784821874998173 ) ) ;
#44485 = CARTESIAN_POINT ( 'NONE',  ( 27.96562500061451928, 3.027376345333611329, 5.243569643749999010 ) ) ;
#44486 = CARTESIAN_POINT ( 'NONE',  ( 4.000000000000000000, 16.13749999999999929, 32.30940107675849049 ) ) ;
#44487 = AXIS2_PLACEMENT_3D ( 'NONE', #70022, #40876, #46774 ) ;
#44488 = CARTESIAN_POINT ( 'NONE',  ( 5.896875000614518747, 6.054752690667223547, 3.707466751127219781E-16 ) ) ;
#44489 = CARTESIAN_POINT ( 'NONE',  ( 12.11250000122903181, 0.000000000000000000, 4.999999999999998224 ) ) ;
#44490 = CARTESIAN_POINT ( 'NONE',  ( 6.712500001229034119, 0.000000000000000000, 4.999999999999998224 ) ) ;
#44491 = CARTESIAN_POINT ( 'NONE',  ( 29.66250000122903074, 0.000000000000000000, 4.999999999999998224 ) ) ;
#44492 = CARTESIAN_POINT ( 'NONE',  ( 2.000000000000000444, 17.91874999877096641, 26.53589838486224650 ) ) ;
#44493 = CARTESIAN_POINT ( 'NONE',  ( 18.69375000122903430, 5.773502691896255534, 3.535250795749688894E-16 ) ) ;
#44494 = CARTESIAN_POINT ( 'NONE',  ( 12.00937500061451857, -4.541064518000417216, -2.621784821875001281 ) ) ;
#44495 = CARTESIAN_POINT ( 'NONE',  ( 1.999999999999997335, 12.87500000000000178, 33.46410161513775705 ) ) ;
#44496 = ORIENTED_EDGE ( 'NONE', *, *, #24962, .F. ) ;
#44497 = CARTESIAN_POINT ( 'NONE',  ( 20.72812500061451502, 4.541064518000418104, 2.621784821874999949 ) ) ;
#44498 = CARTESIAN_POINT ( 'NONE',  ( 14.40937500061451715, 4.541064518000418104, -2.621784821874998173 ) ) ;
#44499 = CARTESIAN_POINT ( 'NONE',  ( 4.978125000614518569, 4.541064518000418104, 2.621784821874999949 ) ) ;
#44500 = CARTESIAN_POINT ( 'NONE',  ( 21.15937500061451715, 4.541064518000418104, -2.621784821874998173 ) ) ;
#44501 = CARTESIAN_POINT ( 'NONE',  ( 10.58437500061451964, -4.541064518000419881, 2.621784821874995952 ) ) ;
#44502 = CARTESIAN_POINT ( 'NONE',  ( 5.615625000614517859, -6.054752690667223547, -1.112240025338166033E-15 ) ) ;
#44503 = CARTESIAN_POINT ( 'NONE',  ( 10.98750000122903536, 6.123233995736764310E-16, -4.999999999999998224 ) ) ;
#44504 = CARTESIAN_POINT ( 'NONE',  ( 5.512500001229033941, -4.330127018922190985, -2.500000000000001332 ) ) ;
#44505 = CARTESIAN_POINT ( 'NONE',  ( 19.86562500061451786, 3.027376345333611329, 5.243569643749999010 ) ) ;
#44506 = CARTESIAN_POINT ( 'NONE',  ( 7.575000001229033053, 2.886751345948126879, 4.999999999999999112 ) ) ;
#44507 = CARTESIAN_POINT ( 'NONE',  ( 16.19062500061451715, 6.054752690667223547, 3.707466751127219781E-16 ) ) ;
#44508 = CARTESIAN_POINT ( 'NONE',  ( 16.19062500061451715, 6.054752690667223547, 3.707466751127219781E-16 ) ) ;
#44509 = CARTESIAN_POINT ( 'NONE',  ( 25.95937500061451431, -4.119189519843965641, -2.378215178125001383 ) ) ;
#44510 = CARTESIAN_POINT ( 'NONE',  ( 14.88750000000000107, -2.886751345948125991, -5.000000000000000000 ) ) ;
#44511 = CARTESIAN_POINT ( 'NONE',  ( 10.42500000122903536, -5.773502691896255534, -1.060575238724906372E-15 ) ) ;
#44512 = CARTESIAN_POINT ( 'NONE',  ( 8.990625000614516082, 6.054752690667223547, 3.707466751127219781E-16 ) ) ;
#44513 = CARTESIAN_POINT ( 'NONE',  ( 11.24062500061451608, 6.054752690667223547, 3.707466751127219781E-16 ) ) ;
#44514 = CARTESIAN_POINT ( 'NONE',  ( 22.05000000122903714, -2.886751345948129988, 4.999999999999997335 ) ) ;
#44515 = CARTESIAN_POINT ( 'NONE',  ( 28.19999999999999929, 0.000000000000000000, 4.999999999999998224 ) ) ;
#44516 = CARTESIAN_POINT ( 'NONE',  ( 2.121784821874999061, 12.50937500061451857, -33.67503911421598417 ) ) ;
#44517 = CARTESIAN_POINT ( 'NONE',  ( 0.000000000000000000, 20.00000000000000000, 30.00000000000000000 ) ) ;
#44518 = EDGE_CURVE ( 'NONE', #52358, #35925, #48654, .T. ) ;
#44519 = CARTESIAN_POINT ( 'NONE',  ( 3.300000001229034918, -2.886751345948125991, -5.000000000000000000 ) ) ;
#44520 = VECTOR ( 'NONE', #41452, 1000.000000000000000 ) ;
#44521 = CARTESIAN_POINT ( 'NONE',  ( 5.071875000614519458, 3.027376345333611329, 5.243569643749999010 ) ) ;
#44522 = CARTESIAN_POINT ( 'NONE',  ( 19.65937500061451360, -4.541064518000417216, -2.621784821875001281 ) ) ;
#44523 = CARTESIAN_POINT ( 'NONE',  ( 8.812500000000000000, 2.886751345948238789, 4.999999999999807265 ) ) ;
#44524 = CARTESIAN_POINT ( 'NONE',  ( 15.47812500061451679, -4.541064518000419881, 2.621784821874995952 ) ) ;
#44525 = CARTESIAN_POINT ( 'NONE',  ( 12.65625000122903110, -4.330127018922190985, -2.500000000000001332 ) ) ;
#44526 = CARTESIAN_POINT ( 'NONE',  ( -1.071796769724483234, 15.40759618943233811, -34.00000000000000711 ) ) ;
#44527 = CARTESIAN_POINT ( 'NONE',  ( 14.47499999999999964, 6.123233995736764310E-16, -4.999999999999998224 ) ) ;
#44528 = CARTESIAN_POINT ( 'NONE',  ( 28.13437500061451502, -4.541064518000419881, 2.621784821874995952 ) ) ;
#44529 = CARTESIAN_POINT ( 'NONE',  ( 21.12187500061451217, 4.119189519843966529, 2.378215178124999607 ) ) ;
#44530 = CARTESIAN_POINT ( 'NONE',  ( 14.09062500061451750, -3.027376345333614438, 5.243569643749998122 ) ) ;
#44531 = CARTESIAN_POINT ( 'NONE',  ( 11.33437500061451608, 4.541064518000418104, 2.621784821874999949 ) ) ;
#44532 = ORIENTED_EDGE ( 'NONE', *, *, #68656, .T. ) ;
#44533 = B_SPLINE_CURVE_WITH_KNOTS ( 'NONE', 3,
 ( #15207, #70633, #43669, #14479, #71002, #2673, #8578, #25190, #20378, #47734 ),
 .UNSPECIFIED., .F., .F.,
 ( 4, 3, 3, 4 ),
 ( 1.830297688535119174E-16, 0.0001572358266159529683, 0.0003242863666395115214, 0.0004914386806651677500 ),
 .UNSPECIFIED. ) ;
#44534 = CARTESIAN_POINT ( 'NONE',  ( 29.09062500061451573, -3.027376345333610441, -5.243569643749999898 ) ) ;
#44535 = CARTESIAN_POINT ( 'NONE',  ( 22.82812500061451644, 6.421520780324663323E-16, -5.243569643749999010 ) ) ;
#44536 = CYLINDRICAL_SURFACE ( 'NONE', #59265, 4.000000000000000000 ) ;
#44537 = CARTESIAN_POINT ( 'NONE',  ( -4.000000000000000000, 20.37500000000000000, 30.00000000000000000 ) ) ;
#44538 = CARTESIAN_POINT ( 'NONE',  ( 11.70000000000000284, -4.330127018922190985, -2.500000000000001332 ) ) ;
#44539 = CARTESIAN_POINT ( 'NONE',  ( 20.73750000122903359, -4.330127018922194537, 2.499999999999995559 ) ) ;
#44540 = CARTESIAN_POINT ( 'NONE',  ( 16.71562500061451573, 3.027376345333611329, 5.243569643749999010 ) ) ;
#44541 = CARTESIAN_POINT ( 'NONE',  ( 11.85937500061451821, -5.492252693125287522, -1.008910452111647106E-15 ) ) ;
#44542 = ORIENTED_EDGE ( 'NONE', *, *, #5151, .F. ) ;
#44543 = CARTESIAN_POINT ( 'NONE',  ( 19.68750000000000355, -2.886751345948129988, 4.999999999999997335 ) ) ;
#44544 = CARTESIAN_POINT ( 'NONE',  ( 21.34687500061451715, -3.027376345333614438, 5.243569643749998122 ) ) ;
#44545 = CARTESIAN_POINT ( 'NONE',  ( 26.84062500061451573, -3.027376345333610441, -5.243569643749999898 ) ) ;
#44546 = ORIENTED_EDGE ( 'NONE', *, *, #21079, .F. ) ;
#44547 = CARTESIAN_POINT ( 'NONE',  ( 21.13125000122903074, -4.330127018922194537, 2.499999999999995559 ) ) ;
#44548 = CARTESIAN_POINT ( 'NONE',  ( 9.515625000614518214, 3.027376345333611329, 5.243569643749999010 ) ) ;
#44549 = CARTESIAN_POINT ( 'NONE',  ( 6.262500000000000178, -5.773502691896255534, -1.060575238724906372E-15 ) ) ;
#44550 = CARTESIAN_POINT ( 'NONE',  ( 16.98750000000000426, -2.886751345948129988, 4.999999999999997335 ) ) ;
#44551 = CARTESIAN_POINT ( 'NONE',  ( 25.31250000000000000, 2.886751345948129099, -4.999999999999998224 ) ) ;
#44552 = CARTESIAN_POINT ( 'NONE',  ( -4.243569643749997233, 18.94062500061451715, 32.45002607614398471 ) ) ;
#44553 = CARTESIAN_POINT ( 'NONE',  ( 3.871875000614519280, -6.054752690667223547, -1.112240025338166033E-15 ) ) ;
#44554 = CARTESIAN_POINT ( 'NONE',  ( 29.44687500061451857, -3.027376345333614438, 5.243569643749998122 ) ) ;
#44555 = ORIENTED_EDGE ( 'NONE', *, *, #39198, .F. ) ;
#44556 = CARTESIAN_POINT ( 'NONE',  ( 24.25312500061451715, 4.541064518000418104, -2.621784821874998173 ) ) ;
#44557 = CARTESIAN_POINT ( 'NONE',  ( 24.49687500061451573, -3.027376345333614438, 5.243569643749998122 ) ) ;
#44558 = CARTESIAN_POINT ( 'NONE',  ( -3.000416591977282496E-16, 19.24062500061459247, -34.90005215228797653 ) ) ;
#44559 = CARTESIAN_POINT ( 'NONE',  ( 13.91249999999999964, -5.773502691896255534, -1.060575238724906372E-15 ) ) ;
#44560 = CARTESIAN_POINT ( 'NONE',  ( 7.865625000614516971, -6.054752690667223547, -1.112240025338166033E-15 ) ) ;
#44561 = CARTESIAN_POINT ( 'NONE',  ( 3.709174336338540989, 3.352913023424228811, 4.031500572517469294 ) ) ;
#44562 = CARTESIAN_POINT ( 'NONE',  ( 13.53750000000000142, -2.886751345948126435, -5.000000000000000000 ) ) ;
#44563 = CARTESIAN_POINT ( 'NONE',  ( 25.45312500061451644, -4.541064518000417216, -2.621784821875001281 ) ) ;
#44564 = CARTESIAN_POINT ( 'NONE',  ( 15.67500000122903181, 2.886751345948126879, 4.999999999999999112 ) ) ;
#44565 = CARTESIAN_POINT ( 'NONE',  ( 28.84687500061451360, 0.000000000000000000, 4.756430356249998326 ) ) ;
#44566 = CARTESIAN_POINT ( 'NONE',  ( 14.52187500061451608, 2.746126346562643317, 4.756430356249998326 ) ) ;
#44567 = CYLINDRICAL_SURFACE ( 'NONE', #30056, 4.999999999999998224 ) ;
#44568 = CARTESIAN_POINT ( 'NONE',  ( 19.99687500061451573, -3.027376345333614438, 5.243569643749998122 ) ) ;
#44569 = CARTESIAN_POINT ( 'NONE',  ( -3.000416591977282496E-16, 13.89687500061451786, 25.09994784771203058 ) ) ;
#44570 = CARTESIAN_POINT ( 'NONE',  ( 21.00937500061451857, -4.541064518000417216, -2.621784821875001281 ) ) ;
#44571 = CARTESIAN_POINT ( 'NONE',  ( 29.59687500061451715, -3.027376345333610441, -5.243569643749999898 ) ) ;
#44572 = CARTESIAN_POINT ( 'NONE',  ( -4.243569643749999898, 18.50937500061451857, 30.00000000000000000 ) ) ;
#44573 = CARTESIAN_POINT ( 'NONE',  ( 10.90312500061451928, 0.000000000000000000, 5.243569643749999010 ) ) ;
#44574 = CARTESIAN_POINT ( 'NONE',  ( 6.309375000614517504, 4.541064518000418104, -2.621784821874998173 ) ) ;
#44575 = CARTESIAN_POINT ( 'NONE',  ( 7.425000001229032698, 2.886751345948062486, -5.000000000000113687 ) ) ;
#44576 = CARTESIAN_POINT ( 'NONE',  ( 7.603125000614517681, 4.541064518000418104, -2.621784821874998173 ) ) ;
#44577 = CARTESIAN_POINT ( 'NONE',  ( 11.93437500061451573, -4.541064518000419881, 2.621784821874995952 ) ) ;
#44578 = SHAPE_REPRESENTATION_RELATIONSHIP ( 'NONE' , 'NONE' ,  #13196, #47954 ) ;
#44579 = CARTESIAN_POINT ( 'NONE',  ( 19.53750000122903430, 6.123233995736764310E-16, -4.999999999999998224 ) ) ;
#44580 = CARTESIAN_POINT ( 'NONE',  ( 8.109375000614518214, 4.541064518000418104, -2.621784821874998173 ) ) ;
#44581 = CARTESIAN_POINT ( 'NONE',  ( 9.628125000614517148, -4.541064518000419881, 2.621784821874995952 ) ) ;
#44582 = CARTESIAN_POINT ( 'NONE',  ( 6.178125000614518747, 6.421520780324663323E-16, -5.243569643749999010 ) ) ;
#44583 = CARTESIAN_POINT ( 'NONE',  ( 26.45625000122903003, 0.000000000000000000, 4.999999999999998224 ) ) ;
#44584 = CARTESIAN_POINT ( 'NONE',  ( 18.79687500061451644, -3.027376345333610441, -5.243569643749999898 ) ) ;
#44585 = DIRECTION ( 'NONE',  ( -1.000000000000000000, -0.000000000000000000, -0.000000000000000000 ) ) ;
#44586 = CARTESIAN_POINT ( 'NONE',  ( 27.92812500061451431, 4.541064518000418104, 2.621784821874999949 ) ) ;
#44587 = CARTESIAN_POINT ( 'NONE',  ( 11.35312500061451679, 0.000000000000000000, 5.243569643749999010 ) ) ;
#44588 = CARTESIAN_POINT ( 'NONE',  ( 29.74687500061451573, 6.054752690667223547, 3.707466751127219781E-16 ) ) ;
#44589 = CARTESIAN_POINT ( 'NONE',  ( 2.121784821874999061, 12.95937500061451786, -33.67503911421598417 ) ) ;
#44590 = CARTESIAN_POINT ( 'NONE',  ( 13.23750000122903359, 6.123233995736764310E-16, -4.999999999999998224 ) ) ;
#44591 =( BOUNDED_CURVE ( )  B_SPLINE_CURVE ( 2, ( #536, #7153, #62219, #57387, #6794, #17500, #63296, #51858, #34495 ),
 .UNSPECIFIED., .F., .F. ) 
 B_SPLINE_CURVE_WITH_KNOTS ( ( 3, 2, 2, 2, 3 ),
 ( 0.2934782608695652439, 0.2971014492753623060, 0.3043478260869565410, 0.3115942028985507206, 0.3152173913043478382 ),
 .UNSPECIFIED. ) 
 CURVE ( )  GEOMETRIC_REPRESENTATION_ITEM ( )  RATIONAL_B_SPLINE_CURVE ( ( 0.9330127018922194093, 0.9330127018922198534, 1.000000000000000000, 0.8660254037844387076, 1.000000000000000000, 0.8660254037844387076, 1.000000000000000000, 0.9330127018922188542, 0.9330127018922194093 ) ) 
 REPRESENTATION_ITEM ( '' )  );
#44592 = ADVANCED_FACE ( 'NONE', ( #57602 ), #69786, .T. ) ;
#44593 = CARTESIAN_POINT ( 'NONE',  ( 4.243569643749999010, 16.46562500061451573, -32.45002607614398471 ) ) ;
#44594 = CARTESIAN_POINT ( 'NONE',  ( 14.85000000122903252, -2.886751345948129988, 4.999999999999997335 ) ) ;
#44595 = CARTESIAN_POINT ( 'NONE',  ( 9.253125000614517148, -4.541064518000417216, -2.621784821875001281 ) ) ;
#44596 = CARTESIAN_POINT ( 'NONE',  ( 14.17500000000000071, 4.330127018922191873, 2.499999999999999556 ) ) ;
#44597 = CARTESIAN_POINT ( 'NONE',  ( 13.66875000122902861, 2.886751345948018077, -5.000000000000190070 ) ) ;
#44598 = CARTESIAN_POINT ( 'NONE',  ( 22.45312500061451644, 4.541064518000418104, -2.621784821874998173 ) ) ;
#44599 = CARTESIAN_POINT ( 'NONE',  ( 8.709375000614517859, 0.000000000000000000, 5.243569643749999010 ) ) ;
#44600 = EDGE_CURVE ( 'NONE', #35381, #1565, #53521, .T. ) ;
#44601 = CARTESIAN_POINT ( 'NONE',  ( 10.68750000122903288, 4.330127018922191873, 2.499999999999999556 ) ) ;
#44602 = CARTESIAN_POINT ( 'NONE',  ( 17.43750000122903288, 4.330127018922191873, 2.499999999999999556 ) ) ;
#44603 = CARTESIAN_POINT ( 'NONE',  ( 14.80312500061451608, 4.541064518000418104, -2.621784821874998173 ) ) ;
#44604 = EDGE_CURVE ( 'NONE', #24717, #68198, #58100, .T. ) ;
#44605 = CARTESIAN_POINT ( 'NONE',  ( 19.37812500061451715, 4.541064518000418104, 2.621784821874999949 ) ) ;
#44606 = CARTESIAN_POINT ( 'NONE',  ( 24.93750000122903288, 6.123233995736764310E-16, -4.999999999999998224 ) ) ;
#44607 = CARTESIAN_POINT ( 'NONE',  ( 28.31250000122903288, 0.000000000000000000, 4.999999999999998224 ) ) ;
#44608 = CARTESIAN_POINT ( 'NONE',  ( 23.85000000000000142, -4.330127018922190985, -2.500000000000001332 ) ) ;
#44609 = CARTESIAN_POINT ( 'NONE',  ( -1.878215178124999163, 13.69062499938548427, 26.74683588394047007 ) ) ;
#44610 = CARTESIAN_POINT ( 'NONE',  ( 25.20937500061451431, 4.541064518000418104, -2.621784821874998173 ) ) ;
#44611 = CARTESIAN_POINT ( 'NONE',  ( 30.00000000000000000, 0.000000000000000000, 4.999999999999998224 ) ) ;
#44612 = CARTESIAN_POINT ( 'NONE',  ( 11.43750000122903465, 6.123233995736764310E-16, -4.999999999999998224 ) ) ;
#44613 = CARTESIAN_POINT ( 'NONE',  ( 27.27187500061451431, -6.054752690667223547, -1.112240025338166033E-15 ) ) ;
#44614 = DIRECTION ( 'NONE',  ( -1.000000000000000000, -0.000000000000000000, -0.000000000000000000 ) ) ;
#44615 = CARTESIAN_POINT ( 'NONE',  ( 4.171875000614517326, 3.027376345333611329, 5.243569643749999010 ) ) ;
#44616 = CARTESIAN_POINT ( 'NONE',  ( 24.44062500061451715, -3.027376345333614438, 5.243569643749998122 ) ) ;
#44617 = CARTESIAN_POINT ( 'NONE',  ( 3.756430356249998770, 14.96562499938548108, 32.16877607737301759 ) ) ;
#44618 = CARTESIAN_POINT ( 'NONE',  ( -4.000000000000000888, 14.05624999877096748, 32.30940107675850470 ) ) ;
#44619 = CARTESIAN_POINT ( 'NONE',  ( 9.534375000614517148, 4.541064518000418104, 2.621784821874999949 ) ) ;
#44620 = CARTESIAN_POINT ( 'NONE',  ( 50.00000000000000000, 1.494782592887643924, -8.875000000000003553 ) ) ;
#44621 = CARTESIAN_POINT ( 'NONE',  ( 29.46562500061451573, -6.054752690667223547, -1.112240025338166033E-15 ) ) ;
#44622 = CARTESIAN_POINT ( 'NONE',  ( 7.509375000614517681, -4.541064518000417216, -2.621784821875001281 ) ) ;
#44623 = CARTESIAN_POINT ( 'NONE',  ( 28.62187500061451573, -6.054752690667223547, -1.112240025338166033E-15 ) ) ;
#44624 = EDGE_CURVE ( 'NONE', #26527, #55366, #13255, .T. ) ;
#44625 = CARTESIAN_POINT ( 'NONE',  ( 30.00000000000000000, 6.123233995736764310E-16, -4.999999999999998224 ) ) ;
#44626 = CARTESIAN_POINT ( 'NONE',  ( 18.71249999999999858, 2.886751345948126879, 4.999999999999999112 ) ) ;
#44627 = VERTEX_POINT ( 'NONE', #63513 ) ;
#44628 = CARTESIAN_POINT ( 'NONE',  ( 27.00000000000000000, -4.330127018922190985, -2.500000000000001332 ) ) ;
#44629 = CARTESIAN_POINT ( 'NONE',  ( 28.92187500061451644, 3.027376345333611329, 5.243569643749999010 ) ) ;
#44630 = ORIENTED_EDGE ( 'NONE', *, *, #18715, .F. ) ;
#44631 = CARTESIAN_POINT ( 'NONE',  ( 18.02812500061451573, 4.541064518000418104, 2.621784821874999949 ) ) ;
#44632 = CARTESIAN_POINT ( 'NONE',  ( 9.515625000614518214, 3.027376345333611329, 5.243569643749999010 ) ) ;
#44633 = CARTESIAN_POINT ( 'NONE',  ( 22.13437500061451502, -2.746126346562646425, 4.756430356249996549 ) ) ;
#44634 = CARTESIAN_POINT ( 'NONE',  ( 4.621875000614516615, 3.027376345333611329, 5.243569643749999010 ) ) ;
#44635 = CARTESIAN_POINT ( 'NONE',  ( 17.88750000122903216, 4.330127018922191873, 2.499999999999999556 ) ) ;
#44636 = LINE ( 'NONE', #67165, #13790 ) ;
#44637 = CARTESIAN_POINT ( 'NONE',  ( 8.071875000614518569, 3.027376345333613106, -5.243569643749998122 ) ) ;
#44638 = CARTESIAN_POINT ( 'NONE',  ( 10.88437500061451679, 4.541064518000418104, 2.621784821874999949 ) ) ;
#44639 = CARTESIAN_POINT ( 'NONE',  ( 22.28437500061451715, -4.541064518000419881, 2.621784821874995952 ) ) ;
#44640 = CARTESIAN_POINT ( 'NONE',  ( 4.460096747122133110, -2.261369503107883983, 4.460096747122133110 ) ) ;
#44641 = EDGE_LOOP ( 'NONE', ( #21447, #52564, #2251, #50364, #43535, #70915, #55600, #72011, #59225, #21246, #3914, #49947, #17031, #5808, #47621, #67190, #16029, #6535, #13939, #53046, #14149, #16077, #41443, #50698, #34231, #70050, #55161, #25390, #22818, #59573, #43653, #27451, #64858, #842, #4881, #68653, #19681, #57182, #47507, #28043 ) ) ;
#44642 = CARTESIAN_POINT ( 'NONE',  ( 11.28749999999999787, -2.886751345948125991, -5.000000000000000000 ) ) ;
#44643 = CARTESIAN_POINT ( 'NONE',  ( 8.184375000614515727, 4.541064518000418104, 2.621784821874999949 ) ) ;
#44644 = CARTESIAN_POINT ( 'NONE',  ( 1.878215178125000495, 15.86562499938548321, 26.74683588394047007 ) ) ;
#44645 = CARTESIAN_POINT ( 'NONE',  ( 21.86250000000000071, 2.886751345948126879, 4.999999999999999112 ) ) ;
#44646 = CARTESIAN_POINT ( 'NONE',  ( 19.45312500061451644, 0.000000000000000000, 5.243569643749999010 ) ) ;
#44647 = CARTESIAN_POINT ( 'NONE',  ( 3.999999999999998668, 17.86250000000000071, 32.30940107675850470 ) ) ;
#44648 = CARTESIAN_POINT ( 'NONE',  ( 22.23750000000000071, 5.773502691896255534, 3.535250795749688401E-16 ) ) ;
#44649 = CARTESIAN_POINT ( 'NONE',  ( 23.22187500061451715, -5.492252693125287522, -1.008910452111647106E-15 ) ) ;
#44650 = CARTESIAN_POINT ( 'NONE',  ( 11.46562500061451573, -6.054752690667223547, -1.112240025338166033E-15 ) ) ;
#44651 = CARTESIAN_POINT ( 'NONE',  ( 29.82187500061451502, 3.027376345333611329, 5.243569643749999010 ) ) ;
#44652 = CARTESIAN_POINT ( 'NONE',  ( 20.10000000000000142, 0.000000000000000000, 4.999999999999998224 ) ) ;
#44653 = CARTESIAN_POINT ( 'NONE',  ( 28.95937500061451431, 0.000000000000000000, 5.243569643749999010 ) ) ;
#44654 = CARTESIAN_POINT ( 'NONE',  ( 9.412499999999999645, -5.773502691896255534, -1.060575238724906372E-15 ) ) ;
#44655 = CARTESIAN_POINT ( 'NONE',  ( 2.000000000000001332, 14.86250000122903536, 33.46410161513774995 ) ) ;
#44656 = CARTESIAN_POINT ( 'NONE',  ( 9.675000001229035362, 2.886751345948129099, -4.999999999999998224 ) ) ;
#44657 = CARTESIAN_POINT ( 'NONE',  ( 19.24687500061452283, -3.027376345333610441, -5.243569643749999898 ) ) ;
#44658 = CARTESIAN_POINT ( 'NONE',  ( 13.13437500061451857, 4.541064518000418104, 2.621784821874999949 ) ) ;
#44659 = CARTESIAN_POINT ( 'NONE',  ( 30.00000000000000000, 6.123233995736764310E-16, -4.999999999999998224 ) ) ;
#44660 = ORIENTED_EDGE ( 'NONE', *, *, #4793, .T. ) ;
#44661 = CARTESIAN_POINT ( 'NONE',  ( 14.91562500061451679, 3.027376345333611329, 5.243569643749999010 ) ) ;
#44662 = CARTESIAN_POINT ( 'NONE',  ( 25.46250000122903501, 4.330127018922192761, -2.499999999999997780 ) ) ;
#44663 = CARTESIAN_POINT ( 'NONE',  ( 15.79687500061451821, 6.054752690667223547, 3.707466751127219781E-16 ) ) ;
#44664 = CARTESIAN_POINT ( 'NONE',  ( 3.253125000614518036, 0.000000000000000000, 5.243569643749999010 ) ) ;
#44665 = CARTESIAN_POINT ( 'NONE',  ( 17.95312500061451644, 4.541064518000418104, -2.621784821874998173 ) ) ;
#44666 = CARTESIAN_POINT ( 'NONE',  ( 28.76250000122903216, 0.000000000000000000, 4.999999999999998224 ) ) ;
#44667 = CARTESIAN_POINT ( 'NONE',  ( 26.07187500061451857, 3.027376345333613106, -5.243569643749998122 ) ) ;
#44668 = CARTESIAN_POINT ( 'NONE',  ( 2.121784821874999061, 11.55312500061451786, 26.32496088578401583 ) ) ;
#44669 = CARTESIAN_POINT ( 'NONE',  ( 16.05937500061451573, -4.541064518000417216, -2.621784821875001281 ) ) ;
#44670 = CARTESIAN_POINT ( 'NONE',  ( 13.16250000122903430, -4.330127018922190985, -2.500000000000001332 ) ) ;
#44671 = CARTESIAN_POINT ( 'NONE',  ( 7.434375000614519280, -4.119189519843968306, 2.378215178124996054 ) ) ;
#44672 = CARTESIAN_POINT ( 'NONE',  ( -4.243569643749999898, 18.47187500061451715, -32.45002607614398471 ) ) ;
#44673 = CARTESIAN_POINT ( 'NONE',  ( 21.27187500061451786, 3.027376345333611329, 5.243569643749999010 ) ) ;
#44674 = CARTESIAN_POINT ( 'NONE',  ( 19.65000000122902790, 5.773502691896255534, 3.535250795749688894E-16 ) ) ;
#44675 = CARTESIAN_POINT ( 'NONE',  ( 17.82187500061451502, -6.054752690667223547, -1.112240025338166033E-15 ) ) ;
#44676 = CARTESIAN_POINT ( 'NONE',  ( 9.001249775931846008E-16, 13.22187500061451715, 34.90005215228797653 ) ) ;
#44677 = CARTESIAN_POINT ( 'NONE',  ( 18.36562500061451431, 3.027376345333613106, -5.243569643749998122 ) ) ;
#44678 = ORIENTED_EDGE ( 'NONE', *, *, #42571, .T. ) ;
#44679 = ORIENTED_EDGE ( 'NONE', *, *, #57650, .F. ) ;
#44680 = CARTESIAN_POINT ( 'NONE',  ( 21.26249999999999574, 2.886751345948129099, -4.999999999999998224 ) ) ;
#44681 = CARTESIAN_POINT ( 'NONE',  ( -3.999999999999999112, 20.00000000000000000, -30.00000000000000000 ) ) ;
#44682 = CARTESIAN_POINT ( 'NONE',  ( 23.95312500061451289, 0.000000000000000000, 5.243569643749999010 ) ) ;
#44683 = CARTESIAN_POINT ( 'NONE',  ( 4.265625000614517326, -6.054752690667223547, -1.112240025338166033E-15 ) ) ;
#44684 = CARTESIAN_POINT ( 'NONE',  ( 16.61250000122903359, 0.000000000000000000, 4.999999999999998224 ) ) ;
#44685 = CARTESIAN_POINT ( 'NONE',  ( 22.49062500061451431, 6.054752690667223547, 3.707466751127219781E-16 ) ) ;
#44686 = CARTESIAN_POINT ( 'NONE',  ( 20.58750000000000213, -2.886751345948129988, 4.999999999999997335 ) ) ;
#44687 = EDGE_CURVE ( 'NONE', #45736, #10824, #25977, .T. ) ;
#44688 = CARTESIAN_POINT ( 'NONE',  ( 25.00312500061451715, -4.541064518000417216, -2.621784821875001281 ) ) ;
#44689 = CARTESIAN_POINT ( 'NONE',  ( 6.665625000614515905, 3.027376345333613106, -5.243569643749998122 ) ) ;
#44690 = ORIENTED_EDGE ( 'NONE', *, *, #21542, .F. ) ;
#44691 = CARTESIAN_POINT ( 'NONE',  ( 29.25000000000000000, -4.330127018922190985, -2.500000000000001332 ) ) ;
#44692 = CARTESIAN_POINT ( 'NONE',  ( 12.49687500061451573, -2.746126346562642428, -4.756430356249999214 ) ) ;
#44693 = CARTESIAN_POINT ( 'NONE',  ( 4.000000000000000000, 11.30000000122903536, -27.69059892324149530 ) ) ;
#44694 = CARTESIAN_POINT ( 'NONE',  ( 9.001249775931846008E-16, 19.52187500061451786, -25.09994784771203058 ) ) ;
#44695 = CARTESIAN_POINT ( 'NONE',  ( 8.062500000000000000, -5.773502691896255534, -1.060575238724906372E-15 ) ) ;
#44696 = CARTESIAN_POINT ( 'NONE',  ( 5.850000001229035185, -2.886751345948129988, 4.999999999999997335 ) ) ;
#44697 = CARTESIAN_POINT ( 'NONE',  ( 12.45937500061451786, -4.541064518000417216, -2.621784821875001281 ) ) ;
#44698 = FACE_OUTER_BOUND ( 'NONE', #70026, .T. ) ;
#44699 = CARTESIAN_POINT ( 'NONE',  ( 4.059375000614519280, 4.541064518000418104, -2.621784821874998173 ) ) ;
#44700 = DIRECTION ( 'NONE',  ( -0.000000000000000000, -1.000000000000000000, -0.000000000000000000 ) ) ;
#44701 = DIRECTION ( 'NONE',  ( 0.000000000000000000, 0.000000000000000000, 1.000000000000000000 ) ) ;
#44702 = CARTESIAN_POINT ( 'NONE',  ( 9.909375000614517148, 4.541064518000418104, -2.621784821874998173 ) ) ;
#44703 = CARTESIAN_POINT ( 'NONE',  ( 3.507483327083503521, -3.563363679198468859, 3.507483327083555924 ) ) ;
#44704 = CARTESIAN_POINT ( 'NONE',  ( 19.60312500061451502, -4.541064518000417216, -2.621784821875001281 ) ) ;
#44705 = CARTESIAN_POINT ( 'NONE',  ( -3.999999999999999112, 12.46250000122903323, -30.00000000000000000 ) ) ;
#44706 = CARTESIAN_POINT ( 'NONE',  ( 4.243569643749999010, 18.26562500061459460, 27.54997392385601174 ) ) ;
#44707 = CARTESIAN_POINT ( 'NONE',  ( 23.48437500061451644, 4.541064518000418104, 2.621784821874999949 ) ) ;
#44708 = CARTESIAN_POINT ( 'NONE',  ( 28.23750000122903359, 4.330127018922191873, 2.499999999999999556 ) ) ;
#44709 = CARTESIAN_POINT ( 'NONE',  ( 19.54687500061451289, -4.119189519843965641, -2.378215178125001383 ) ) ;
#44710 = CARTESIAN_POINT ( 'NONE',  ( 24.59062500061451573, -3.027376345333610441, -5.243569643749999898 ) ) ;
#44711 = CARTESIAN_POINT ( 'NONE',  ( 15.10312500061451502, -4.541064518000417216, -2.621784821875001281 ) ) ;
#44712 = CARTESIAN_POINT ( 'NONE',  ( 14.56875000122903252, 2.886751345948129099, -4.999999999999998224 ) ) ;
#44713 = CARTESIAN_POINT ( 'NONE',  ( 11.22187500061451892, 3.027376345333613106, -5.243569643749998122 ) ) ;
#44714 = CARTESIAN_POINT ( 'NONE',  ( 34.99999999999999289, 9.000000000000000000, 0.000000000000000000 ) ) ;
#44715 = CARTESIAN_POINT ( 'NONE',  ( 24.90000000122903145, -2.886751345948125991, -5.000000000000000000 ) ) ;
#44716 = CARTESIAN_POINT ( 'NONE',  ( 27.03750000000000142, -2.886751345948139758, -4.999999999999975131 ) ) ;
#44717 = CARTESIAN_POINT ( 'NONE',  ( 15.30937500061451750, 4.541064518000418104, -2.621784821874998173 ) ) ;
#44718 = CARTESIAN_POINT ( 'NONE',  ( -2.000000000000000000, 11.82500000000000107, 26.53589838486224650 ) ) ;
#44719 = CARTESIAN_POINT ( 'NONE',  ( 3.310802318797580579, -3.746810377620464205, 3.668301323911666412 ) ) ;
#44720 = EDGE_CURVE ( 'NONE', #65546, #22787, #58683, .T. ) ;
#44721 = CARTESIAN_POINT ( 'NONE',  ( 19.48125000122903216, 6.123233995736764310E-16, -4.999999999999998224 ) ) ;
#44722 = CARTESIAN_POINT ( 'NONE',  ( 25.92187500061451999, -6.054752690667223547, -1.112240025338166033E-15 ) ) ;
#44723 = CARTESIAN_POINT ( 'NONE',  ( 17.48437500061451999, 6.421520780324663323E-16, -5.243569643749999010 ) ) ;
#44724 = CARTESIAN_POINT ( 'NONE',  ( 1.878215178125000495, 16.87812499938548072, 26.74683588394047007 ) ) ;
#44725 = CARTESIAN_POINT ( 'NONE',  ( 28.12499999999999645, 4.330127018922191873, 2.499999999999999556 ) ) ;
#44726 = CARTESIAN_POINT ( 'NONE',  ( 3.150000001229034119, -2.886751345948129988, 4.999999999999997335 ) ) ;
#44727 = CARTESIAN_POINT ( 'NONE',  ( 4.425000000000001599, -4.330127018922194537, 2.499999999999995559 ) ) ;
#44728 = CARTESIAN_POINT ( 'NONE',  ( 29.63437500061451502, 5.824947211148865298E-16, -4.756430356249998326 ) ) ;
#44729 = CARTESIAN_POINT ( 'NONE',  ( 19.45312500061451644, 0.000000000000000000, 5.243569643749999010 ) ) ;
#44730 = CARTESIAN_POINT ( 'NONE',  ( 9.337500000000000355, -2.886751345948129988, 4.999999999999997335 ) ) ;
#44731 =( BOUNDED_CURVE ( )  B_SPLINE_CURVE ( 2, ( #4403, #38743, #67189, #71627, #15452, #27654, #72349, #21000, #32463 ),
 .UNSPECIFIED., .F., .F. ) 
 B_SPLINE_CURVE_WITH_KNOTS ( ( 3, 2, 2, 2, 3 ),
 ( 0.7282608695652174058, 0.7318840579710145233, 0.7391304347826086474, 0.7463768115942028825, 0.7500000000000000000 ),
 .UNSPECIFIED. ) 
 CURVE ( )  GEOMETRIC_REPRESENTATION_ITEM ( )  RATIONAL_B_SPLINE_CURVE ( ( 0.9330127018922194093, 0.9330127018922194093, 1.000000000000000000, 0.8660254037844387076, 1.000000000000000000, 0.8660254037844387076, 1.000000000000000000, 0.9330127018922194093, 0.9330127018922194093 ) ) 
 REPRESENTATION_ITEM ( '' )  );
#44732 = CARTESIAN_POINT ( 'NONE',  ( 7.285825834671762338E-16, 10.00000000000000000, -24.00000000000000000 ) ) ;
#44733 = CARTESIAN_POINT ( 'NONE',  ( 16.50000000000000000, 0.000000000000000000, 4.999999999999998224 ) ) ;
#44734 = CARTESIAN_POINT ( 'NONE',  ( -4.243569643749999898, 11.70312500061451644, 30.00000000000000000 ) ) ;
#44735 = CARTESIAN_POINT ( 'NONE',  ( 2.393811435568372112E-14, 18.23750000000000071, 34.00000000000000000 ) ) ;
#44736 = CARTESIAN_POINT ( 'NONE',  ( 20.02500000122903145, 2.886751345948129099, -4.999999999999998224 ) ) ;
#44737 = CARTESIAN_POINT ( 'NONE',  ( 15.11249999999999893, 2.886751345948126879, 4.999999999999998224 ) ) ;
#44738 = CARTESIAN_POINT ( 'NONE',  ( 27.83437500061451786, 6.421520780324663323E-16, -5.243569643749999010 ) ) ;
#44739 = ORIENTED_EDGE ( 'NONE', *, *, #49591, .T. ) ;
#44740 = CARTESIAN_POINT ( 'NONE',  ( 16.11562500061451786, 3.027376345333613106, -5.243569643749998122 ) ) ;
#44741 = CARTESIAN_POINT ( 'NONE',  ( 22.22812500061451502, -4.541064518000419881, 2.621784821874995952 ) ) ;
#44742 = CARTESIAN_POINT ( 'NONE',  ( 22.65937500061451715, 0.000000000000000000, 5.243569643749999010 ) ) ;
#44743 = CARTESIAN_POINT ( 'NONE',  ( 6.937499999999999112, 5.773502691896255534, 3.535250795749688894E-16 ) ) ;
#44744 = CARTESIAN_POINT ( 'NONE',  ( 10.07812500061451644, -4.541064518000419881, 2.621784821874995952 ) ) ;
#44745 = CARTESIAN_POINT ( 'NONE',  ( 24.51562500061451289, -6.054752690667223547, -1.112240025338166033E-15 ) ) ;
#44746 = CARTESIAN_POINT ( 'NONE',  ( 14.97187500061451892, 3.027376345333611329, 5.243569643749999010 ) ) ;
#44747 = CARTESIAN_POINT ( 'NONE',  ( 18.75937500061451857, -4.541064518000417216, -2.621784821875001281 ) ) ;
#44748 = DIRECTION ( 'NONE',  ( -1.000000000000000000, -0.000000000000000000, -0.000000000000000000 ) ) ;
#44749 = CARTESIAN_POINT ( 'NONE',  ( -2.121784821874996840, 18.07812500061451644, 33.67503911421598417 ) ) ;
#44750 = CARTESIAN_POINT ( 'NONE',  ( 20.55000000122903359, 5.773502691896255534, 3.535250795749688894E-16 ) ) ;
#44751 = CARTESIAN_POINT ( 'NONE',  ( 17.55937500061451573, 4.119189519843966529, -2.378215178124998275 ) ) ;
#44752 = CARTESIAN_POINT ( 'NONE',  ( 12.14062500061451821, 6.054752690667223547, 3.707466751127219781E-16 ) ) ;
#44753 = CARTESIAN_POINT ( 'NONE',  ( 6.159375000614517148, -4.541064518000417216, -2.621784821875001281 ) ) ;
#44754 = CARTESIAN_POINT ( 'NONE',  ( 5.559375000614517504, 0.000000000000000000, 5.243569643749999010 ) ) ;
#44755 = VERTEX_POINT ( 'NONE', #18431 ) ;
#44756 = CARTESIAN_POINT ( 'NONE',  ( 27.83437500061451786, 6.421520780324663323E-16, -5.243569643749999010 ) ) ;
#44757 = CARTESIAN_POINT ( 'NONE',  ( 19.94062500061451715, -3.027376345333614438, 5.243569643749998122 ) ) ;
#44758 = CARTESIAN_POINT ( 'NONE',  ( 3.290625000614516793, -3.027376345333614438, 5.243569643749998122 ) ) ;
#44759 = CARTESIAN_POINT ( 'NONE',  ( 27.74062500061451431, -3.027376345333610441, -5.243569643749999898 ) ) ;
#44760 = CARTESIAN_POINT ( 'NONE',  ( 23.40937500061451715, 4.541064518000418104, -2.621784821874998173 ) ) ;
#44761 = CARTESIAN_POINT ( 'NONE',  ( 18.47812500061451857, 4.541064518000418104, 2.621784821874999949 ) ) ;
#44762 = CARTESIAN_POINT ( 'NONE',  ( -3.999999999999999112, 10.55000000000000249, 30.00000000000000000 ) ) ;
#44763 = CARTESIAN_POINT ( 'NONE',  ( 24.36562500061451786, 3.027376345333611329, 5.243569643749999010 ) ) ;
#44764 = CARTESIAN_POINT ( 'NONE',  ( 4.950000001229033941, -2.886751345948129988, 4.999999999999997335 ) ) ;
#44765 = VERTEX_POINT ( 'NONE', #52071 ) ;
#44766 = CARTESIAN_POINT ( 'NONE',  ( 27.52500000000000213, 6.123233995736764310E-16, -4.999999999999998224 ) ) ;
#44767 = CARTESIAN_POINT ( 'NONE',  ( -2.828200636599751609E-16, 14.93750000000000000, -34.61880215351700230 ) ) ;
#44768 = CARTESIAN_POINT ( 'NONE',  ( -3.756430356250001434, 17.51562499938548356, 32.16877607737301048 ) ) ;
#44769 = CARTESIAN_POINT ( 'NONE',  ( 5.821875000614519458, 3.027376345333613106, -5.243569643749998122 ) ) ;
#44770 = CARTESIAN_POINT ( 'NONE',  ( 12.02812500061451573, 6.421520780324663323E-16, -5.243569643749999010 ) ) ;
#44771 = CARTESIAN_POINT ( 'NONE',  ( 7.209375000614519635, 4.541064518000418104, -2.621784821874998173 ) ) ;
#44772 = CARTESIAN_POINT ( 'NONE',  ( 25.20000000122903216, -2.886751345948129988, 4.999999999999997335 ) ) ;
#44773 = CARTESIAN_POINT ( 'NONE',  ( 13.88437500061451679, 6.421520780324663323E-16, -5.243569643749999010 ) ) ;
#44774 = CARTESIAN_POINT ( 'NONE',  ( 29.80312500061451431, 0.000000000000000000, 5.243569643749999010 ) ) ;
#44775 = CARTESIAN_POINT ( 'NONE',  ( 28.16249999999999787, 2.886751345948126879, 4.999999999999999112 ) ) ;
#44776 = ADVANCED_FACE ( 'NONE', ( #25446 ), #24347, .F. ) ;
#44777 = CARTESIAN_POINT ( 'NONE',  ( 27.23437500061451644, -4.541064518000419881, 2.621784821874995952 ) ) ;
#44778 = CARTESIAN_POINT ( 'NONE',  ( 4.078125000614517326, 4.541064518000418104, 2.621784821874999949 ) ) ;
#44779 = CARTESIAN_POINT ( 'NONE',  ( 13.52812500061451750, 4.541064518000418104, 2.621784821874999949 ) ) ;
#44780 = EDGE_CURVE ( 'NONE', #24228, #49807, #35793, .T. ) ;
#44781 = EDGE_LOOP ( 'NONE', ( #77, #49584, #51294, #20002 ) ) ;
#44782 = CARTESIAN_POINT ( 'NONE',  ( 9.740625000614516082, -3.027376345333610441, -5.243569643749999898 ) ) ;
#44783 = CARTESIAN_POINT ( 'NONE',  ( 9.515625000614518214, 3.027376345333611329, 5.243569643749999010 ) ) ;
#44784 = CARTESIAN_POINT ( 'NONE',  ( 18.64687500061451786, -2.746126346562646425, 4.756430356249996549 ) ) ;
#44785 = CARTESIAN_POINT ( 'NONE',  ( 14.64375000122903359, 5.773502691896255534, 3.535250795749688401E-16 ) ) ;
#44786 = CARTESIAN_POINT ( 'NONE',  ( 15.07499999999999929, 4.330127018922191873, 2.499999999999999556 ) ) ;
#44787 =( BOUNDED_CURVE ( )  B_SPLINE_CURVE ( 2, ( #66801, #60499, #4383, #45351, #43901, #50170, #56432, #15803, #61600 ),
 .UNSPECIFIED., .F., .F. ) 
 B_SPLINE_CURVE_WITH_KNOTS ( ( 3, 2, 2, 2, 3 ),
 ( 0.3586956521739130821, 0.3623188405797101441, 0.3695652173913043237, 0.3768115942028985588, 0.3804347826086956763 ),
 .UNSPECIFIED. ) 
 CURVE ( )  GEOMETRIC_REPRESENTATION_ITEM ( )  RATIONAL_B_SPLINE_CURVE ( ( 0.9330127018922194093, 0.9330127018922198534, 1.000000000000000000, 0.8660254037844387076, 1.000000000000000000, 0.8660254037844387076, 1.000000000000000000, 0.9330127018922188542, 0.9330127018922194093 ) ) 
 REPRESENTATION_ITEM ( '' )  );
#44788 = CARTESIAN_POINT ( 'NONE',  ( 15.00937500061451679, 0.000000000000000000, 5.243569643749999010 ) ) ;
#44789 = CARTESIAN_POINT ( 'NONE',  ( 12.60000000122903430, -2.886751345948129988, 4.999999999999997335 ) ) ;
#44790 = CARTESIAN_POINT ( 'NONE',  ( 19.16250000000000142, 2.886751345948126879, 4.999999999999999112 ) ) ;
#44791 = CARTESIAN_POINT ( 'NONE',  ( 20.89687500061452141, -3.027376345333614438, 5.243569643749998122 ) ) ;
#44792 = CARTESIAN_POINT ( 'NONE',  ( -2.121784821874999949, 14.32812500061451644, -33.67503911421598417 ) ) ;
#44793 = CARTESIAN_POINT ( 'NONE',  ( 24.64687500061451431, 4.119189519843966529, -2.378215178124998275 ) ) ;
#44794 = CARTESIAN_POINT ( 'NONE',  ( 1.999999999999997335, 13.26874999877096606, 33.46410161513775705 ) ) ;
#44795 = CARTESIAN_POINT ( 'NONE',  ( 27.85312500061451502, 4.541064518000418104, -2.621784821874998173 ) ) ;
#44796 = CARTESIAN_POINT ( 'NONE',  ( -3.999999999999999112, 19.55000000000000071, -30.00000000000000000 ) ) ;
#44797 = CARTESIAN_POINT ( 'NONE',  ( 24.37500000000000000, 6.123233995736764310E-16, -4.999999999999998224 ) ) ;
#44798 = CARTESIAN_POINT ( 'NONE',  ( 26.77499999999999858, 4.330127018922191873, 2.499999999999999556 ) ) ;
#44799 = CARTESIAN_POINT ( 'NONE',  ( 9.628125000614517148, -4.541064518000419881, 2.621784821874995952 ) ) ;
#44800 = CARTESIAN_POINT ( 'NONE',  ( 27.30937500061451217, 2.746126346562645981, -4.756430356249997438 ) ) ;
#44801 = CARTESIAN_POINT ( 'NONE',  ( 21.68437500061451573, 4.541064518000418104, 2.621784821874999949 ) ) ;
#44802 = CARTESIAN_POINT ( 'NONE',  ( 14.40937500061451537, 2.746126346562643317, 4.756430356249998326 ) ) ;
#44803 = CARTESIAN_POINT ( 'NONE',  ( 4.340625000614515727, -3.027376345333610441, -5.243569643749999898 ) ) ;
#44804 = CARTESIAN_POINT ( 'NONE',  ( 11.78437500061451892, 4.541064518000418104, 2.621784821874999949 ) ) ;
#44805 = ORIENTED_EDGE ( 'NONE', *, *, #8112, .F. ) ;
#44806 = CARTESIAN_POINT ( 'NONE',  ( 21.15937500061451715, 4.541064518000418104, -2.621784821874998173 ) ) ;
#44807 = CARTESIAN_POINT ( 'NONE',  ( 3.578402880298067856, 3.495305883107370448, -31.80580486484916491 ) ) ;
#44808 = CARTESIAN_POINT ( 'NONE',  ( 29.96250000000000213, 2.886751345948126879, 4.999999999999999112 ) ) ;
#44809 = CARTESIAN_POINT ( 'NONE',  ( 4.949999999999999289, -4.330127018922190985, -2.500000000000001332 ) ) ;
#44810 = CARTESIAN_POINT ( 'NONE',  ( 15.41250000122903252, -4.330127018922190985, -2.500000000000001332 ) ) ;
#44811 = CARTESIAN_POINT ( 'NONE',  ( 20.75625000122903430, -4.330127018922190985, -2.500000000000001332 ) ) ;
#44812 = ORIENTED_EDGE ( 'NONE', *, *, #21977, .T. ) ;
#44813 = CARTESIAN_POINT ( 'NONE',  ( 12.86250000000000071, 2.886751345948126879, 4.999999999999999112 ) ) ;
#44814 = CARTESIAN_POINT ( 'NONE',  ( 27.85312500061451502, 4.541064518000418104, -2.621784821874998173 ) ) ;
#44815 = CARTESIAN_POINT ( 'NONE',  ( 16.83749999999999858, 5.773502691896255534, 3.535250795749688894E-16 ) ) ;
#44816 = CARTESIAN_POINT ( 'NONE',  ( 9.600000001229034297, -2.886751345948125991, -5.000000000000000000 ) ) ;
#44817 = CARTESIAN_POINT ( 'NONE',  ( 9.065625000614517148, 3.027376345333611329, 5.243569643749999010 ) ) ;
#44818 = CARTESIAN_POINT ( 'NONE',  ( 9.299999999999998934, 0.000000000000000000, 4.999999999999998224 ) ) ;
#44819 = CARTESIAN_POINT ( 'NONE',  ( 2.121784821874999061, 15.65937500061451892, -33.67503911421598417 ) ) ;
#44820 = CARTESIAN_POINT ( 'NONE',  ( 27.82500000122903572, 2.886751345948126879, 4.999999999999999112 ) ) ;
#44821 = CARTESIAN_POINT ( 'NONE',  ( 1.878215178124997609, 15.71562499938548108, 33.25316411605952993 ) ) ;
#44822 = CARTESIAN_POINT ( 'NONE',  ( 6.299999999999999822, -4.330127018922190985, -2.500000000000001332 ) ) ;
#44823 = CARTESIAN_POINT ( 'NONE',  ( -1.999999999999997113, 13.32499999999999929, -26.53589838486224295 ) ) ;
#44824 = VERTEX_POINT ( 'NONE', #63147 ) ;
#44825 = CARTESIAN_POINT ( 'NONE',  ( 25.22812500061451502, 4.541064518000418104, 2.621784821874999949 ) ) ;
#44826 = CARTESIAN_POINT ( 'NONE',  ( 4.215355816196066030, -2.689023592745824143, 4.501582466356354395 ) ) ;
#44827 = CARTESIAN_POINT ( 'NONE',  ( 28.95937500061451431, 0.000000000000000000, 5.243569643749999010 ) ) ;
#44828 = CARTESIAN_POINT ( 'NONE',  ( 22.54687500061451999, 6.054752690667223547, 3.707466751127219781E-16 ) ) ;
#44829 = CARTESIAN_POINT ( 'NONE',  ( 15.62812500061451537, 6.421520780324663323E-16, -5.243569643749999010 ) ) ;
#44830 = CARTESIAN_POINT ( 'NONE',  ( 4.243569643749999898, 12.37812500061459353, -30.00000000000000000 ) ) ;
#44831 = CARTESIAN_POINT ( 'NONE',  ( 6.778125000614518392, 4.541064518000418104, 2.621784821874999949 ) ) ;
#44832 = CARTESIAN_POINT ( 'NONE',  ( 29.17500000122903714, 2.886751345948126879, 4.999999999999999112 ) ) ;
#44833 = CARTESIAN_POINT ( 'NONE',  ( 23.40937500061451715, 4.119189519843966529, -2.378215178124998275 ) ) ;
#44834 = CARTESIAN_POINT ( 'NONE',  ( 18.51562500061451289, 3.027376345333611329, 5.243569643749999010 ) ) ;
#44835 = CARTESIAN_POINT ( 'NONE',  ( 4.000000000000000000, 11.30000000122903536, -27.69059892324149885 ) ) ;
#44836 = CARTESIAN_POINT ( 'NONE',  ( -1.878215178125001827, 18.79062499938548214, 33.25316411605952283 ) ) ;
#44837 = CARTESIAN_POINT ( 'NONE',  ( 15.00937500061451679, 0.000000000000000000, 5.243569643749999010 ) ) ;
#44838 = CARTESIAN_POINT ( 'NONE',  ( 14.67187500061451821, -6.054752690667223547, -1.112240025338166033E-15 ) ) ;
#44839 = CARTESIAN_POINT ( 'NONE',  ( 22.65937500061451715, 0.000000000000000000, 5.243569643749999010 ) ) ;
#44840 = ORIENTED_EDGE ( 'NONE', *, *, #66601, .F. ) ;
#44841 = CARTESIAN_POINT ( 'NONE',  ( 3.531796677802674811, 3.539267187803308179, -3.868928841707397925 ) ) ;
#44842 = CARTESIAN_POINT ( 'NONE',  ( 25.86562500061451431, -6.054752690667223547, -1.112240025338166033E-15 ) ) ;
#44843 = CARTESIAN_POINT ( 'NONE',  ( 26.54062500061451146, 6.054752690667223547, 3.707466751127219781E-16 ) ) ;
#44844 = CARTESIAN_POINT ( 'NONE',  ( -1.071796769724480347, 17.26115380933863008, 34.00000000000000711 ) ) ;
#44845 = CARTESIAN_POINT ( 'NONE',  ( 3.999999999999999112, 16.62500000000000000, 30.00000000000000000 ) ) ;
#44846 = CARTESIAN_POINT ( 'NONE',  ( 5.634375000614519458, -4.541064518000419881, 2.621784821874995952 ) ) ;
#44847 = CARTESIAN_POINT ( 'NONE',  ( 12.15000000122903501, -2.886751345948129988, 4.999999999999997335 ) ) ;
#44848 = CARTESIAN_POINT ( 'NONE',  ( 6.525000001229033231, 2.886751345948129099, -4.999999999999998224 ) ) ;
#44849 = CARTESIAN_POINT ( 'NONE',  ( 3.590625000614518836, 6.054752690667223547, 3.707466751127219781E-16 ) ) ;
#44850 = CARTESIAN_POINT ( 'NONE',  ( 2.828200636599751609E-16, 17.95624999877096784, 25.38119784648299415 ) ) ;
#44851 = CARTESIAN_POINT ( 'NONE',  ( 18.43125000122903501, -4.330127018922194537, 2.499999999999995559 ) ) ;
#44852 = CARTESIAN_POINT ( 'NONE',  ( 10.80937500061451928, 4.541064518000418104, -2.621784821874998173 ) ) ;
#44853 = CARTESIAN_POINT ( 'NONE',  ( -4.000000000000000888, 17.65624999877096712, 32.30940107675850470 ) ) ;
#44854 = ORIENTED_EDGE ( 'NONE', *, *, #66541, .F. ) ;
#44855 = CARTESIAN_POINT ( 'NONE',  ( 20.05312500061451431, -4.541064518000417216, -2.621784821875001281 ) ) ;
#44856 = CARTESIAN_POINT ( 'NONE',  ( 13.99687500061451928, 6.054752690667223547, 3.707466751127219781E-16 ) ) ;
#44857 = CARTESIAN_POINT ( 'NONE',  ( 4.340625000614515727, -3.027376345333610441, -5.243569643749999898 ) ) ;
#44858 = CARTESIAN_POINT ( 'NONE',  ( 21.04687500061451644, -3.027376345333610441, -5.243569643749999898 ) ) ;
#44859 = CARTESIAN_POINT ( 'NONE',  ( 10.24687500061451750, -3.027376345333610441, -5.243569643749999898 ) ) ;
#44860 = CARTESIAN_POINT ( 'NONE',  ( 4.190625000614518925, -3.027376345333614438, 5.243569643749998122 ) ) ;
#44861 = CARTESIAN_POINT ( 'NONE',  ( 11.73750000122903181, -4.330127018922194537, 2.499999999999995559 ) ) ;
#44862 = CARTESIAN_POINT ( 'NONE',  ( 6.150000001229033231, 5.773502691896255534, 3.535250795749688894E-16 ) ) ;
#44863 = CARTESIAN_POINT ( 'NONE',  ( 19.64062500061451644, -3.027376345333610441, -5.243569643749999898 ) ) ;
#44864 = ADVANCED_FACE ( 'NONE', ( #57957 ), #2915, .F. ) ;
#44865 = CARTESIAN_POINT ( 'NONE',  ( 8.962500001229033231, 0.000000000000000000, 4.999999999999998224 ) ) ;
#44866 = CARTESIAN_POINT ( 'NONE',  ( 18.40312500061451573, 4.541064518000418104, -2.621784821874998173 ) ) ;
#44867 = CARTESIAN_POINT ( 'NONE',  ( 15.51562500061451644, -6.054752690667223547, -1.112240025338166033E-15 ) ) ;
#44868 = CARTESIAN_POINT ( 'NONE',  ( 24.83437500061451431, 4.119189519843966529, 2.378215178124999607 ) ) ;
#44869 = CARTESIAN_POINT ( 'NONE',  ( 16.72500000000000142, 6.123233995736764310E-16, -4.999999999999998224 ) ) ;
#44870 = CARTESIAN_POINT ( 'NONE',  ( 9.037500001229034297, -4.330127018922194537, 2.499999999999995559 ) ) ;
#44871 = CARTESIAN_POINT ( 'NONE',  ( 5.878125000614517148, 4.541064518000418104, 2.621784821874999949 ) ) ;
#44872 = EDGE_CURVE ( 'NONE', #71649, #57451, #7713, .T. ) ;
#44873 = CARTESIAN_POINT ( 'NONE',  ( 21.41250000122903074, 4.330127018922192761, -2.499999999999997780 ) ) ;
#44874 = CARTESIAN_POINT ( 'NONE',  ( 27.00000000000000000, -4.330127018922190985, -2.500000000000001332 ) ) ;
#44875 = CARTESIAN_POINT ( 'NONE',  ( 2.121784821875001281, 10.10937500061451821, -26.32496088578401938 ) ) ;
#44876 = LINE ( 'NONE', #10877, #32392 ) ;
#44877 = CARTESIAN_POINT ( 'NONE',  ( 2.662500001229036073, 0.000000000000000000, 4.999999999999998224 ) ) ;
#44878 = CARTESIAN_POINT ( 'NONE',  ( 4.621875000614516615, 3.027376345333611329, 5.243569643749999010 ) ) ;
#44879 = CARTESIAN_POINT ( 'NONE',  ( 20.70937500061451786, 4.541064518000418104, -2.621784821874998173 ) ) ;
#44880 = CARTESIAN_POINT ( 'NONE',  ( -3.999999999999999112, 15.01250000000000107, 27.69059892324149885 ) ) ;
#44881 = CARTESIAN_POINT ( 'NONE',  ( 15.85312500061451857, 0.000000000000000000, 5.243569643749999010 ) ) ;
#44882 = CARTESIAN_POINT ( 'NONE',  ( 12.95625000122903359, 0.000000000000000000, 4.999999999999998224 ) ) ;
#44883 = CARTESIAN_POINT ( 'NONE',  ( 23.13749999999999929, 5.773502691896255534, 3.535250795749688401E-16 ) ) ;
#44884 = CARTESIAN_POINT ( 'NONE',  ( 0.000000000000000000, 20.00000000000000000, 26.00000000000000000 ) ) ;
#44885 = CARTESIAN_POINT ( 'NONE',  ( 28.05937500061451573, 0.000000000000000000, 5.243569643749999010 ) ) ;
#44886 = CARTESIAN_POINT ( 'NONE',  ( 21.38437500061451502, -2.746126346562641984, -4.756430356249999214 ) ) ;
#44887 = CARTESIAN_POINT ( 'NONE',  ( 11.61562500061451608, 3.027376345333613106, -5.243569643749998122 ) ) ;
#44888 = CARTESIAN_POINT ( 'NONE',  ( 11.25937500061451679, 4.541064518000418104, -2.621784821874998173 ) ) ;
#44889 = ORIENTED_EDGE ( 'NONE', *, *, #2122, .F. ) ;
#44890 = CARTESIAN_POINT ( 'NONE',  ( 2.918837393651653400, -4.059695890482965197, -3.197878993417715865 ) ) ;
#44891 = CARTESIAN_POINT ( 'NONE',  ( 22.04062500061451502, 6.054752690667223547, 3.707466751127219781E-16 ) ) ;
#44892 = DIRECTION ( 'NONE',  ( 0.000000000000000000, 0.000000000000000000, 1.000000000000000000 ) ) ;
#44893 = CARTESIAN_POINT ( 'NONE',  ( 20.51249999999999574, 2.886751345948182834, 4.999999999999902300 ) ) ;
#44894 = CARTESIAN_POINT ( 'NONE',  ( 12.11250000000000249, -5.773502691896255534, -1.060575238724906372E-15 ) ) ;
#44895 = CARTESIAN_POINT ( 'NONE',  ( 22.01250000122903216, 0.000000000000000000, 4.999999999999998224 ) ) ;
#44896 = CARTESIAN_POINT ( 'NONE',  ( 17.35312500061451502, -4.541064518000417216, -2.621784821875001281 ) ) ;
#44897 = CARTESIAN_POINT ( 'NONE',  ( 12.68437500061451750, -2.746126346562646425, 4.756430356249996549 ) ) ;
#44898 = ORIENTED_EDGE ( 'NONE', *, *, #71305, .F. ) ;
#44899 = CARTESIAN_POINT ( 'NONE',  ( 19.20000000000000284, 0.000000000000000000, 4.999999999999998224 ) ) ;
#44900 = CARTESIAN_POINT ( 'NONE',  ( 24.60000000000000142, 0.000000000000000000, 4.999999999999998224 ) ) ;
#44901 = CARTESIAN_POINT ( 'NONE',  ( 21.68437500061451573, 4.541064518000418104, 2.621784821874999949 ) ) ;
#44902 = CARTESIAN_POINT ( 'NONE',  ( 26.39062500061451644, -3.027376345333610441, -5.243569643749999898 ) ) ;
#44903 = VERTEX_POINT ( 'NONE', #36165 ) ;
#44904 = DIRECTION ( 'NONE',  ( 0.000000000000000000, 0.000000000000000000, -1.000000000000000000 ) ) ;
#44905 = CARTESIAN_POINT ( 'NONE',  ( 8.953125000614518214, 4.541064518000418104, -2.621784821874998173 ) ) ;
#44906 = CARTESIAN_POINT ( 'NONE',  ( 10.98750000000000071, 5.773502691896255534, 3.535250795749688401E-16 ) ) ;
#44907 = CARTESIAN_POINT ( 'NONE',  ( 15.37500000000000000, 6.123233995736764310E-16, -4.999999999999998224 ) ) ;
#44908 = CARTESIAN_POINT ( 'NONE',  ( 7.762500001229033053, -4.330127018922190985, -2.500000000000001332 ) ) ;
#44909 = CARTESIAN_POINT ( 'NONE',  ( 5.484375000614518214, 4.541064518000418104, 2.621784821874999949 ) ) ;
#44910 = CARTESIAN_POINT ( 'NONE',  ( 28.58437500061451786, -4.541064518000419881, 2.621784821874995952 ) ) ;
#44911 = ORIENTED_EDGE ( 'NONE', *, *, #55095, .F. ) ;
#44912 = CARTESIAN_POINT ( 'NONE',  ( 24.44062500061451715, -3.027376345333614438, 5.243569643749998122 ) ) ;
#44913 = CARTESIAN_POINT ( 'NONE',  ( 26.44687500061451502, -3.027376345333610441, -5.243569643749999898 ) ) ;
#44914 = CARTESIAN_POINT ( 'NONE',  ( -2.121784821874999949, 18.82812500061459104, -33.67503911421598417 ) ) ;
#44915 = CARTESIAN_POINT ( 'NONE',  ( 12.48750000000000249, -2.886751345948129988, 4.999999999999997335 ) ) ;
#44916 = CARTESIAN_POINT ( 'NONE',  ( 10.04062500061451502, -3.027376345333614438, 5.243569643749998122 ) ) ;
#44917 = CARTESIAN_POINT ( 'NONE',  ( 29.32499999999999929, 6.123233995736764310E-16, -4.999999999999998224 ) ) ;
#44918 = CARTESIAN_POINT ( 'NONE',  ( 13.42499999999999893, -4.330127018922194537, 2.499999999999995559 ) ) ;
#44919 = CARTESIAN_POINT ( 'NONE',  ( 25.15312500061451217, 4.541064518000418104, -2.621784821874998173 ) ) ;
#44920 = CARTESIAN_POINT ( 'NONE',  ( 12.78750000122903430, 6.123233995736764310E-16, -4.999999999999998224 ) ) ;
#44921 = CARTESIAN_POINT ( 'NONE',  ( 14.14687500061451786, -2.746126346562646425, 4.756430356249996549 ) ) ;
#44922 = CARTESIAN_POINT ( 'NONE',  ( 3.815625000614518036, -6.054752690667223547, -1.112240025338166033E-15 ) ) ;
#44923 = CARTESIAN_POINT ( 'NONE',  ( 20.22187500061451715, 3.027376345333613106, -5.243569643749998122 ) ) ;
#44924 = CARTESIAN_POINT ( 'NONE',  ( -3.000416591977282496E-16, 14.34687500061451715, 25.09994784771203058 ) ) ;
#44925 = CARTESIAN_POINT ( 'NONE',  ( 21.68437500061451573, 4.541064518000418104, 2.621784821874999949 ) ) ;
#44926 = CARTESIAN_POINT ( 'NONE',  ( 3.112500000000000711, -5.773502691896255534, -1.060575238724906372E-15 ) ) ;
#44927 = CARTESIAN_POINT ( 'NONE',  ( -4.243569643749999898, 18.92187500061451644, 27.54997392385601529 ) ) ;
#44928 = CARTESIAN_POINT ( 'NONE',  ( 11.05312500061451608, -4.541064518000417216, -2.621784821875001281 ) ) ;
#44929 = LINE ( 'NONE', #35994, #71385 ) ;
#44930 = CARTESIAN_POINT ( 'NONE',  ( 6.796875000614516438, 6.054752690667223547, 3.707466751127219781E-16 ) ) ;
#44931 = CARTESIAN_POINT ( 'NONE',  ( 6.815625000614517148, 3.027376345333611329, 5.243569643749999010 ) ) ;
#44932 = CARTESIAN_POINT ( 'NONE',  ( 11.89687500061451608, -3.027376345333614438, 5.243569643749998122 ) ) ;
#44933 = CARTESIAN_POINT ( 'NONE',  ( 18.56250000122903288, -4.330127018922190985, -2.500000000000001332 ) ) ;
#44934 = CARTESIAN_POINT ( 'NONE',  ( 7.096875000614517148, -3.027376345333610441, -5.243569643749999898 ) ) ;
#44935 = CARTESIAN_POINT ( 'NONE',  ( 9.103125000614515017, 0.000000000000000000, 5.243569643749999010 ) ) ;
#44936 = CARTESIAN_POINT ( 'NONE',  ( 45.00000000000000000, 6.123233995736764310E-16, -4.999999999999998224 ) ) ;
#44937 = CARTESIAN_POINT ( 'NONE',  ( 26.49375000122903145, -2.886751345948129988, 4.999999999999997335 ) ) ;
#44938 = CARTESIAN_POINT ( 'NONE',  ( 19.43437500061451928, 4.541064518000418104, 2.621784821874999949 ) ) ;
#44939 = CARTESIAN_POINT ( 'NONE',  ( 4.471804083240662031, 2.236731597915199821, 4.552588781061169598 ) ) ;
#44940 = CARTESIAN_POINT ( 'NONE',  ( 27.36562500061451786, 3.027376345333613106, -5.243569643749998122 ) ) ;
#44941 = CARTESIAN_POINT ( 'NONE',  ( 12.81562500061451537, -6.054752690667223547, -1.112240025338166033E-15 ) ) ;
#44942 = DIRECTION ( 'NONE',  ( 0.000000000000000000, 1.000000000000000000, -0.000000000000000000 ) ) ;
#44943 = CARTESIAN_POINT ( 'NONE',  ( -4.243569643749999898, 11.72187500061451892, -32.45002607614398471 ) ) ;
#44944 = CARTESIAN_POINT ( 'NONE',  ( 12.82500000122903394, 2.886751345948129099, -4.999999999999998224 ) ) ;
#44945 = CARTESIAN_POINT ( 'NONE',  ( 27.21562500061451928, -6.054752690667223547, -1.112240025338166033E-15 ) ) ;
#44946 = EDGE_CURVE ( 'NONE', #61283, #40700, #20358, .T. ) ;
#44947 = CARTESIAN_POINT ( 'NONE',  ( -4.243569643749999898, 15.26562500061451644, -32.45002607614398471 ) ) ;
#44948 = CARTESIAN_POINT ( 'NONE',  ( 15.03750000122903252, 6.123233995736764310E-16, -4.999999999999998224 ) ) ;
#44949 = CARTESIAN_POINT ( 'NONE',  ( 12.97499999999999964, -4.330127018922194537, 2.499999999999995559 ) ) ;
#44950 = CARTESIAN_POINT ( 'NONE',  ( 21.96562500061451573, 3.027376345333613106, -5.243569643749998122 ) ) ;
#44951 = CARTESIAN_POINT ( 'NONE',  ( 6.646875000614518747, -3.027376345333610441, -5.243569643749999898 ) ) ;
#44952 = CARTESIAN_POINT ( 'NONE',  ( 8.475000001229034297, 2.886751345948126879, 4.999999999999999112 ) ) ;
#44953 = CARTESIAN_POINT ( 'NONE',  ( 16.95000000122903216, 5.773502691896255534, 3.535250795749688894E-16 ) ) ;
#44954 = CARTESIAN_POINT ( 'NONE',  ( 12.29062500061451857, -3.027376345333614438, 5.243569643749998122 ) ) ;
#44955 = CARTESIAN_POINT ( 'NONE',  ( 17.27812500061451217, -4.541064518000419881, 2.621784821874995952 ) ) ;
#44956 = CARTESIAN_POINT ( 'NONE',  ( 26.55000000122902648, -2.886751345948129988, 4.999999999999997335 ) ) ;
#44957 = CARTESIAN_POINT ( 'NONE',  ( 28.42500000122904069, -5.773502691896255534, -1.060575238724906372E-15 ) ) ;
#44958 = CARTESIAN_POINT ( 'NONE',  ( 22.08749999999999858, -2.886751345948125991, -5.000000000000000000 ) ) ;
#44959 = CARTESIAN_POINT ( 'NONE',  ( 24.75937500061451502, 4.541064518000418104, -2.621784821874998173 ) ) ;
#44960 = LINE ( 'NONE', #21682, #25247 ) ;
#44961 = CARTESIAN_POINT ( 'NONE',  ( 10.61250000122903536, 4.330127018922192761, -2.499999999999997780 ) ) ;
#44962 = CARTESIAN_POINT ( 'NONE',  ( 26.85937500061451644, -4.541064518000417216, -2.621784821875001281 ) ) ;
#44963 = CARTESIAN_POINT ( 'NONE',  ( 5.746875000614517504, -3.027376345333610441, -5.243569643749999898 ) ) ;
#44964 = CARTESIAN_POINT ( 'NONE',  ( 24.40312500061451573, 0.000000000000000000, 5.243569643749999010 ) ) ;
#44965 = CARTESIAN_POINT ( 'NONE',  ( -7.967954043666661671E-16, 15.34062499938548108, 34.33755215474603517 ) ) ;
#44966 = DIRECTION ( 'NONE',  ( -0.000000000000000000, -1.000000000000000000, -0.000000000000000000 ) ) ;
#44967 = CARTESIAN_POINT ( 'NONE',  ( 10.73437500061451644, 6.421520780324663323E-16, -5.243569643749999010 ) ) ;
#44968 = LINE ( 'NONE', #16871, #69056 ) ;
#44969 = CARTESIAN_POINT ( 'NONE',  ( 3.871875000614519280, -6.054752690667223547, -1.112240025338166033E-15 ) ) ;
#44970 = CARTESIAN_POINT ( 'NONE',  ( 7.471875000614519813, -6.054752690667223547, -1.112240025338166033E-15 ) ) ;
#44971 = CARTESIAN_POINT ( 'NONE',  ( -10.00000000000000000, 0.000000000000000000, 50.00000000000000000 ) ) ;
#44972 = CARTESIAN_POINT ( 'NONE',  ( 28.92187500061451644, 3.027376345333611329, 5.243569643749999010 ) ) ;
#44973 = CARTESIAN_POINT ( 'NONE',  ( 3.849931240356728512, 3.190302406438068505, 3.849931240356827544 ) ) ;
#44974 = CARTESIAN_POINT ( 'NONE',  ( 18.97499999999999787, 6.123233995736764310E-16, -4.999999999999998224 ) ) ;
#44975 = ORIENTED_EDGE ( 'NONE', *, *, #47376, .F. ) ;
#44976 = CARTESIAN_POINT ( 'NONE',  ( 26.13749999999999929, -2.886751345948125991, -5.000000000000000000 ) ) ;
#44977 = CARTESIAN_POINT ( 'NONE',  ( 27.60937500061451644, 0.000000000000000000, 5.243569643749999010 ) ) ;
#44978 = EDGE_CURVE ( 'NONE', #42322, #62090, #3345, .T. ) ;
#44979 = ORIENTED_EDGE ( 'NONE', *, *, #61414, .T. ) ;
#44980 = CARTESIAN_POINT ( 'NONE',  ( 16.41562500061451857, -6.054752690667223547, -1.112240025338166033E-15 ) ) ;
#44981 = CARTESIAN_POINT ( 'NONE',  ( 7.265625000614516438, 3.027376345333611329, 5.243569643749999010 ) ) ;
#44982 = CARTESIAN_POINT ( 'NONE',  ( 21.87187500061451573, 5.824947211148865298E-16, -4.756430356249998326 ) ) ;
#44983 = CARTESIAN_POINT ( 'NONE',  ( 3.571875000614517237, 3.027376345333613106, -5.243569643749998122 ) ) ;
#44984 = CARTESIAN_POINT ( 'NONE',  ( 18.56250000122903288, -4.330127018922190985, -2.500000000000001332 ) ) ;
#44985 = CARTESIAN_POINT ( 'NONE',  ( 23.73749999999999716, -2.886751345948129988, 4.999999999999997335 ) ) ;
#44986 = CARTESIAN_POINT ( 'NONE',  ( 23.92500000122903359, -5.773502691896255534, -1.060575238724906372E-15 ) ) ;
#44987 = CARTESIAN_POINT ( 'NONE',  ( 7.134375000614516793, 6.421520780324663323E-16, -5.243569643749999010 ) ) ;
#44988 = CARTESIAN_POINT ( 'NONE',  ( 12.30937500061451573, 0.000000000000000000, 5.243569643749999010 ) ) ;
#44989 = CARTESIAN_POINT ( 'NONE',  ( 22.84687500061451715, -3.027376345333610441, -5.243569643749999898 ) ) ;
#44990 = FACE_BOUND ( 'NONE', #68012, .T. ) ;
#44991 = ORIENTED_EDGE ( 'NONE', *, *, #2783, .F. ) ;
#44992 = CARTESIAN_POINT ( 'NONE',  ( 4.509375000614518569, 4.541064518000418104, -2.621784821874998173 ) ) ;
#44993 = CARTESIAN_POINT ( 'NONE',  ( 10.31250000000000355, -5.773502691896255534, -1.060575238724906372E-15 ) ) ;
#44994 = CARTESIAN_POINT ( 'NONE',  ( 8.034375000614518925, 6.421520780324663323E-16, -5.243569643749999010 ) ) ;
#44995 = CARTESIAN_POINT ( 'NONE',  ( 20.51249999999999929, 2.886751345948126879, 4.999999999999999112 ) ) ;
#44996 = CARTESIAN_POINT ( 'NONE',  ( 15.85312500061451857, 0.000000000000000000, 5.243569643749999010 ) ) ;
#44997 = CARTESIAN_POINT ( 'NONE',  ( -4.000000000000000888, 17.26249999999999929, 32.30940107675850470 ) ) ;
#44998 = DIRECTION ( 'NONE',  ( 0.000000000000000000, 0.000000000000000000, 1.000000000000000000 ) ) ;
#44999 = CARTESIAN_POINT ( 'NONE',  ( 22.73437500061451644, -4.119189519843968306, 2.378215178124996054 ) ) ;
#45000 = CARTESIAN_POINT ( 'NONE',  ( 10.97812500061451679, -4.541064518000419881, 2.621784821874995952 ) ) ;
#45001 = CARTESIAN_POINT ( 'NONE',  ( 25.92187500061451999, -6.054752690667223547, -1.112240025338166033E-15 ) ) ;
#45002 = CARTESIAN_POINT ( 'NONE',  ( 20.78732959644809952, -2.499999999999999556, -5.500000000000000000 ) ) ;
#45003 = CARTESIAN_POINT ( 'NONE',  ( 4.167140676845648706, 2.763139261668956514, -4.167140676845877856 ) ) ;
#45004 = CARTESIAN_POINT ( 'NONE',  ( 9.112500000000000711, 2.886751345948129099, -4.999999999999998224 ) ) ;
#45005 = CARTESIAN_POINT ( 'NONE',  ( -2.828200636599751609E-16, 14.60000000122903430, 25.38119784648299770 ) ) ;
#45007 =( BOUNDED_CURVE ( )  B_SPLINE_CURVE ( 2, ( #27085, #67696, #67345, #49617, #39628, #16706, #39263, #15980, #62146 ),
 .UNSPECIFIED., .F., .F. ) 
 B_SPLINE_CURVE_WITH_KNOTS ( ( 3, 2, 2, 2, 3 ),
 ( 0.07608695652173913526, 0.07971014492753622505, 0.08695652173913043237, 0.09420289855072463969, 0.09782608695652174335 ),
 .UNSPECIFIED. ) 
 CURVE ( )  GEOMETRIC_REPRESENTATION_ITEM ( )  RATIONAL_B_SPLINE_CURVE ( ( 0.9330127018922192983, 0.9330127018922194093, 1.000000000000000000, 0.8660254037844387076, 1.000000000000000000, 0.8660254037844387076, 1.000000000000000000, 0.9330127018922194093, 0.9330127018922194093 ) ) 
 REPRESENTATION_ITEM ( '' )  );
#45006 = CARTESIAN_POINT ( 'NONE',  ( 8.550000001229031810, -2.886751345948129988, 4.999999999999997335 ) ) ;
#45008 = CARTESIAN_POINT ( 'NONE',  ( 21.04687500061451644, -3.027376345333610441, -5.243569643749999898 ) ) ;
#45009 = CARTESIAN_POINT ( 'NONE',  ( 13.43437500061451750, 6.421520780324663323E-16, -5.243569643749999010 ) ) ;
#45010 = CARTESIAN_POINT ( 'NONE',  ( 3.998297483032399402, 3.002268681709985287, -4.299000508453080016 ) ) ;
#45011 = VERTEX_POINT ( 'NONE', #25818 ) ;
#45012 = CARTESIAN_POINT ( 'NONE',  ( 14.16562500061451679, -6.054752690667223547, -1.112240025338166033E-15 ) ) ;
#45013 = CARTESIAN_POINT ( 'NONE',  ( 27.22500000122903430, 2.886751345948129099, -4.999999999999998224 ) ) ;
#45014 = CARTESIAN_POINT ( 'NONE',  ( 15.42187500061451821, 3.027376345333611329, 5.243569643749999010 ) ) ;
#45015 = CARTESIAN_POINT ( 'NONE',  ( 5.681944431425972830, 8.230953001180115081, -31.96676831340010239 ) ) ;
#45016 = CARTESIAN_POINT ( 'NONE',  ( 16.30312500061451786, 0.000000000000000000, 5.243569643749999010 ) ) ;
#45017 = EDGE_CURVE ( 'NONE', #755, #47001, #53899, .T. ) ;
#45018 = CARTESIAN_POINT ( 'NONE',  ( 18.37500000000000355, -4.330127018922194537, 2.499999999999995559 ) ) ;
#45019 = CARTESIAN_POINT ( 'NONE',  ( 27.23437500061451644, -4.541064518000419881, 2.621784821874995952 ) ) ;
#45020 = CARTESIAN_POINT ( 'NONE',  ( 2.121784821875001281, 10.05312500061451608, 33.67503911421598417 ) ) ;
#45021 = CARTESIAN_POINT ( 'NONE',  ( 14.89687500061451786, 6.054752690667223547, 3.707466751127219781E-16 ) ) ;
#45022 = CARTESIAN_POINT ( 'NONE',  ( 14.96250000122903323, -4.330127018922190985, -2.500000000000001332 ) ) ;
#45023 = CARTESIAN_POINT ( 'NONE',  ( 7.396875000614519635, -2.746126346562646425, 4.756430356249996549 ) ) ;
#45024 = CARTESIAN_POINT ( 'NONE',  ( 4.243569643749999010, 18.77187500061451431, -32.45002607614398471 ) ) ;
#45025 = CARTESIAN_POINT ( 'NONE',  ( 18.38437500061451857, 6.421520780324663323E-16, -5.243569643749999010 ) ) ;
#45026 = CARTESIAN_POINT ( 'NONE',  ( 21.00000000122903288, 5.773502691896255534, 3.535250795749688894E-16 ) ) ;
#45027 = CARTESIAN_POINT ( 'NONE',  ( 13.99687500061451928, 6.054752690667223547, 3.707466751127219781E-16 ) ) ;
#45028 = CARTESIAN_POINT ( 'NONE',  ( -4.243569643749999898, 12.62187500061451928, 27.54997392385601529 ) ) ;
#45029 = CARTESIAN_POINT ( 'NONE',  ( 23.43750000122902932, -4.330127018922194537, 2.499999999999995559 ) ) ;
#45030 = CARTESIAN_POINT ( 'NONE',  ( 16.26562500061451289, 3.027376345333611329, 5.243569643749999010 ) ) ;
#45031 = VERTEX_POINT ( 'NONE', #42446 ) ;
#45032 = ORIENTED_EDGE ( 'NONE', *, *, #60829, .F. ) ;
#45033 = CARTESIAN_POINT ( 'NONE',  ( 19.83750000000000213, -2.886751345948125991, -5.000000000000000000 ) ) ;
#45034 = FACE_OUTER_BOUND ( 'NONE', #69594, .T. ) ;
#45035 = CARTESIAN_POINT ( 'NONE',  ( 22.22812500061451502, -4.541064518000419881, 2.621784821874995952 ) ) ;
#45036 = CARTESIAN_POINT ( 'NONE',  ( 3.999818103236636890, 3.000242528463000991, 29.85633969779405206 ) ) ;
#45037 = CARTESIAN_POINT ( 'NONE',  ( 14.81250000122903288, 0.000000000000000000, 4.999999999999998224 ) ) ;
#45038 = CARTESIAN_POINT ( 'NONE',  ( 21.47812500061451502, 6.421520780324663323E-16, -5.243569643749999010 ) ) ;
#45039 = CARTESIAN_POINT ( 'NONE',  ( 25.07812500061451644, 6.421520780324663323E-16, -5.243569643749999010 ) ) ;
#45040 = EDGE_CURVE ( 'NONE', #68374, #25347, #20993, .T. ) ;
#45041 = CARTESIAN_POINT ( 'NONE',  ( 5.465625000614517504, 3.027376345333611329, 5.243569643749999010 ) ) ;
#45042 = ORIENTED_EDGE ( 'NONE', *, *, #25641, .F. ) ;
#45043 = LINE ( 'NONE', #22135, #7389 ) ;
#45044 = CARTESIAN_POINT ( 'NONE',  ( -3.999999999999997335, 10.25000000122903643, -27.69059892324149530 ) ) ;
#45045 = CARTESIAN_POINT ( 'NONE',  ( 11.07187500061451679, -5.492252693125287522, -1.008910452111647106E-15 ) ) ;
#45046 = CYLINDRICAL_SURFACE ( 'NONE', #44158, 1.500000000000000444 ) ;
#45047 = CARTESIAN_POINT ( 'NONE',  ( 4.000000000000000000, 10.40000000122903501, -27.69059892324149530 ) ) ;
#45048 = CARTESIAN_POINT ( 'NONE',  ( 9.001249775931846008E-16, 18.62187500061451928, -25.09994784771203058 ) ) ;
#45049 = CARTESIAN_POINT ( 'NONE',  ( 5.925000001229033586, -5.773502691896255534, -1.060575238724906372E-15 ) ) ;
#45050 = CARTESIAN_POINT ( 'NONE',  ( 9.112500000000000711, 2.886751345948129099, -4.999999999999998224 ) ) ;
#45051 = CARTESIAN_POINT ( 'NONE',  ( 4.012500001229033053, 0.000000000000000000, 4.999999999999998224 ) ) ;
#45052 = CARTESIAN_POINT ( 'NONE',  ( 13.35937500061451821, -4.541064518000417216, -2.621784821875001281 ) ) ;
#45053 = CARTESIAN_POINT ( 'NONE',  ( 30.00000000000000000, 0.000000000000000000, 0.000000000000000000 ) ) ;
#45054 = CARTESIAN_POINT ( 'NONE',  ( 4.321875000614517681, -6.054752690667223547, -1.112240025338166033E-15 ) ) ;
#45055 = DIRECTION ( 'NONE',  ( -1.000000000000000000, -0.000000000000000000, -0.000000000000000000 ) ) ;
#45056 = CARTESIAN_POINT ( 'NONE',  ( 10.69687500061451679, -3.027376345333610441, -5.243569643749999898 ) ) ;
#45057 = CARTESIAN_POINT ( 'NONE',  ( 1.071796769724493892, 17.27990381179670010, -34.00000000000000000 ) ) ;
#45058 = CARTESIAN_POINT ( 'NONE',  ( 30.00000000000000000, 6.123233995736764310E-16, -4.999999999999998224 ) ) ;
#45059 = CARTESIAN_POINT ( 'NONE',  ( -4.243569643749999898, 17.06562500061459176, 27.54997392385601529 ) ) ;
#45060 = CARTESIAN_POINT ( 'NONE',  ( 21.00937500061451857, -4.541064518000417216, -2.621784821875001281 ) ) ;
#45061 = FILL_AREA_STYLE_COLOUR ( '', #43815 ) ;
#45062 = CARTESIAN_POINT ( 'NONE',  ( 27.90000000122903145, -2.886751345948129988, 4.999999999999997335 ) ) ;
#45063 = CARTESIAN_POINT ( 'NONE',  ( 18.64687500061451431, -4.119189519843965641, -2.378215178125001383 ) ) ;
#45064 = CARTESIAN_POINT ( 'NONE',  ( 25.97812500061451502, 6.421520780324663323E-16, -5.243569643749999010 ) ) ;
#45065 = CARTESIAN_POINT ( 'NONE',  ( 14.42812500061451786, 4.541064518000418104, 2.621784821874999949 ) ) ;
#45066 = CARTESIAN_POINT ( 'NONE',  ( 15.20625000122903181, 0.000000000000000000, 4.999999999999998224 ) ) ;
#45067 = CARTESIAN_POINT ( 'NONE',  ( 10.73437500061451644, 6.421520780324663323E-16, -5.243569643749999010 ) ) ;
#45068 = CARTESIAN_POINT ( 'NONE',  ( 29.77499999999999858, 6.123233995736764310E-16, -4.999999999999998224 ) ) ;
#45069 = CARTESIAN_POINT ( 'NONE',  ( 24.15000000122903145, 5.773502691896255534, 3.535250795749688894E-16 ) ) ;
#45070 = CARTESIAN_POINT ( 'NONE',  ( 4.321875000614517681, -6.054752690667223547, -1.112240025338166033E-15 ) ) ;
#45071 = CARTESIAN_POINT ( 'NONE',  ( 14.85937500061451644, 4.541064518000418104, -2.621784821874998173 ) ) ;
#45072 = CARTESIAN_POINT ( 'NONE',  ( 29.10937500061451644, -4.541064518000417216, -2.621784821875001281 ) ) ;
#45073 = CARTESIAN_POINT ( 'NONE',  ( -1.071796769724504328, 11.54240381056766829, 33.99999999999999289 ) ) ;
#45074 = LINE ( 'NONE', #10724, #32505 ) ;
#45075 = CARTESIAN_POINT ( 'NONE',  ( 22.24687500061451217, -3.027376345333614438, 5.243569643749998122 ) ) ;
#45076 = CARTESIAN_POINT ( 'NONE',  ( 14.85937500061451644, 4.541064518000418104, -2.621784821874998173 ) ) ;
#45077 = CARTESIAN_POINT ( 'NONE',  ( -3.756430356250001434, 16.61562499938548143, 32.16877607737301048 ) ) ;
#45078 = CARTESIAN_POINT ( 'NONE',  ( 27.86249999999999716, -5.773502691896255534, -1.060575238724906372E-15 ) ) ;
#45079 = CARTESIAN_POINT ( 'NONE',  ( 2.775000001229033675, -5.773502691896255534, -1.060575238724906372E-15 ) ) ;
#45080 = CARTESIAN_POINT ( 'NONE',  ( 7.884375000614518569, -2.746126346562642428, -4.756430356249999214 ) ) ;
#45081 = CARTESIAN_POINT ( 'NONE',  ( 17.20312500061451644, 0.000000000000000000, 5.243569643749999010 ) ) ;
#45082 = CARTESIAN_POINT ( 'NONE',  ( 7.987500000000000711, -2.886751345948129988, 4.999999999999997335 ) ) ;
#45083 = EDGE_CURVE ( 'NONE', #1870, #71251, #70881, .T. ) ;
#45084 = DIRECTION ( 'NONE',  ( -0.000000000000000000, -1.000000000000000000, -0.000000000000000000 ) ) ;
#45085 = CARTESIAN_POINT ( 'NONE',  ( 16.01249999999999929, 2.886751345948126879, 4.999999999999999112 ) ) ;
#45086 = CARTESIAN_POINT ( 'NONE',  ( -2.121784821874996840, 13.57812500061451644, 33.67503911421598417 ) ) ;
#45087 = CARTESIAN_POINT ( 'NONE',  ( 0.6945855708053418898, 20.89427347822356751, 33.93923227099254092 ) ) ;
#45088 = CARTESIAN_POINT ( 'NONE',  ( 21.15000000122903145, -2.886751345948129988, 4.999999999999997335 ) ) ;
#45089 = CARTESIAN_POINT ( 'NONE',  ( -3.999999999999999112, 13.36250000122903359, 30.00000000000000000 ) ) ;
#45090 = CARTESIAN_POINT ( 'NONE',  ( 26.44687500061451502, -3.027376345333610441, -5.243569643749999898 ) ) ;
#45091 = ORIENTED_EDGE ( 'NONE', *, *, #55867, .T. ) ;
#45092 = CARTESIAN_POINT ( 'NONE',  ( 21.89062500061451289, -3.027376345333610441, -5.243569643749999898 ) ) ;
#45093 = CARTESIAN_POINT ( 'NONE',  ( 22.43437500061451573, 6.421520780324663323E-16, -5.243569643749999010 ) ) ;
#45094 = CARTESIAN_POINT ( 'NONE',  ( 6.562500000000001776, 2.886751345948126879, 4.999999999999999112 ) ) ;
#45095 = CARTESIAN_POINT ( 'NONE',  ( 10.52812500061451750, -4.541064518000419881, 2.621784821874995952 ) ) ;
#45096 = CARTESIAN_POINT ( 'NONE',  ( 23.91562500061451502, 3.027376345333611329, 5.243569643749999010 ) ) ;
#45097 = CARTESIAN_POINT ( 'NONE',  ( 15.57187500061451679, -6.054752690667223547, -1.112240025338166033E-15 ) ) ;
#45098 = CARTESIAN_POINT ( 'NONE',  ( 19.84687500061451360, 6.054752690667223547, 3.707466751127219781E-16 ) ) ;
#45099 = DIRECTION ( 'NONE',  ( 1.000000000000000000, -0.000000000000000000, -0.000000000000000000 ) ) ;
#45100 = CARTESIAN_POINT ( 'NONE',  ( 2.121784821875001281, 17.25312500061451715, 33.67503911421598417 ) ) ;
#45101 = CARTESIAN_POINT ( 'NONE',  ( 22.16250000122903074, -4.330127018922190985, -2.500000000000001332 ) ) ;
#45102 = CARTESIAN_POINT ( 'NONE',  ( 15.83437500061451608, 4.119189519843966529, 2.378215178124999607 ) ) ;
#45103 = CARTESIAN_POINT ( 'NONE',  ( 12.89062500061451821, -3.027376345333610441, -5.243569643749999898 ) ) ;
#45104 = CARTESIAN_POINT ( 'NONE',  ( 5.821875000614519458, 3.027376345333613106, -5.243569643749998122 ) ) ;
#45105 = CARTESIAN_POINT ( 'NONE',  ( 3.721875000614518036, 3.027376345333611329, 5.243569643749999010 ) ) ;
#45106 = VERTEX_POINT ( 'NONE', #9190 ) ;
#45107 = CARTESIAN_POINT ( 'NONE',  ( 28.47187500061451715, 3.027376345333611329, 5.243569643749999010 ) ) ;
#45108 = CARTESIAN_POINT ( 'NONE',  ( 17.12812500061451715, 4.541064518000418104, 2.621784821874999949 ) ) ;
#45109 = CARTESIAN_POINT ( 'NONE',  ( 27.97500000122903074, -5.773502691896255534, -1.060575238724906372E-15 ) ) ;
#45110 = CARTESIAN_POINT ( 'NONE',  ( 27.55312500061451786, 0.000000000000000000, 5.243569643749999010 ) ) ;
#45111 = CIRCLE ( 'NONE', #66300, 1.500000000000000444 ) ;
#45112 = CARTESIAN_POINT ( 'NONE',  ( 21.79687500061451644, -3.027376345333614438, 5.243569643749998122 ) ) ;
#45113 = CARTESIAN_POINT ( 'NONE',  ( 17.80312500061451786, -4.541064518000417216, -2.621784821875001281 ) ) ;
#45114 = CARTESIAN_POINT ( 'NONE',  ( -3.999999999999999556, 10.51250000000000107, 27.69059892324149530 ) ) ;
#45115 = CARTESIAN_POINT ( 'NONE',  ( 24.10312500061451502, -4.541064518000417216, -2.621784821875001281 ) ) ;
#45116 = CARTESIAN_POINT ( 'NONE',  ( 4.050000001229035362, -2.886751345948129988, 4.999999999999997335 ) ) ;
#45117 = VERTEX_POINT ( 'NONE', #4396 ) ;
#45118 = CARTESIAN_POINT ( 'NONE',  ( 27.93750000000000000, -2.886751345948125991, -5.000000000000000000 ) ) ;
#45119 = CARTESIAN_POINT ( 'NONE',  ( 2.000000000000001332, 12.05000000000000249, -26.53589838486224650 ) ) ;
#45120 = CARTESIAN_POINT ( 'NONE',  ( -7.967954043666661671E-16, 16.69062499938548427, 34.33755215474603517 ) ) ;
#45121 = CARTESIAN_POINT ( 'NONE',  ( 4.246875000614519280, -3.027376345333614438, 5.243569643749998122 ) ) ;
#45122 = CARTESIAN_POINT ( 'NONE',  ( 9.928125000614517859, 4.541064518000418104, 2.621784821874999949 ) ) ;
#45123 = CARTESIAN_POINT ( 'NONE',  ( 7.059375000614518392, -4.541064518000417216, -2.621784821875001281 ) ) ;
#45124 = CARTESIAN_POINT ( 'NONE',  ( 25.35000000122903074, -2.886751345948125991, -5.000000000000000000 ) ) ;
#45125 = EDGE_CURVE ( 'NONE', #52599, #6077, #30299, .T. ) ;
#45126 = CARTESIAN_POINT ( 'NONE',  ( 13.80937500061451750, -4.541064518000417216, -2.621784821875001281 ) ) ;
#45127 = CARTESIAN_POINT ( 'NONE',  ( 28.75312500061451715, 4.541064518000418104, -2.621784821874998173 ) ) ;
#45128 = CARTESIAN_POINT ( 'NONE',  ( 27.82499999999999929, -4.330127018922194537, 2.499999999999995559 ) ) ;
#45129 = CARTESIAN_POINT ( 'NONE',  ( 14.47499999999999964, 6.123233995736764310E-16, -4.999999999999998224 ) ) ;
#45130 = CARTESIAN_POINT ( 'NONE',  ( 12.62812500061451537, 4.541064518000418104, 2.621784821874999949 ) ) ;
#45131 = ORIENTED_EDGE ( 'NONE', *, *, #46580, .F. ) ;
#45132 = CARTESIAN_POINT ( 'NONE',  ( 9.253125000614517148, -4.541064518000417216, -2.621784821875001281 ) ) ;
#45133 = CARTESIAN_POINT ( 'NONE',  ( 6.928125000614516082, -4.541064518000419881, 2.621784821874995952 ) ) ;
#45134 = CARTESIAN_POINT ( 'NONE',  ( 18.57187500061451857, 2.746126346562643317, 4.756430356249998326 ) ) ;
#45135 = EDGE_CURVE ( 'NONE', #51427, #5506, #15815, .T. ) ;
#45136 = DIRECTION ( 'NONE',  ( 0.000000000000000000, 8.673617379884035472E-17, 1.000000000000000000 ) ) ;
#45137 = EDGE_CURVE ( 'NONE', #7111, #29389, #3657, .T. ) ;
#45138 = CARTESIAN_POINT ( 'NONE',  ( 14.92500000000000071, 6.123233995736764310E-16, -4.999999999999998224 ) ) ;
#45139 = CARTESIAN_POINT ( 'NONE',  ( 17.10937500061451999, 4.541064518000418104, -2.621784821874998173 ) ) ;
#45140 = CARTESIAN_POINT ( 'NONE',  ( 11.17500000122903536, 2.886751345948126879, 4.999999999999999112 ) ) ;
#45141 = CARTESIAN_POINT ( 'NONE',  ( 18.86249999999999716, -5.773502691896255534, -1.060575238724906372E-15 ) ) ;
#45142 = CARTESIAN_POINT ( 'NONE',  ( 21.00937500061451857, -4.541064518000417216, -2.621784821875001281 ) ) ;
#45143 = CARTESIAN_POINT ( 'NONE',  ( -3.000416591977282496E-16, 14.29062500061451679, -34.90005215228797653 ) ) ;
#45144 = CARTESIAN_POINT ( 'NONE',  ( 34.99999999999999289, -6.363961030678960462, -6.363961030678893849 ) ) ;
#45145 = CARTESIAN_POINT ( 'NONE',  ( 26.29687500061451644, -4.119189519843965641, -2.378215178125001383 ) ) ;
#45146 = DIRECTION ( 'NONE',  ( -1.000000000000000000, -0.000000000000000000, -0.000000000000000000 ) ) ;
#45147 = CARTESIAN_POINT ( 'NONE',  ( 27.70312500061451289, -4.541064518000417216, -2.621784821875001281 ) ) ;
#45148 = CARTESIAN_POINT ( 'NONE',  ( 17.21250000122903145, -4.330127018922190985, -2.500000000000001332 ) ) ;
#45149 = CARTESIAN_POINT ( 'NONE',  ( 29.74687500061451217, 6.054752690667223547, 3.707466751127219781E-16 ) ) ;
#45150 =( BOUNDED_CURVE ( )  B_SPLINE_CURVE ( 2, ( #23131, #50502, #6153, #28682, #625, #50861, #45687, #68578, #41580 ),
 .UNSPECIFIED., .F., .F. ) 
 B_SPLINE_CURVE_WITH_KNOTS ( ( 3, 2, 2, 2, 3 ),
 ( 0.1527777777777777901, 0.1574074074074074125, 0.1666666666666666574, 0.1759259259259259300, 0.1805555555555555525 ),
 .UNSPECIFIED. ) 
 CURVE ( )  GEOMETRIC_REPRESENTATION_ITEM ( )  RATIONAL_B_SPLINE_CURVE ( ( 0.9330127018922194093, 0.9330127018922195203, 1.000000000000000000, 0.8660254037844387076, 1.000000000000000000, 0.8660254037844387076, 1.000000000000000000, 0.9330127018922194093, 0.9330127018922194093 ) ) 
 REPRESENTATION_ITEM ( '' )  );
#45151 = CARTESIAN_POINT ( 'NONE',  ( 25.16249999999999432, -5.773502691896255534, -1.060575238724906372E-15 ) ) ;
#45152 = CARTESIAN_POINT ( 'NONE',  ( 8.615625000614517859, 3.027376345333611329, 5.243569643749999010 ) ) ;
#45153 = CARTESIAN_POINT ( 'NONE',  ( 27.60937500061451644, -5.492252693125287522, -1.008910452111647106E-15 ) ) ;
#45154 = CARTESIAN_POINT ( 'NONE',  ( 18.15937500061451715, 0.000000000000000000, 5.243569643749999010 ) ) ;
#45155 = CARTESIAN_POINT ( 'NONE',  ( 11.03437500061451182, -2.746126346562641984, -4.756430356249999214 ) ) ;
#45156 = CARTESIAN_POINT ( 'NONE',  ( 4.115625000614516082, 3.027376345333611329, 5.243569643749999010 ) ) ;
#45157 = CARTESIAN_POINT ( 'NONE',  ( 9.909375000614517148, 4.541064518000418104, -2.621784821874998173 ) ) ;
#45158 = ORIENTED_EDGE ( 'NONE', *, *, #14707, .T. ) ;
#45159 = CARTESIAN_POINT ( 'NONE',  ( 21.04687500061451644, -3.027376345333610441, -5.243569643749999898 ) ) ;
#45160 = CARTESIAN_POINT ( 'NONE',  ( -1.243387493232115393E-14, 15.70624999877096784, 26.00000000000000000 ) ) ;
#45161 = CARTESIAN_POINT ( 'NONE',  ( 28.35000000000000142, -4.330127018922190985, -2.500000000000001332 ) ) ;
#45162 = CARTESIAN_POINT ( 'NONE',  ( 5.062500000000000888, 2.886751345948129099, -4.999999999999998224 ) ) ;
#45163 = CARTESIAN_POINT ( 'NONE',  ( 14.32500000122903394, 2.886751345948126879, 4.999999999999999112 ) ) ;
#45164 = CARTESIAN_POINT ( 'NONE',  ( 3.999999999999998668, 12.27500000122903501, 27.69059892324149530 ) ) ;
#45165 = CARTESIAN_POINT ( 'NONE',  ( 19.12500000000000000, 4.330127018922191873, 2.499999999999999556 ) ) ;
#45166 = ORIENTED_EDGE ( 'NONE', *, *, #15334, .F. ) ;
#45167 = CARTESIAN_POINT ( 'NONE',  ( 12.11250000000000249, -5.773502691896255534, -1.060575238724906372E-15 ) ) ;
#45168 = CARTESIAN_POINT ( 'NONE',  ( 23.50312500061451360, 0.000000000000000000, 5.243569643749999010 ) ) ;
#45169 = CARTESIAN_POINT ( 'NONE',  ( 17.77499999999999858, 4.330127018922191873, 2.499999999999999556 ) ) ;
#45170 = CARTESIAN_POINT ( 'NONE',  ( 9.750000001229032875, 5.773502691896255534, 3.535250795749688894E-16 ) ) ;
#45171 = CARTESIAN_POINT ( 'NONE',  ( 9.553125000614517859, 0.000000000000000000, 5.243569643749999010 ) ) ;
#45172 = CARTESIAN_POINT ( 'NONE',  ( 9.375000000000001776, -4.330127018922194537, 2.499999999999995559 ) ) ;
#45173 = CARTESIAN_POINT ( 'NONE',  ( 30.00000000000000000, 0.000000000000000000, 0.000000000000000000 ) ) ;
#45174 = CARTESIAN_POINT ( 'NONE',  ( -4.243569643749999898, 14.00937500061451857, -30.00000000000000000 ) ) ;
#45175 = CARTESIAN_POINT ( 'NONE',  ( 28.76250000122903216, 0.000000000000000000, 4.999999999999998224 ) ) ;
#45176 = CARTESIAN_POINT ( 'NONE',  ( 1.878215178124997609, 13.91562499938548392, 33.25316411605952993 ) ) ;
#45177 = CARTESIAN_POINT ( 'NONE',  ( 8.099999999999999645, -4.330127018922190985, -2.500000000000001332 ) ) ;
#45178 = FACE_OUTER_BOUND ( 'NONE', #49424, .T. ) ;
#45179 = ORIENTED_EDGE ( 'NONE', *, *, #27906, .F. ) ;
#45180 = CARTESIAN_POINT ( 'NONE',  ( 23.87812500061451715, 4.541064518000418104, 2.621784821874999949 ) ) ;
#45181 = CARTESIAN_POINT ( 'NONE',  ( 14.25000000122903465, 5.773502691896255534, 3.535250795749688894E-16 ) ) ;
#45182 = CARTESIAN_POINT ( 'NONE',  ( 29.54062500061451502, -3.027376345333610441, -5.243569643749999898 ) ) ;
#45183 = CARTESIAN_POINT ( 'NONE',  ( 18.75937500061451857, -4.541064518000417216, -2.621784821875001281 ) ) ;
#45184 = CARTESIAN_POINT ( 'NONE',  ( 17.76562500061451644, -6.054752690667223547, -1.112240025338166033E-15 ) ) ;
#45185 = CARTESIAN_POINT ( 'NONE',  ( 4.243569643749999898, 12.34062500061459389, -27.54997392385601529 ) ) ;
#45186 = CARTESIAN_POINT ( 'NONE',  ( 6.290625000614517681, 6.054752690667223547, 3.707466751127219781E-16 ) ) ;
#45187 = CARTESIAN_POINT ( 'NONE',  ( 28.27500000122903145, 2.886751345948126879, 4.999999999999999112 ) ) ;
#45188 = CARTESIAN_POINT ( 'NONE',  ( 21.00937500061451857, -4.119189519843965641, -2.378215178125001383 ) ) ;
#45189 = CARTESIAN_POINT ( 'NONE',  ( 20.01562500061451644, -6.054752690667223547, -1.112240025338166033E-15 ) ) ;
#45190 = CYLINDRICAL_SURFACE ( 'NONE', #57468, 4.999999999999998224 ) ;
#45191 = CARTESIAN_POINT ( 'NONE',  ( -3.756430356250001434, 17.85312499938548214, 32.16877607737301048 ) ) ;
#45192 = CARTESIAN_POINT ( 'NONE',  ( 13.43437500061451750, 6.421520780324663323E-16, -5.243569643749999010 ) ) ;
#45193 = CARTESIAN_POINT ( 'NONE',  ( 12.12187500061451573, 3.027376345333613106, -5.243569643749998122 ) ) ;
#45194 = CARTESIAN_POINT ( 'NONE',  ( 20.78437500061451715, 4.541064518000418104, 2.621784821874999949 ) ) ;
#45195 = ORIENTED_EDGE ( 'NONE', *, *, #21528, .T. ) ;
#45196 = CARTESIAN_POINT ( 'NONE',  ( 27.15000000000000213, 4.330127018922192761, -2.499999999999997780 ) ) ;
#45197 = CARTESIAN_POINT ( 'NONE',  ( 27.29062500061451502, -3.027376345333610441, -5.243569643749999898 ) ) ;
#45198 = CARTESIAN_POINT ( 'NONE',  ( 23.69062500061451004, -3.027376345333610441, -5.243569643749999898 ) ) ;
#45199 = LINE ( 'NONE', #12288, #36817 ) ;
#45200 = CARTESIAN_POINT ( 'NONE',  ( 2.000000000000001332, 17.89999999999999858, 33.46410161513774995 ) ) ;
#45201 = CARTESIAN_POINT ( 'NONE',  ( 3.909375000614518481, -4.541064518000417216, -2.621784821875001281 ) ) ;
#45202 = CARTESIAN_POINT ( 'NONE',  ( 11.21250000122903501, 0.000000000000000000, 4.999999999999998224 ) ) ;
#45203 = CARTESIAN_POINT ( 'NONE',  ( 6.600000001229032520, 5.773502691896255534, 3.535250795749688894E-16 ) ) ;
#45204 = CARTESIAN_POINT ( 'NONE',  ( 21.75000000122903288, -2.886751345948159742, -4.999999999999942268 ) ) ;
#45205 = CARTESIAN_POINT ( 'NONE',  ( 3.103125000614517237, 4.541064518000418104, -2.621784821874998173 ) ) ;
#45206 = CARTESIAN_POINT ( 'NONE',  ( -4.000000000000000000, 18.06874999877096855, 30.00000000000000000 ) ) ;
#45207 = CARTESIAN_POINT ( 'NONE',  ( 15.69375000122903074, -2.886751345948129988, 4.999999999999997335 ) ) ;
#45208 = CARTESIAN_POINT ( 'NONE',  ( 12.53437500061451537, 6.421520780324663323E-16, -5.243569643749999010 ) ) ;
#45209 = DIRECTION ( 'NONE',  ( 0.000000000000000000, 0.000000000000000000, -1.000000000000000000 ) ) ;
#45210 = CARTESIAN_POINT ( 'NONE',  ( 16.75312500061451715, 0.000000000000000000, 5.243569643749999010 ) ) ;
#45211 = CARTESIAN_POINT ( 'NONE',  ( 13.05937500061451750, 4.541064518000418104, -2.621784821874998173 ) ) ;
#45212 = CARTESIAN_POINT ( 'NONE',  ( 5.353125000614515905, 4.541064518000418104, -2.621784821874998173 ) ) ;
#45213 = CARTESIAN_POINT ( 'NONE',  ( 22.43437500061451573, 6.421520780324663323E-16, -5.243569643749999010 ) ) ;
#45214 = CARTESIAN_POINT ( 'NONE',  ( 8.709375000614517859, 0.000000000000000000, 5.243569643749999010 ) ) ;
#45215 = CARTESIAN_POINT ( 'NONE',  ( 5.165625000614518569, -6.054752690667223547, -1.112240025338166033E-15 ) ) ;
#45216 = CARTESIAN_POINT ( 'NONE',  ( 11.81250000122903465, -4.330127018922190985, -2.500000000000001332 ) ) ;
#45217 = CARTESIAN_POINT ( 'NONE',  ( 5.325000001229033941, 2.886751345948126879, 4.999999999999999112 ) ) ;
#45218 =( BOUNDED_CURVE ( )  B_SPLINE_CURVE ( 2, ( #43357, #53331, #70685, #13804, #20802, #19328, #25990, #37799, #60319 ),
 .UNSPECIFIED., .F., .F. ) 
 B_SPLINE_CURVE_WITH_KNOTS ( ( 3, 2, 2, 2, 3 ),
 ( 0.1805555555555555525, 0.1851851851851851749, 0.1944444444444444475, 0.2037037037037036924, 0.2083333333333333426 ),
 .UNSPECIFIED. ) 
 CURVE ( )  GEOMETRIC_REPRESENTATION_ITEM ( )  RATIONAL_B_SPLINE_CURVE ( ( 0.9330127018922194093, 0.9330127018922194093, 1.000000000000000000, 0.8660254037844387076, 1.000000000000000000, 0.8660254037844387076, 1.000000000000000000, 0.9330127018922191873, 0.9330127018922194093 ) ) 
 REPRESENTATION_ITEM ( '' )  );
#45219 = CARTESIAN_POINT ( 'NONE',  ( 20.69062500061451715, 6.054752690667223547, 3.707466751127219781E-16 ) ) ;
#45220 = CARTESIAN_POINT ( 'NONE',  ( 7.837500001229035007, 6.123233995736764310E-16, -4.999999999999998224 ) ) ;
#45221 = CARTESIAN_POINT ( 'NONE',  ( 17.80312500061451786, -4.541064518000417216, -2.621784821875001281 ) ) ;
#45222 = CARTESIAN_POINT ( 'NONE',  ( 13.34062500061451750, -3.027376345333610441, -5.243569643749999898 ) ) ;
#45223 = CARTESIAN_POINT ( 'NONE',  ( 26.74687500061451573, -2.746126346562646425, 4.756430356249996549 ) ) ;
#45224 = CARTESIAN_POINT ( 'NONE',  ( 13.23750000000000071, 5.773502691896255534, 3.535250795749688894E-16 ) ) ;
#45225 = CARTESIAN_POINT ( 'NONE',  ( 8.850000001229034297, 5.773502691896255534, 3.535250795749688894E-16 ) ) ;
#45226 = CARTESIAN_POINT ( 'NONE',  ( 5.840625000614516615, 6.054752690667223547, 3.707466751127219781E-16 ) ) ;
#45227 = CARTESIAN_POINT ( 'NONE',  ( 20.85000000122903430, -2.886751345948125991, -5.000000000000000000 ) ) ;
#45228 = CARTESIAN_POINT ( 'NONE',  ( 28.01249999999999574, 2.886751345948129099, -4.999999999999998224 ) ) ;
#45229 = CARTESIAN_POINT ( 'NONE',  ( 4.243569643749999010, 10.67187500061451644, -32.45002607614398471 ) ) ;
#45230 = CARTESIAN_POINT ( 'NONE',  ( 9.787499999999999645, -2.886751345948130876, 4.999999999999996447 ) ) ;
#45231 = EDGE_CURVE ( 'NONE', #6912, #7983, #21358, .T. ) ;
#45232 = CARTESIAN_POINT ( 'NONE',  ( 1.626862140677534273E-15, 11.67500000122903181, -26.00000000000000355 ) ) ;
#45233 = CARTESIAN_POINT ( 'NONE',  ( 9.562500001229032875, -4.330127018922190985, -2.500000000000001332 ) ) ;
#45234 = CARTESIAN_POINT ( 'NONE',  ( 20.55937500061451573, -4.541064518000417216, -2.621784821875001281 ) ) ;
#45235 = CARTESIAN_POINT ( 'NONE',  ( 4.000000000000000000, 18.50000000122903288, 32.30940107675849760 ) ) ;
#45236 = CARTESIAN_POINT ( 'NONE',  ( 16.90312500061451573, -4.541064518000417216, -2.621784821875001281 ) ) ;
#45237 = CARTESIAN_POINT ( 'NONE',  ( 10.81875000122903252, -5.773502691896255534, -1.060575238724906372E-15 ) ) ;
#45238 = CARTESIAN_POINT ( 'NONE',  ( 1.592000809091587073E-14, 15.38750000000000284, -34.00000000000000000 ) ) ;
#45239 = CARTESIAN_POINT ( 'NONE',  ( 4.406803030766965001, -3.629725346580264578, 3.713131282202427830 ) ) ;
#45240 = CARTESIAN_POINT ( 'NONE',  ( 25.20937500061451431, 4.541064518000418104, -2.621784821874998173 ) ) ;
#45241 = CARTESIAN_POINT ( 'NONE',  ( 20.37187500061451217, -4.119189519843968306, 2.378215178124996054 ) ) ;
#45242 = CARTESIAN_POINT ( 'NONE',  ( 11.46562500061451573, -6.054752690667223547, -1.112240025338166033E-15 ) ) ;
#45243 = CARTESIAN_POINT ( 'NONE',  ( 9.909375000614517148, 4.541064518000418104, -2.621784821874998173 ) ) ;
#45244 = ORIENTED_EDGE ( 'NONE', *, *, #14641, .F. ) ;
#45245 = CARTESIAN_POINT ( 'NONE',  ( 29.20312500061451644, 4.541064518000418104, -2.621784821874998173 ) ) ;
#45246 = CARTESIAN_POINT ( 'NONE',  ( 23.61562500061451431, -6.054752690667223547, -1.112240025338166033E-15 ) ) ;
#45247 = DIRECTION ( 'NONE',  ( -1.000000000000000000, -0.000000000000000000, -0.000000000000000000 ) ) ;
#45248 = CARTESIAN_POINT ( 'NONE',  ( 1.071796769724489895, 15.47990381179670116, -34.00000000000000000 ) ) ;
#45249 = EDGE_CURVE ( 'NONE', #66380, #47866, #56209, .T. ) ;
#45250 = CARTESIAN_POINT ( 'NONE',  ( 12.37500000000000000, 4.330127018922191873, 2.499999999999999556 ) ) ;
#45251 = CARTESIAN_POINT ( 'NONE',  ( 22.76250000122903216, 4.330127018922192761, -2.499999999999997780 ) ) ;
#45252 = CARTESIAN_POINT ( 'NONE',  ( 17.16562500061451502, 3.027376345333611329, 5.243569643749999010 ) ) ;
#45253 = CARTESIAN_POINT ( 'NONE',  ( 12.94687500061451502, 4.119189519843966529, -2.378215178124998275 ) ) ;
#45254 = ORIENTED_EDGE ( 'NONE', *, *, #893, .T. ) ;
#45255 = CARTESIAN_POINT ( 'NONE',  ( 21.07499999999999929, -4.330127018922194537, 2.499999999999995559 ) ) ;
#45256 = CARTESIAN_POINT ( 'NONE',  ( 23.77499999999999858, -4.330127018922194537, 2.499999999999995559 ) ) ;
#45257 = CARTESIAN_POINT ( 'NONE',  ( 21.15937500061451715, 4.541064518000418104, -2.621784821874998173 ) ) ;
#45258 = CARTESIAN_POINT ( 'NONE',  ( 25.90312500061451573, -4.541064518000417216, -2.621784821875001281 ) ) ;
#45259 = ADVANCED_FACE ( 'NONE', ( #14720 ), #20255, .F. ) ;
#45260 = ORIENTED_EDGE ( 'NONE', *, *, #1978, .F. ) ;
#45261 = CARTESIAN_POINT ( 'NONE',  ( 0.000000000000000000, 20.00000000000000000, 30.00000000000000000 ) ) ;
#45262 = CARTESIAN_POINT ( 'NONE',  ( 8.615625000614517859, 3.027376345333611329, 5.243569643749999010 ) ) ;
#45263 = CARTESIAN_POINT ( 'NONE',  ( 23.92499999999999716, 6.123233995736764310E-16, -4.999999999999998224 ) ) ;
#45264 = CARTESIAN_POINT ( 'NONE',  ( 15.59999999999999964, 0.000000000000000000, 4.999999999999998224 ) ) ;
#45265 = CARTESIAN_POINT ( 'NONE',  ( -4.243569643749997233, 17.14062500061451644, 32.45002607614398471 ) ) ;
#45266 = CARTESIAN_POINT ( 'NONE',  ( 5.596875000614516260, -3.027376345333614438, 5.243569643749998122 ) ) ;
#45267 = CARTESIAN_POINT ( 'NONE',  ( 27.15937500061451360, 0.000000000000000000, 5.243569643749999010 ) ) ;
#45268 = ORIENTED_EDGE ( 'NONE', *, *, #19563, .F. ) ;
#45269 = CARTESIAN_POINT ( 'NONE',  ( 23.12812500061451360, -4.541064518000419881, 2.621784821874995952 ) ) ;
#45270 = CARTESIAN_POINT ( 'NONE',  ( 24.94687500061451502, -3.027376345333614438, 5.243569643749998122 ) ) ;
#45271 = CARTESIAN_POINT ( 'NONE',  ( -2.121784821874999949, 19.72812500061459318, -33.67503911421598417 ) ) ;
#45272 = CARTESIAN_POINT ( 'NONE',  ( 12.26249999999999929, 2.886751345948129099, -4.999999999999998224 ) ) ;
#45273 = CARTESIAN_POINT ( 'NONE',  ( 9.440625000614517148, 6.054752690667223547, 3.707466751127219781E-16 ) ) ;
#45274 = LINE ( 'NONE', #32731, #42178 ) ;
#45275 = DIRECTION ( 'NONE',  ( -0.000000000000000000, -1.000000000000000000, -0.000000000000000000 ) ) ;
#45276 = CARTESIAN_POINT ( 'NONE',  ( 27.25312500061451360, -4.541064518000417216, -2.621784821875001281 ) ) ;
#45277 = CARTESIAN_POINT ( 'NONE',  ( 29.14687500061451431, 4.119189519843966529, -2.378215178124998275 ) ) ;
#45278 = CARTESIAN_POINT ( 'NONE',  ( 11.82187500061451679, 2.746126346562643317, 4.756430356249998326 ) ) ;
#45279 = CARTESIAN_POINT ( 'NONE',  ( 2.878125000614517592, -4.541064518000419881, 2.621784821874995952 ) ) ;
#45280 = CARTESIAN_POINT ( 'NONE',  ( 20.48437500061451289, -4.541064518000419881, 2.621784821874995952 ) ) ;
#45281 = CARTESIAN_POINT ( 'NONE',  ( 2.121784821875001281, 14.15937500061451715, 33.67503911421598417 ) ) ;
#45282 = CARTESIAN_POINT ( 'NONE',  ( 19.39687500061451786, 6.054752690667223547, 3.707466751127219781E-16 ) ) ;
#45283 = CARTESIAN_POINT ( 'NONE',  ( 3.450000000000001510, 0.000000000000000000, 4.999999999999998224 ) ) ;
#45284 = CARTESIAN_POINT ( 'NONE',  ( -2.121784821874999949, 18.43437500061451928, 26.32496088578401938 ) ) ;
#45285 = CARTESIAN_POINT ( 'NONE',  ( 11.01562500061451821, -6.054752690667223547, -1.112240025338166033E-15 ) ) ;
#45286 = CARTESIAN_POINT ( 'NONE',  ( 14.47499999999999964, 6.123233995736764310E-16, -4.999999999999998224 ) ) ;
#45287 = CARTESIAN_POINT ( 'NONE',  ( 8.184375000614515727, 4.541064518000418104, 2.621784821874999949 ) ) ;
#45288 = CYLINDRICAL_SURFACE ( 'NONE', #49013, 4.000000000000000000 ) ;
#45289 = CARTESIAN_POINT ( 'NONE',  ( 8.203125000614518214, 0.000000000000000000, 5.243569643749999010 ) ) ;
#45290 = CARTESIAN_POINT ( 'NONE',  ( 12.00937500061451857, -4.541064518000417216, -2.621784821875001281 ) ) ;
#45291 = CARTESIAN_POINT ( 'NONE',  ( 19.27500000122903145, 2.886751345948126879, 4.999999999999999112 ) ) ;
#45292 = CARTESIAN_POINT ( 'NONE',  ( 7.884375000614517681, -4.541064518000419881, 2.621784821874995952 ) ) ;
#45293 = CARTESIAN_POINT ( 'NONE',  ( 9.665625000614515017, -6.054752690667223547, -1.112240025338166033E-15 ) ) ;
#45294 = DIRECTION ( 'NONE',  ( -1.000000000000000000, -0.000000000000000000, -0.000000000000000000 ) ) ;
#45295 = CARTESIAN_POINT ( 'NONE',  ( 22.59375000122903288, -2.886751345948125991, -5.000000000000000000 ) ) ;
#45296 = CARTESIAN_POINT ( 'NONE',  ( 19.69687500061451857, -3.027376345333610441, -5.243569643749999898 ) ) ;
#45297 = CARTESIAN_POINT ( 'NONE',  ( -0.7368805616696194605, 9.859898480082234684, -34.17910162106521454 ) ) ;
#45298 = ORIENTED_EDGE ( 'NONE', *, *, #44604, .F. ) ;
#45299 = CARTESIAN_POINT ( 'NONE',  ( 26.27812500061451573, -4.541064518000419881, 2.621784821874995952 ) ) ;
#45300 = CARTESIAN_POINT ( 'NONE',  ( 12.96562500061451750, 3.027376345333613106, -5.243569643749998122 ) ) ;
#45301 = CARTESIAN_POINT ( 'NONE',  ( 28.80937500061451573, 4.541064518000418104, -2.621784821874998173 ) ) ;
#45302 = CARTESIAN_POINT ( 'NONE',  ( 12.47812500061451502, 6.421520780324663323E-16, -5.243569643749999010 ) ) ;
#45303 = CARTESIAN_POINT ( 'NONE',  ( 25.33125000122903003, 6.123233995736764310E-16, -4.999999999999998224 ) ) ;
#45304 = CARTESIAN_POINT ( 'NONE',  ( 13.65000000122903323, -2.886751345948125991, -5.000000000000000000 ) ) ;
#45305 = CARTESIAN_POINT ( 'NONE',  ( 26.69062500061451715, -3.027376345333614438, 5.243569643749998122 ) ) ;
#45306 = CARTESIAN_POINT ( 'NONE',  ( 4.243569643749999898, 14.62812500061451715, -30.00000000000000000 ) ) ;
#45307 = CARTESIAN_POINT ( 'NONE',  ( 15.18750000122903465, 4.330127018922191873, 2.499999999999999556 ) ) ;
#45308 = CARTESIAN_POINT ( 'NONE',  ( 12.44999999999999929, 0.000000000000000000, 4.999999999999998224 ) ) ;
#45309 = B_SPLINE_CURVE_WITH_KNOTS ( 'NONE', 3,
 ( #52041, #36497, #8061, #64571, #29146, #53122, #13588, #52401, #7693, #24317, #19124, #51681, #1085, #46138, #69405, #46866, #18760, #18039, #63835, #40595, #35044, #63116, #46500, #12870, #35402, #41678, #36135, #13227, #30231, #47585, #52763, #19490, #70114, #2166, #24677, #58654, #2521, #26146, #25786, #26519, #60477, #37226, #3992, #36861, #3624, #2883 ),
 .UNSPECIFIED., .F., .F.,
 ( 4, 2, 2, 2, 2, 2, 2, 2, 2, 2, 2, 2, 2, 2, 2, 2, 2, 2, 2, 2, 2, 2, 4 ),
 ( 0.000000000000000000, 0.001203096460345616731, 0.002406192920691233462, 0.003609289381036850410, 0.004812385841382466924, 0.005413934071555267374, 0.006015482301728067825, 0.007218578762073687809, 0.008421675222419306925, 0.009023223452592120386, 0.009624771682764935582, 0.01082786814311056250, 0.01142941637328337770, 0.01203096460345619116, 0.01323406106380183023, 0.01443715752414746756, 0.01503870575432028275, 0.01564025398449309795, 0.01684335044483871446, 0.01744489867501152619, 0.01804644690518434139, 0.01864799513535714964, 0.01924954336552996484 ),
 .UNSPECIFIED. ) ;
#45310 = CARTESIAN_POINT ( 'NONE',  ( 20.69062500061451715, 6.054752690667223547, 3.707466751127219781E-16 ) ) ;
#45311 = CARTESIAN_POINT ( 'NONE',  ( 7.846875000614518036, -3.027376345333614438, 5.243569643749998122 ) ) ;
#45312 = CARTESIAN_POINT ( 'NONE',  ( 7.350000001229033408, -2.886751345948125991, -5.000000000000000000 ) ) ;
#45313 = CARTESIAN_POINT ( 'NONE',  ( 16.27500000122903501, -5.773502691896255534, -1.060575238724906372E-15 ) ) ;
#45314 = CARTESIAN_POINT ( 'NONE',  ( 12.81562500061451537, -6.054752690667223547, -1.112240025338166033E-15 ) ) ;
#45315 = CARTESIAN_POINT ( 'NONE',  ( 15.36562500061451608, 3.027376345333611329, 5.243569643749999010 ) ) ;
#45316 = CARTESIAN_POINT ( 'NONE',  ( 29.13750000122903216, 4.330127018922191873, 2.499999999999999556 ) ) ;
#45317 = CARTESIAN_POINT ( 'NONE',  ( 21.67500000000000071, 6.123233995736764310E-16, -4.999999999999998224 ) ) ;
#45318 = AXIS2_PLACEMENT_3D ( 'NONE', #29856, #52392, #46856 ) ;
#45319 = CARTESIAN_POINT ( 'NONE',  ( 24.12187500061451217, -6.054752690667223547, -1.112240025338166033E-15 ) ) ;
#45320 = CARTESIAN_POINT ( 'NONE',  ( 12.05625000122903145, 0.000000000000000000, 4.999999999999998224 ) ) ;
#45321 = CARTESIAN_POINT ( 'NONE',  ( 10.01250000122903394, -4.330127018922190985, -2.500000000000001332 ) ) ;
#45322 = CARTESIAN_POINT ( 'NONE',  ( 27.64687500061452141, -3.027376345333614438, 5.243569643749998122 ) ) ;
#45323 = CARTESIAN_POINT ( 'NONE',  ( 5.446875000614518569, 6.054752690667223547, 3.707466751127219781E-16 ) ) ;
#45324 = CARTESIAN_POINT ( 'NONE',  ( 23.20312500061451644, -4.541064518000417216, -2.621784821875001281 ) ) ;
#45325 = CARTESIAN_POINT ( 'NONE',  ( 3.756430356250000546, 15.04062499938548392, 27.83122392262697886 ) ) ;
#45326 = CARTESIAN_POINT ( 'NONE',  ( 6.899999999999999467, 4.330127018922192761, -2.499999999999997780 ) ) ;
#45327 = CARTESIAN_POINT ( 'NONE',  ( 11.25937500061451679, 4.541064518000418104, -2.621784821874998173 ) ) ;
#45328 = DIRECTION ( 'NONE',  ( 0.000000000000000000, -1.000000000000000000, 0.000000000000000000 ) ) ;
#45329 = CARTESIAN_POINT ( 'NONE',  ( 29.05312500061451431, -4.541064518000417216, -2.621784821875001281 ) ) ;
#45330 = CARTESIAN_POINT ( 'NONE',  ( 5.821875000614519458, 3.027376345333613106, -5.243569643749998122 ) ) ;
#45331 = MANIFOLD_SOLID_BREP ( 'Cut-Extrude1', #38304 ) ;
#45332 = CARTESIAN_POINT ( 'NONE',  ( -3.999999999999999112, 14.56250000000000000, 27.69059892324149885 ) ) ;
#45333 = CARTESIAN_POINT ( 'NONE',  ( 26.44687500061451502, -3.027376345333610441, -5.243569643749999898 ) ) ;
#45334 = CARTESIAN_POINT ( 'NONE',  ( 2.121784821875001281, 10.95312500061459460, 33.67503911421598417 ) ) ;
#45335 = CARTESIAN_POINT ( 'NONE',  ( 18.48750000000000071, -2.886751345948125991, -5.000000000000000000 ) ) ;
#45336 = ORIENTED_EDGE ( 'NONE', *, *, #52747, .T. ) ;
#45337 = CARTESIAN_POINT ( 'NONE',  ( 27.52500000000000213, 6.123233995736764310E-16, -4.999999999999998224 ) ) ;
#45338 = CARTESIAN_POINT ( 'NONE',  ( 28.47187500061451715, 3.027376345333611329, 5.243569643749999010 ) ) ;
#45339 = EDGE_CURVE ( 'NONE', #40669, #38622, #37850, .T. ) ;
#45340 = VERTEX_POINT ( 'NONE', #44282 ) ;
#45341 = CARTESIAN_POINT ( 'NONE',  ( 15.44062500061451537, -3.027376345333614438, 5.243569643749998122 ) ) ;
#45342 = CARTESIAN_POINT ( 'NONE',  ( 8.128125000614515372, 4.541064518000418104, 2.621784821874999949 ) ) ;
#45343 = CARTESIAN_POINT ( 'NONE',  ( 19.65937500061451360, 2.746126346562645981, -4.756430356249997438 ) ) ;
#45344 = CARTESIAN_POINT ( 'NONE',  ( 5.371875000614516615, 3.027376345333613106, -5.243569643749998122 ) ) ;
#45345 = CARTESIAN_POINT ( 'NONE',  ( 18.60000000122903430, -2.886751345948125991, -5.000000000000000000 ) ) ;
#45346 = CARTESIAN_POINT ( 'NONE',  ( 22.94999999999999929, -4.330127018922190985, -2.500000000000001332 ) ) ;
#45347 = DIRECTION ( 'NONE',  ( 0.000000000000000000, 0.000000000000000000, 1.000000000000000000 ) ) ;
#45348 = CARTESIAN_POINT ( 'NONE',  ( 7.209375000614519635, 4.541064518000418104, -2.621784821874998173 ) ) ;
#45349 = CARTESIAN_POINT ( 'NONE',  ( 10.77187500061451786, 3.027376345333613106, -5.243569643749998122 ) ) ;
#45350 = CARTESIAN_POINT ( 'NONE',  ( 21.49687500061451573, -3.027376345333610441, -5.243569643749999898 ) ) ;
#45351 = CARTESIAN_POINT ( 'NONE',  ( 3.999999999999998668, 15.87500000122903465, -32.30940107675850470 ) ) ;
#45352 = VERTEX_POINT ( 'NONE', #666 ) ;
#45353 = CARTESIAN_POINT ( 'NONE',  ( 4.696875000614518569, -3.027376345333614438, 5.243569643749998122 ) ) ;
#45354 = CARTESIAN_POINT ( 'NONE',  ( 7.771875000614516971, 3.027376345333611329, 5.243569643749999010 ) ) ;
#45355 = CARTESIAN_POINT ( 'NONE',  ( 18.93750000000000000, -2.886751345948125991, -5.000000000000000000 ) ) ;
#45356 = CARTESIAN_POINT ( 'NONE',  ( 16.56562500061451715, 3.027376345333613106, -5.243569643749998122 ) ) ;
#45357 = CARTESIAN_POINT ( 'NONE',  ( -4.000000000000000000, 18.57500000000000284, 30.00000000000000000 ) ) ;
#45358 = CARTESIAN_POINT ( 'NONE',  ( 18.14999999999999858, 4.330127018922192761, -2.499999999999997780 ) ) ;
#45359 = CARTESIAN_POINT ( 'NONE',  ( 21.00937500061451857, -4.119189519843965641, -2.378215178125001383 ) ) ;
#45360 = CARTESIAN_POINT ( 'NONE',  ( 10.64062500061451644, -3.027376345333610441, -5.243569643749999898 ) ) ;
#45361 = CARTESIAN_POINT ( 'NONE',  ( 25.84687500061451360, -3.027376345333614438, 5.243569643749998122 ) ) ;
#45362 = CARTESIAN_POINT ( 'NONE',  ( 27.75937500061451502, -4.541064518000417216, -2.621784821875001281 ) ) ;
#45363 = CARTESIAN_POINT ( 'NONE',  ( 10.91250000000000320, 2.886751345948129099, -4.999999999999998224 ) ) ;
#45364 = CARTESIAN_POINT ( 'NONE',  ( 4.000000000000000000, 14.45000000122903572, 32.30940107675849049 ) ) ;
#45365 = CARTESIAN_POINT ( 'NONE',  ( 8.400000001229035007, 5.773502691896255534, 3.535250795749688894E-16 ) ) ;
#45366 = CARTESIAN_POINT ( 'NONE',  ( 20.74687500061451573, 6.054752690667223547, 3.707466751127219781E-16 ) ) ;
#45367 = CARTESIAN_POINT ( 'NONE',  ( 14.85937500061451644, 4.541064518000418104, -2.621784821874998173 ) ) ;
#45368 = CARTESIAN_POINT ( 'NONE',  ( -3.780580586577212632, 3.275490995243299341, -31.33113147093461492 ) ) ;
#45369 = ORIENTED_EDGE ( 'NONE', *, *, #25127, .T. ) ;
#45370 = AXIS2_PLACEMENT_3D ( 'NONE', #23043, #58828, #13772 ) ;
#45371 = CARTESIAN_POINT ( 'NONE',  ( 15.14062500061451644, -3.027376345333610441, -5.243569643749999898 ) ) ;
#45372 = CARTESIAN_POINT ( 'NONE',  ( 26.66250000122903430, -4.330127018922190985, -2.500000000000001332 ) ) ;
#45373 = CARTESIAN_POINT ( 'NONE',  ( 15.83437500061451608, 4.541064518000418104, 2.621784821874999949 ) ) ;
#45374 = CARTESIAN_POINT ( 'NONE',  ( 3.515625000614516882, 3.027376345333613106, -5.243569643749998122 ) ) ;
#45375 = CARTESIAN_POINT ( 'NONE',  ( 17.09062500061451573, 6.054752690667223547, 3.707466751127219781E-16 ) ) ;
#45376 = CARTESIAN_POINT ( 'NONE',  ( 5.810221930991193690E-16, 20.20624999877096428, 26.00000000000000000 ) ) ;
#45377 = CARTESIAN_POINT ( 'NONE',  ( 25.80937500061451928, 0.000000000000000000, 5.243569643749999010 ) ) ;
#45378 = CARTESIAN_POINT ( 'NONE',  ( -4.243569643749999898, 9.903125000614517504, 30.00000000000000000 ) ) ;
#45379 = CARTESIAN_POINT ( 'NONE',  ( 15.53437500061451715, -4.541064518000419881, 2.621784821874995952 ) ) ;
#45380 = CARTESIAN_POINT ( 'NONE',  ( 13.83750000122903323, 4.330127018922191873, 2.499999999999999556 ) ) ;
#45381 = CARTESIAN_POINT ( 'NONE',  ( 7.771875000614516082, 2.746126346562643317, 4.756430356249998326 ) ) ;
#45382 = CARTESIAN_POINT ( 'NONE',  ( -2.121784821874999949, 16.18437500061451573, -33.67503911421598417 ) ) ;
#45383 = CARTESIAN_POINT ( 'NONE',  ( 18.75937500061451857, -4.541064518000417216, -2.621784821875001281 ) ) ;
#45384 = CARTESIAN_POINT ( 'NONE',  ( 19.68750000122903288, 4.330127018922191873, 2.499999999999999556 ) ) ;
#45385 = CARTESIAN_POINT ( 'NONE',  ( 14.74687500061451573, -3.027376345333610441, -5.243569643749999898 ) ) ;
#45386 = CARTESIAN_POINT ( 'NONE',  ( -4.243569643749999898, 11.27187500061451608, 27.54997392385601529 ) ) ;
#45387 = CARTESIAN_POINT ( 'NONE',  ( 21.22500000122903074, -5.773502691896255534, -1.060575238724906372E-15 ) ) ;
#45388 = CARTESIAN_POINT ( 'NONE',  ( 15.62812500061451537, 6.421520780324663323E-16, -5.243569643749999010 ) ) ;
#45389 = CARTESIAN_POINT ( 'NONE',  ( 29.42812500061451431, -4.541064518000419881, 2.621784821874995952 ) ) ;
#45390 = ORIENTED_EDGE ( 'NONE', *, *, #46996, .T. ) ;
#45391 = VERTEX_POINT ( 'NONE', #55719 ) ;
#45392 = CARTESIAN_POINT ( 'NONE',  ( 21.63749999999999929, -2.886751345948125991, -5.000000000000000000 ) ) ;
#45393 = CARTESIAN_POINT ( 'NONE',  ( -3.999999999999999112, 17.86250000122903359, 30.00000000000000000 ) ) ;
#45394 = CARTESIAN_POINT ( 'NONE',  ( 3.859048791629764885, 3.180512981247726856, 28.91364485973339526 ) ) ;
#45395 = CARTESIAN_POINT ( 'NONE',  ( 15.41250000122903252, -4.330127018922190985, -2.500000000000001332 ) ) ;
#45396 = CARTESIAN_POINT ( 'NONE',  ( 19.37812500061451715, 4.541064518000418104, 2.621784821874999949 ) ) ;
#45397 = CARTESIAN_POINT ( 'NONE',  ( 22.49062500061451431, 6.054752690667223547, 3.707466751127219781E-16 ) ) ;
#45398 = CARTESIAN_POINT ( 'NONE',  ( 4.603125000614518569, 0.000000000000000000, 5.243569643749999010 ) ) ;
#45399 = EDGE_CURVE ( 'NONE', #54432, #1846, #60482, .T. ) ;
#45400 = CARTESIAN_POINT ( 'NONE',  ( 28.94999999999999929, 4.330127018922192761, -2.499999999999997780 ) ) ;
#45401 = CARTESIAN_POINT ( 'NONE',  ( 17.86875000122903501, 2.886751345948126879, 4.999999999999998224 ) ) ;
#45402 = CARTESIAN_POINT ( 'NONE',  ( 9.196875000614518569, -2.746126346562646425, 4.756430356249996549 ) ) ;
#45403 = CARTESIAN_POINT ( 'NONE',  ( 29.74687500061451217, 6.054752690667223547, 3.707466751127219781E-16 ) ) ;
#45404 = CARTESIAN_POINT ( 'NONE',  ( -3.999999999999999112, 10.66250000122903430, -30.00000000000000000 ) ) ;
#45405 = CARTESIAN_POINT ( 'NONE',  ( 9.001249775931846008E-16, 17.27187500061451786, -25.09994784771203058 ) ) ;
#45406 =( BOUNDED_CURVE ( )  B_SPLINE_CURVE ( 2, ( #61256, #23174, #5477, #5833, #10650 ),
 .UNSPECIFIED., .F., .F. ) 
 B_SPLINE_CURVE_WITH_KNOTS ( ( 3, 2, 3 ),
 ( 0.000000000000000000, 0.007246376811594202987, 0.01086956521739130578 ),
 .UNSPECIFIED. ) 
 CURVE ( )  GEOMETRIC_REPRESENTATION_ITEM ( )  RATIONAL_B_SPLINE_CURVE ( ( 1.000000000000000000, 0.8660254037844387076, 1.000000000000000000, 0.9330127018922192983, 0.9330127018922194093 ) ) 
 REPRESENTATION_ITEM ( '' )  );
#45407 = CARTESIAN_POINT ( 'NONE',  ( 6.187500001229032875, 4.330127018922191873, 2.499999999999999556 ) ) ;
#45408 = CARTESIAN_POINT ( 'NONE',  ( 8.250000000000000000, 4.330127018922192761, -2.499999999999997780 ) ) ;
#45409 = CARTESIAN_POINT ( 'NONE',  ( 3.637500001229036162, -4.330127018922194537, 2.499999999999995559 ) ) ;
#45410 = CARTESIAN_POINT ( 'NONE',  ( 11.25937500061451679, 4.541064518000418104, -2.621784821874998173 ) ) ;
#45411 = CARTESIAN_POINT ( 'NONE',  ( 19.53750000122903430, 6.123233995736764310E-16, -4.999999999999998224 ) ) ;
#45412 = CARTESIAN_POINT ( 'NONE',  ( 3.384375000614517237, -4.541064518000419881, 2.621784821874995952 ) ) ;
#45413 = CARTESIAN_POINT ( 'NONE',  ( 12.78750000122903430, 6.123233995736764310E-16, -4.999999999999998224 ) ) ;
#45414 = CARTESIAN_POINT ( 'NONE',  ( 12.73125000122903394, 6.123233995736764310E-16, -4.999999999999998224 ) ) ;
#45415 = ADVANCED_FACE ( 'NONE', ( #39457 ), #5113, .F. ) ;
#45416 = CARTESIAN_POINT ( 'NONE',  ( 9.234375000614518214, -4.541064518000419881, 2.621784821874995952 ) ) ;
#45417 = CARTESIAN_POINT ( 'NONE',  ( 13.65937500061451715, 0.000000000000000000, 5.243569643749999010 ) ) ;
#45418 = DIRECTION ( 'NONE',  ( 0.000000000000000000, -0.000000000000000000, -1.000000000000000000 ) ) ;
#45419 = CARTESIAN_POINT ( 'NONE',  ( 7.387500000000001066, 5.773502691896255534, 3.535250795749688894E-16 ) ) ;
#45420 = CARTESIAN_POINT ( 'NONE',  ( 4.243569643749999010, 16.46562500061459744, 27.54997392385601174 ) ) ;
#45421 = CARTESIAN_POINT ( 'NONE',  ( 22.05937500061451573, 4.541064518000418104, -2.621784821874998173 ) ) ;
#45422 = SURFACE_STYLE_FILL_AREA ( #17682 ) ;
#45423 =( BOUNDED_CURVE ( )  B_SPLINE_CURVE ( 2, ( #12812, #59320, #53437, #69345, #47168, #2827, #64512 ),
 .UNSPECIFIED., .F., .F. ) 
 B_SPLINE_CURVE_WITH_KNOTS ( ( 3, 2, 2, 3 ),
 ( 0.9599622389005039169, 0.9611111111111111382, 0.9638888888888889062, 0.9649218417165331685 ),
 .UNSPECIFIED. ) 
 CURVE ( )  GEOMETRIC_REPRESENTATION_ITEM ( )  RATIONAL_B_SPLINE_CURVE ( ( 0.9350132099087378190, 0.9445889114130223696, 1.000000000000000000, 0.8660254037844387076, 1.000000000000000000, 0.9501798023223894107, 0.9374121827714954058 ) ) 
 REPRESENTATION_ITEM ( '' )  );
#45424 = CARTESIAN_POINT ( 'NONE',  ( 26.21250000122903501, -4.330127018922190985, -2.500000000000001332 ) ) ;
#45425 = CARTESIAN_POINT ( 'NONE',  ( 17.14687500061451431, 0.000000000000000000, 4.756430356249998326 ) ) ;
#45426 = CARTESIAN_POINT ( 'NONE',  ( 23.31562500061451715, 3.027376345333613106, -5.243569643749998122 ) ) ;
#45427 = CARTESIAN_POINT ( 'NONE',  ( 16.52812500061451573, 6.421520780324663323E-16, -5.243569643749999010 ) ) ;
#45428 = CARTESIAN_POINT ( 'NONE',  ( 25.35937500061451644, -5.492252693125287522, -1.008910452111647106E-15 ) ) ;
#45429 = CARTESIAN_POINT ( 'NONE',  ( 11.82187500061451679, 3.027376345333611329, 5.243569643749999010 ) ) ;
#45430 = CARTESIAN_POINT ( 'NONE',  ( 27.75000000000000000, 0.000000000000000000, 4.999999999999998224 ) ) ;
#45431 = CARTESIAN_POINT ( 'NONE',  ( 25.35000000122903074, -2.886751345948125991, -5.000000000000000000 ) ) ;
#45432 = CARTESIAN_POINT ( 'NONE',  ( 3.421875000614516882, -6.054752690667223547, -1.112240025338166033E-15 ) ) ;
#45433 = AXIS2_PLACEMENT_3D ( 'NONE', #59738, #9147, #31683 ) ;
#45434 = CARTESIAN_POINT ( 'NONE',  ( 13.69687500061451679, -3.027376345333614438, 5.243569643749998122 ) ) ;
#45435 = CARTESIAN_POINT ( 'NONE',  ( 28.43437500061451573, 4.541064518000418104, 2.621784821874999949 ) ) ;
#45436 = CARTESIAN_POINT ( 'NONE',  ( 8.212500001229035007, -4.330127018922190985, -2.500000000000001332 ) ) ;
#45437 = DIRECTION ( 'NONE',  ( 0.000000000000000000, 0.000000000000000000, 1.000000000000000000 ) ) ;
#45438 = CARTESIAN_POINT ( 'NONE',  ( 23.44687500061451502, 6.054752690667223547, 3.707466751127219781E-16 ) ) ;
#45439 = CARTESIAN_POINT ( 'NONE',  ( 14.52187500061451608, 3.027376345333611329, 5.243569643749999010 ) ) ;
#45440 = CARTESIAN_POINT ( 'NONE',  ( 1.878215178124997609, 14.92812499938548321, 33.25316411605952993 ) ) ;
#45441 = CARTESIAN_POINT ( 'NONE',  ( 26.55000000000000071, -4.330127018922190985, -2.500000000000001332 ) ) ;
#45442 = CARTESIAN_POINT ( 'NONE',  ( 4.237500001229036251, 6.123233995736764310E-16, -4.999999999999998224 ) ) ;
#45443 = CARTESIAN_POINT ( 'NONE',  ( 7.359375000614517326, -5.492252693125287522, -1.008910452111647106E-15 ) ) ;
#45444 = CARTESIAN_POINT ( 'NONE',  ( 17.91562500061451502, 3.027376345333613106, -5.243569643749998122 ) ) ;
#45445 = CARTESIAN_POINT ( 'NONE',  ( 6.750000000000002665, -4.330127018922190985, -2.500000000000001332 ) ) ;
#45446 = CARTESIAN_POINT ( 'NONE',  ( 26.06250000122903288, 0.000000000000000000, 4.999999999999998224 ) ) ;
#45447 = CARTESIAN_POINT ( 'NONE',  ( 17.69999999999999929, 4.330127018922192761, -2.499999999999997780 ) ) ;
#45448 = CARTESIAN_POINT ( 'NONE',  ( -4.243569643749999898, 13.46562500061451928, 27.54997392385601529 ) ) ;
#45449 = LINE ( 'NONE', #35079, #37232 ) ;
#45450 = CARTESIAN_POINT ( 'NONE',  ( 21.18750000122903288, -4.330127018922194537, 2.499999999999995559 ) ) ;
#45451 = CARTESIAN_POINT ( 'NONE',  ( 3.975671559181609194, 9.180671356215654555, 25.48966973224918320 ) ) ;
#45452 =( BOUNDED_SURFACE ( )  B_SPLINE_SURFACE ( 1, 2, ( 
 ( #50944, #39872, #22849, #45403, #11783, #56831, #45769, #708, #28766, #23216, #17664, #62747, #34665, #51670, #26137, #48678, #71202, #20578, #64192, #9149, #25405, #64926, #65287, #43133, #42039, #64562, #8779, #59007, #13951, #36488, #37219, #69746, #42767, #54218, #14675, #70837, #25032, #47214, #19114, #8411, #25776, #8052, #14316, #47948, #20213, #59741, #13579, #41669, #36852, #19481, #36125, #31685, #42404, #30941, #3616, #59368, #31314, #53482, #37584, #53857, #30221, #65657, #70476, #2157, #19853, #3248, #15046, #52754, #48314, #60106, #24668, #58644, #30586, #2874, #53112, #2509, #47575, #70105, #49409, #67497, #16143, #9876, #54948, #32411, #20950, #66028, #43503, #61213, #26880, #56040, #66769, #27606, #72301, #60840, #4709, #10246, #10968, #37948, #32048, #21681, #60467, #38694, #9515, #55315, #67140, #49049, #15406, #50140, #22050, #44239, #32778, #27971, #54580, #73028, #5431, #4354, #10608, #5071, #33137, #27240, #71941, #72670, #61566, #3984, #44610, #55674, #16498, #33491, #39053, #66394, #50501, #21317, #26509, #22412, #71576, #49777, #44959, #43870, #15771, #38313, #16860, #39415, #51586, #6878, #6517, #63015, #28681, #46765, #68577, #62302, #34214, #11698, #258, #45319, #22767, #40499, #6152, #35304, #46041, #29411, #986, #40142, #57106, #62658, #63384, #17226, #11341, #23494, #39786, #17937, #61937, #34578, #46401, #28323, #67853, #51944, #1341, #12414, #12054, #7236, #33857, #52300, #57827, #56748, #34946, #57473, #23853, #29050, #51221, #68937, #40867, #56401, #18296, #12769, #29763, #1701, #24215, #45686, #69300, #624, #5791, #18662, #50860, #23130, #68219, #17581, #36030, #64096, #41579, #2416, #64465, #47853, #19383, #30851, #30127, #59277, #70014, #36399, #64834, #48218, #58546, #7957, #53386, #53022, #30494, #24938, #14222, #58185, #19758, #8685, #42307, #70380, #13480, #35664, #7590, #47481, #36758, #47122, #58912, #41942, #31217, #53760, #52658, #2067, #8322, #13857, #24576, #3154, #2781, #25306, #25683, #70740, #20118, #42673, #65196, #41224, #63733, #13125, #69654, #19018, #1221, #46277, #69539, #34094, #23727, #41106, #63616, #13006, #40021, #40373, #7473, #29643, #52181, #57349, #68816, #62892, #69181, #18172, #40741, #6755, #41460, #63257, #56634, #58064, #51818, #6030, #12649, #35184, #18898, #28564, #57710, #35544, #29999, #52542, #62535, #12286, #1949, #1583, #24092, #29288, #863, #63979, #7114, #34457, #6391, #56985, #45565, #17462, #68097, #46640, #51460, #24456, #18542, #47004, #51100, #34821, #496, #23006, #11932, #28923, #23370, #45918, #68450, #17812, #13361, #59159, #70991, #52904, #19261, #31468, #25927, #3027, #36637, #31837, #35902, #3768, #9303, #69895, #19997, #8937, #48099, #31095, #30732, #54011, #65441, #7838, #3407, #37002, #42550, #37374, #20367, #70261, #70622, #2662, #58427, #26293, #30375, #8567, #65077, #58793, #25179, #53264, #8203, #64713, #25558, #48467, #53634, #14468, #47364, #14833, #59524, #42918, #59898, #48830, #47722, #19632, #54373, #42189, #14097, #71360, #20735, #2302, #43293, #24817, #41815, #64346, #13737, #36279, #2902, #48707, #54247, #66423, #4381, #14346, #4013, #42433, #49077, #42794, #59770, #32076, #64954, #20242, #25433, #15801, #53885, #59398, #15074, #43899, #36880, #71230, #8808, #59036, #54976, #26910, #49436, #71970, #31345, #21344, #8438, #14705, #26537, #20609, #3277, #43167, #65686, #31712, #25805, #71604, #48343, #30974, #47975, #37611, #3644, #53509, #70503, #70868, #20979, #65315, #43532, #37249, #9177, #54608, #26167, #60133, #9542, #66053, #19880, #15431, #37976, #60497, #9903, #32440, #16170, #32805, #4737, #27271, #56069, #23161, #45715, #50168, #288, #28351, #38342, #39080, #22439, #49804, #33166, #72329, #44988, #21709, #72697, #39444, #6182, #56430, #61965, #61242, #68249, #17255, #653, #60870, #39815, #22796, #67167, #67525, #61598, #5820, #10273, #55342, #44267, #5461, #10999, #16528, #51250, #33519, #66799, #38721, #10635, #62331, #73058, #16890, #55704, #11727, #5098, #27634, #34243, #22079, #44638, #28001, #50888, #45349, #50530, #11368, #33886, #67883, #28711, #56776, #13157, #46073, #12801, #12087, #23886, #24973, #63415, #17969, #18329, #57507, #58219, #34608, #35699, #69335, #41257, #24250, #41613, #2100, #1376, #1736, #6909, #17612, #30529, #57138, #35337, #46798, #63046, #29440, #34978, #12447, #68972, #7269, #7624, #57860, #18693, #51616, #69690, #29798, #52334, #52694, #7993, #51977, #46433, #63769, #40902, #30161, #24611, #47158, #6547, #19055, #64132, #13518, #36066, #2450, #58586, #53056, #47518, #40172, #68608, #62691, #29081, #1017, #23523, #40530, #8355, #54162, #59310, #53426, #54523, #9091, #25717, #31989, #3558, #31628, #20154, #4296, #26080, #70047, #20894, #14619, #41980, #37158, #48619, #32351, #19420, #59684, #3926, #26449, #48989, #2816, #3190, #43448, #65601, #14989, #42708, #36795, #54889, #71144, #70418, #42345, #19794, #30884, #25344, #47889, #20517, #14256, #65970, #43075, #37527, #60048, #48255, #65229, #70778, #71519, #64868, #64501, #9459, #8720, #15350, #13893, #37891, #60410, #36433, #31253, #9819, #26821, #58947, #53795, #67798, #49355, #39732, #45266, #32723, #55984, #44909, #10913, #67084, #66712, #67446, #28274, #43811, #39364, #4656, #5377, #71885, #21995, #33807, #15714, #55260, #16808, #61879, #39000, #72613, #17172, #21258, #62249, #11646, #27185, #27915, #11286, #33439, #16443, #16086, #56350, #50805, #66336, #5740, #72975, #50449, #208, #22713, #33081, #22357, #38634, #38252, #34161, #60781, #44553, #56698, #21624, #61158, #10553, #44182, #27550, #61515, #6098, #10188, #49719, #72247, #55620, #5016, #50082, #63684, #18968, #40443, #62959, #7183, #57418, #12354, #34889, #35613, #68166, #41175, #52611, #13074 ),
 ( #35252, #68882, #1287, #58133, #23440, #6460, #23076, #17529, #40091, #46348, #13427, #35976, #6822, #7539, #18610, #28629, #29356, #12716, #62605, #45986, #12001, #57773, #34524, #51889, #29711, #69607, #46713, #52249, #51532, #58496, #30072, #64047, #51167, #2017, #24528, #23797, #1652, #18239, #69248, #570, #45633, #57054, #40812, #63328, #28995, #47072, #24160, #41528, #932, #68522, #17883, #31164, #15266, #37071, #7905, #31904, #25628, #52972, #48165, #20065, #43362, #30443, #70690, #14903, #37444, #59964, #13808, #14171, #54441, #3475, #25995, #53706, #47798, #65885, #14536, #8272, #53335, #30802, #19333, #64415, #41887, #59594, #25250, #3840, #65145, #48534, #42621, #59227, #3099, #8635, #9372, #36347, #2368, #9007, #58862, #31539, #24886, #54079, #65516, #47431, #2733, #71061, #20436, #42985, #26361, #48901, #69962, #71430, #20807, #70328, #37804, #19704, #42257, #64780, #36705, #5288, #39278, #54801, #50365, #10825, #66996, #11195, #44825, #44093, #44465, #49632, #60324, #124, #4207, #32996, #16358, #32634, #72159, #4570, #55174, #38545, #49996, #27833, #4930, #61432, #21171, #61790, #55535, #21909, #22273, #50721, #21538, #66620, #38913, #15996, #61069, #10466, #67360, #26735, #72892, #33721, #16723, #56266, #45180, #27465, #72521, #5657, #55897, #38167, #33360, #28192, #22629, #67711, #43724, #71802, #17083, #9734, #32268, #49269, #66247, #15625, #60691, #10104, #27100, #17445, #23709, #57333, #7097, #1566, #477, #51080, #46260, #28903, #22986, #24076, #51801, #68432, #46622, #68799, #1204, #62874, #46987, #18155, #39644, #63601, #6737, #11559, #29271, #40723, #1933, #62162, #63239, #69165, #18524, #41089, #45546, #45901, #12991, #35168, #57692, #12270, #6371, #24438, #12633, #40002, #11914, #62516, #68076, #34439, #56967, #29626, #51441, #35527, #52163, #58048, #7456, #17795, #34801, #40355, #29983, #843, #34075, #52525, #23352, #69523, #56615, #6010, #28545, #58408, #24800, #36983, #31449, #8549, #42169, #37356, #18881, #9284, #14813, #2283, #25537, #14449, #53616, #36619, #36259, #59505, #70973, #13346, #8919, #42532, #48078, #42899, #3388, #2642, #3007, #8183, #41444, #31817, #35883, #64695, #70606, #64325, #30711, #58774, #13718, #70241, #31076, #53991, #59140, #19979, #52885, #20348, #14079, #65058, #25909, #54356, #53244, #25161, #48449, #47702, #19612, #65423, #59878, #7821, #3750, #26274, #48811, #47343, #63962, #30356, #69877, #19242, #41797, #32548, #38081, #49184, #37715, #4841, #38454, #44004, #5199, #66161, #71714, #65795, #60235, #9649, #15906, #56175, #5568, #10012, #33273, #61344, #71341, #72068, #55448, #32183, #15537, #54716, #27375, #4119, #55085, #72431, #39188, #16273, #21815, #21086, #28105, #50279, #33630, #20716, #72803, #55812, #27014, #49907, #21448, #38829, #43274, #15176, #26648, #60980, #66526, #49546, #11102, #10379, #43637, #60603, #4485, #22186, #32911, #44380, #66905, #44740, #10740, #27740, #67274, #16633, #61703, #40922, #69710, #64152, #29457, #1756, #35355, #8376, #42002, #7289, #47177, #6927, #46818, #46091, #57879, #58968, #24269, #51994, #52353, #18347, #19076, #68627, #41633, #30183, #17989, #50634, #46452, #1395, #7645, #36454, #57526, #63789, #23904, #38, #47539, #70068, #19441, #64522, #68990, #13915, #23541, #29818, #13539, #13179, #63434, #35718, #41278, #69356, #12821, #36087, #18713, #40548, #63064, #58240, #52714, #12467, #34997, #2120, #24632, #58607, #8014, #30549, #53076, #2471, #24995, #42367, #14277, #64889, #9481, #48276, #4317, #15010, #49009, #20538, #9112, #26102, #31650, #32371, #59330, #53447, #43094, #8741, #60069, #30905, #3579, #15372, #70439, #36815, #71540, #43467, #65622, #54183, #49376, #2837, #21279, #26842, #31274, #37547, #26470, #32010, #48640, #70800, #20915, #9842, #25366, #65991, #54545, #3947, #54909, #37914, #14639, #60431, #20175, #47910, #43833, #19814, #71165, #71906, #3210, #42729, #65250, #25739, #66358, #15735, #38274, #60802, #53817, #37180, #59705, #5397, #44928, #45285, #589, #22017, #44573, #61900, #39019, #67103, #16461, #17192, #49740, #22732, #34180, #67819, #50824, #68185, #61534, #27934, #11664, #5760, #61178, #67464, #50467, #227, #39752, #44202, #21645, #16827, #72633, #66733, #62269, #22376, #10932, #56715, #39381, #11305, #33458, #17548, #33826, #10208, #6116, #28293, #72267, #72995, #40109, #32743, #56003, #28647, #51185, #55280, #56369, #23094, #16104, #5034, #38654, #45651, #4675, #27205, #10573, #33101, #55640, #27571, #50103, #29729, #63347, #40831, #2384, #57791, #952, #68542, #40463, #13444, #24178, #41192, #47447, #41545, #62979, #46006, #35993, #57438, #12375, #51908, #7556, #2033, #34910, #12733, #46367, #19349, #52988, #18258, #58151, #17903, #7200, #57072, #68901, #69979, #35269, #6841, #52267, #29376, #30090, #6479, #52628, #63701, #29014, #62624, #1307, #23816, #18627, #12019, #1669, #46730, #69265, #34542, #58511, #7922, #30459, #24902, #13092, #51551, #23460, #35630, #24544, #47089, #69622, #18984, #64063, #14551, #42272, #54457, #64795, #26752, #58877, #31556, #37087, #49285, #60341, #70344, #59980, #25267, #31921, #25645, #42637, #14919, #47814, #3115, #8651, #19720, #8287, #48550, #9025, #59611, #48917, #64431, #54096, #30817, #37461, #53350, #3493, #71818, #41906, #53723, #3856, #26378, #13823, #65161, #26011, #2748, #36721, #14186, #71077, #59242, #48182, #43002, #9750, #9390, #65533, #31180, #36363, #20823, #4224, #70706, #43378, #71448, #65902, #15282, #20452, #37822, #32284, #20081, #54818, #10484, #21190, #34092, #38184, #67014, #27851, #66637, #33013, #38563, #16015, #72539, #10843, #39294, #38930, #22289, #55192, #140, #16375, #55913, #56284, #11577, #55552, #4948, #72907, #50015, #27482, #21927, #28209, #60708, #33738 ) ),
 .UNSPECIFIED., .F., .F., .F. ) 
 B_SPLINE_SURFACE_WITH_KNOTS ( ( 2, 2 ),
 ( 3, 2, 2, 2, 2, 2, 2, 2, 2, 2, 2, 2, 2, 2, 2, 2, 2, 2, 2, 2, 2, 2, 2, 2, 2, 2, 2, 2, 2, 2, 2, 2, 2, 2, 2, 2, 2, 2, 2, 2, 2, 2, 2, 2, 2, 2, 2, 2, 2, 2, 2, 2, 2, 2, 2, 2, 2, 2, 2, 2, 2, 2, 2, 2, 2, 2, 2, 2, 2, 2, 2, 2, 2, 2, 2, 2, 2, 2, 2, 2, 2, 2, 2, 2, 2, 2, 2, 2, 2, 2, 2, 2, 2, 2, 2, 2, 2, 2, 2, 2, 2, 2, 2, 2, 2, 2, 2, 2, 2, 2, 2, 2, 2, 2, 2, 2, 2, 2, 2, 2, 2, 2, 2, 2, 2, 2, 2, 2, 2, 2, 2, 2, 2, 2, 2, 2, 2, 2, 2, 2, 2, 2, 2, 2, 2, 2, 2, 2, 2, 2, 2, 2, 2, 2, 2, 2, 2, 2, 2, 2, 2, 2, 2, 2, 2, 2, 2, 2, 2, 2, 2, 2, 2, 2, 2, 2, 2, 2, 2, 2, 2, 2, 2, 2, 2, 2, 2, 2, 2, 2, 2, 2, 2, 2, 2, 2, 2, 2, 2, 2, 2, 2, 2, 2, 2, 2, 2, 2, 2, 2, 2, 2, 2, 2, 2, 2, 2, 2, 2, 2, 2, 2, 2, 2, 2, 2, 2, 2, 2, 2, 2, 2, 2, 2, 2, 2, 2, 2, 2, 2, 2, 2, 2, 2, 2, 2, 2, 2, 2, 2, 2, 2, 2, 2, 2, 2, 2, 2, 2, 2, 2, 2, 2, 2, 2, 2, 2, 2, 2, 2, 2, 2, 2, 2, 2, 2, 2, 2, 2, 2, 2, 2, 2, 2, 2, 2, 2, 2, 2, 2, 2, 2, 2, 2, 2, 2, 2, 2, 2, 2, 2, 2, 2, 2, 2, 2, 2, 2, 2, 2, 2, 2, 2, 2, 2, 2, 2, 2, 2, 2, 2, 2, 2, 2, 2, 2, 2, 2, 2, 2, 2, 2, 2, 2, 2, 2, 2, 2, 2, 2, 2, 2, 2, 2, 2, 2, 2, 2, 2, 2, 2, 2, 2, 2, 2, 2, 2, 2, 2, 2, 3 ),
 ( 0.000000000000000000, 1.000000000000000000 ),
 ( 0.000000000000000000, 0.002777777777777777884, 0.005555555555555555768, 0.008333333333333333218, 0.01111111111111111154, 0.01388888888888888812, 0.01666666666666666644, 0.01944444444444444475, 0.02222222222222222307, 0.02500000000000000139, 0.02777777777777777624, 0.03055555555555555455, 0.03333333333333333287, 0.03611111111111110772, 0.03888888888888888951, 0.04166666666666666435, 0.04444444444444444614, 0.04722222222222222099, 0.05000000000000000278, 0.05277777777777777762, 0.05555555555555555247, 0.05833333333333333426, 0.06111111111111110911, 0.06388888888888888395, 0.06666666666666666574, 0.06944444444444444753, 0.07222222222222221544, 0.07499999999999999722, 0.07777777777777777901, 0.08055555555555556080, 0.08333333333333332871, 0.08611111111111111049, 0.08888888888888889228, 0.09166666666666666019, 0.09444444444444444198, 0.09722222222222222376, 0.1000000000000000056, 0.1027777777777777735, 0.1055555555555555552, 0.1083333333333333370, 0.1111111111111111049, 0.1138888888888888867, 0.1166666666666666685, 0.1194444444444444503, 0.1222222222222222182, 0.1250000000000000000, 0.1277777777777777679, 0.1305555555555555636, 0.1333333333333333315, 0.1361111111111110994, 0.1388888888888888951, 0.1416666666666666630, 0.1444444444444444309, 0.1472222222222222265, 0.1499999999999999944, 0.1527777777777777901, 0.1555555555555555580, 0.1583333333333333259, 0.1611111111111111216, 0.1638888888888888895, 0.1666666666666666574, 0.1694444444444444531, 0.1722222222222222210, 0.1749999999999999889, 0.1777777777777777846, 0.1805555555555555525, 0.1833333333333333204, 0.1861111111111111160, 0.1888888888888888840, 0.1916666666666666796, 0.1944444444444444475, 0.1972222222222222154, 0.2000000000000000111, 0.2027777777777777790, 0.2055555555555555469, 0.2083333333333333426, 0.2111111111111111105, 0.2138888888888888784, 0.2166666666666666741, 0.2194444444444444420, 0.2222222222222222099, 0.2250000000000000056, 0.2277777777777777735, 0.2305555555555555691, 0.2333333333333333370, 0.2361111111111111049, 0.2388888888888889006, 0.2416666666666666685, 0.2444444444444444364, 0.2472222222222222321, 0.2500000000000000000, 0.2527777777777777679, 0.2555555555555555358, 0.2583333333333333592, 0.2611111111111111271, 0.2638888888888888951, 0.2666666666666666630, 0.2694444444444444309, 0.2722222222222221988, 0.2750000000000000222, 0.2777777777777777901, 0.2805555555555555580, 0.2833333333333333259, 0.2861111111111110938, 0.2888888888888888618, 0.2916666666666666852, 0.2944444444444444531, 0.2972222222222222210, 0.2999999999999999889, 0.3027777777777777568, 0.3055555555555555802, 0.3083333333333333481, 0.3111111111111111160, 0.3138888888888888840, 0.3166666666666666519, 0.3194444444444444198, 0.3222222222222222432, 0.3250000000000000111, 0.3277777777777777790, 0.3305555555555555469, 0.3333333333333333148, 0.3361111111111111382, 0.3388888888888889062, 0.3416666666666666741, 0.3444444444444444420, 0.3472222222222222099, 0.3499999999999999778, 0.3527777777777778012, 0.3555555555555555691, 0.3583333333333333370, 0.3611111111111111049, 0.3638888888888888729, 0.3666666666666666408, 0.3694444444444444642, 0.3722222222222222321, 0.3750000000000000000, 0.3777777777777777679, 0.3805555555555555358, 0.3833333333333333592, 0.3861111111111111271, 0.3888888888888888951, 0.3916666666666666630, 0.3944444444444444309, 0.3972222222222221988, 0.4000000000000000222, 0.4027777777777777901, 0.4055555555555555580, 0.4083333333333333259, 0.4111111111111110938, 0.4138888888888888618, 0.4166666666666666852, 0.4194444444444444531, 0.4222222222222222210, 0.4249999999999999889, 0.4277777777777777568, 0.4305555555555555802, 0.4333333333333333481, 0.4361111111111111160, 0.4388888888888888840, 0.4416666666666666519, 0.4444444444444444198, 0.4472222222222222432, 0.4500000000000000111, 0.4527777777777777790, 0.4555555555555555469, 0.4583333333333333148, 0.4611111111111111382, 0.4638888888888889062, 0.4666666666666666741, 0.4694444444444444420, 0.4722222222222222099, 0.4749999999999999778, 0.4777777777777778012, 0.4805555555555555691, 0.4833333333333333370, 0.4861111111111111049, 0.4888888888888888729, 0.4916666666666666408, 0.4944444444444444642, 0.4972222222222222321, 0.5000000000000000000, 0.5027777777777777679, 0.5055555555555555358, 0.5083333333333333037, 0.5111111111111110716, 0.5138888888888888395, 0.5166666666666667185, 0.5194444444444444864, 0.5222222222222222543, 0.5250000000000000222, 0.5277777777777777901, 0.5305555555555555580, 0.5333333333333333259, 0.5361111111111110938, 0.5388888888888888618, 0.5416666666666666297, 0.5444444444444443976, 0.5472222222222222765, 0.5500000000000000444, 0.5527777777777778123, 0.5555555555555555802, 0.5583333333333333481, 0.5611111111111111160, 0.5638888888888888840, 0.5666666666666666519, 0.5694444444444444198, 0.5722222222222221877, 0.5749999999999999556, 0.5777777777777777235, 0.5805555555555556024, 0.5833333333333333703, 0.5861111111111111382, 0.5888888888888889062, 0.5916666666666666741, 0.5944444444444444420, 0.5972222222222222099, 0.5999999999999999778, 0.6027777777777777457, 0.6055555555555555136, 0.6083333333333332815, 0.6111111111111111605, 0.6138888888888889284, 0.6166666666666666963, 0.6194444444444444642, 0.6222222222222222321, 0.6250000000000000000, 0.6277777777777777679, 0.6305555555555555358, 0.6333333333333333037, 0.6361111111111110716, 0.6388888888888888395, 0.6416666666666667185, 0.6444444444444444864, 0.6472222222222222543, 0.6500000000000000222, 0.6527777777777777901, 0.6555555555555555580, 0.6583333333333333259, 0.6611111111111110938, 0.6638888888888888618, 0.6666666666666666297, 0.6694444444444443976, 0.6722222222222222765, 0.6750000000000000444, 0.6777777777777778123, 0.6805555555555555802, 0.6833333333333333481, 0.6861111111111111160, 0.6888888888888888840, 0.6916666666666666519, 0.6944444444444444198, 0.6972222222222221877, 0.6999999999999999556, 0.7027777777777777235, 0.7055555555555556024, 0.7083333333333333703, 0.7111111111111111382, 0.7138888888888889062, 0.7166666666666666741, 0.7194444444444444420, 0.7222222222222222099, 0.7249999999999999778, 0.7277777777777777457, 0.7305555555555555136, 0.7333333333333332815, 0.7361111111111111605, 0.7388888888888889284, 0.7416666666666666963, 0.7444444444444444642, 0.7472222222222222321, 0.7500000000000000000, 0.7527777777777777679, 0.7555555555555555358, 0.7583333333333333037, 0.7611111111111110716, 0.7638888888888888395, 0.7666666666666667185, 0.7694444444444444864, 0.7722222222222222543, 0.7750000000000000222, 0.7777777777777777901, 0.7805555555555555580, 0.7833333333333333259, 0.7861111111111110938, 0.7888888888888888618, 0.7916666666666666297, 0.7944444444444443976, 0.7972222222222222765, 0.8000000000000000444, 0.8027777777777778123, 0.8055555555555555802, 0.8083333333333333481, 0.8111111111111111160, 0.8138888888888888840, 0.8166666666666666519, 0.8194444444444444198, 0.8222222222222221877, 0.8249999999999999556, 0.8277777777777777235, 0.8305555555555556024, 0.8333333333333333703, 0.8361111111111111382, 0.8388888888888889062, 0.8416666666666666741, 0.8444444444444444420, 0.8472222222222222099, 0.8499999999999999778, 0.8527777777777777457, 0.8555555555555555136, 0.8583333333333332815, 0.8611111111111111605, 0.8638888888888889284, 0.8666666666666666963, 0.8694444444444444642, 0.8722222222222222321, 0.8750000000000000000, 0.8777777777777777679, 0.8805555555555555358, 0.8833333333333333037, 0.8861111111111110716, 0.8888888888888888395, 0.8916666666666667185, 0.8944444444444444864, 0.8972222222222222543, 0.9000000000000000222, 0.9027777777777777901, 0.9055555555555555580, 0.9083333333333333259, 0.9111111111111110938, 0.9138888888888888618, 0.9166666666666666297, 0.9194444444444443976, 0.9222222222222222765, 0.9250000000000000444, 0.9277777777777778123, 0.9305555555555555802, 0.9333333333333333481, 0.9361111111111111160, 0.9388888888888888840, 0.9416666666666666519, 0.9444444444444444198, 0.9472222222222221877, 0.9499999999999999556, 0.9527777777777777235, 0.9555555555555556024, 0.9583333333333333703, 0.9611111111111111382, 0.9638888888888889062, 0.9666666666666666741, 0.9694444444444444420, 0.9722222222222222099, 0.9749999999999999778, 0.9777777777777777457, 0.9805555555555555136, 0.9833333333333332815, 0.9861111111111111605, 0.9888888888888889284, 0.9916666666666666963, 0.9944444444444444642, 0.9972222222222222321, 1.000000000000000000 ),
 .UNSPECIFIED. ) 
 GEOMETRIC_REPRESENTATION_ITEM ( )  RATIONAL_B_SPLINE_SURFACE ( (
 ( 1.000000000000000000, 0.8660254037844387076, 1.000000000000000000, 0.8660254037844387076, 1.000000000000000000, 0.8660254037844387076, 1.000000000000000000, 0.8660254037844387076, 1.000000000000000000, 0.8660254037844387076, 1.000000000000000000, 0.8660254037844387076, 1.000000000000000000, 0.8660254037844387076, 1.000000000000000000, 0.8660254037844387076, 1.000000000000000000, 0.8660254037844387076, 1.000000000000000000, 0.8660254037844387076, 1.000000000000000000, 0.8660254037844387076, 1.000000000000000000, 0.8660254037844387076, 1.000000000000000000, 0.8660254037844387076, 1.000000000000000000, 0.8660254037844387076, 1.000000000000000000, 0.8660254037844387076, 1.000000000000000000, 0.8660254037844387076, 1.000000000000000000, 0.8660254037844387076, 1.000000000000000000, 0.8660254037844387076, 1.000000000000000000, 0.8660254037844387076, 1.000000000000000000, 0.8660254037844387076, 1.000000000000000000, 0.8660254037844387076, 1.000000000000000000, 0.8660254037844387076, 1.000000000000000000, 0.8660254037844387076, 1.000000000000000000, 0.8660254037844387076, 1.000000000000000000, 0.8660254037844387076, 1.000000000000000000, 0.8660254037844387076, 1.000000000000000000, 0.8660254037844387076, 1.000000000000000000, 0.8660254037844387076, 1.000000000000000000, 0.8660254037844387076, 1.000000000000000000, 0.8660254037844387076, 1.000000000000000000, 0.8660254037844387076, 1.000000000000000000, 0.8660254037844387076, 1.000000000000000000, 0.8660254037844387076, 1.000000000000000000, 0.8660254037844387076, 1.000000000000000000, 0.8660254037844387076, 1.000000000000000000, 0.8660254037844387076, 1.000000000000000000, 0.8660254037844387076, 1.000000000000000000, 0.8660254037844387076, 1.000000000000000000, 0.8660254037844387076, 1.000000000000000000, 0.8660254037844387076, 1.000000000000000000, 0.8660254037844387076, 1.000000000000000000, 0.8660254037844387076, 1.000000000000000000, 0.8660254037844387076, 1.000000000000000000, 0.8660254037844387076, 1.000000000000000000, 0.8660254037844387076, 1.000000000000000000, 0.8660254037844387076, 1.000000000000000000, 0.8660254037844387076, 1.000000000000000000, 0.8660254037844387076, 1.000000000000000000, 0.8660254037844387076, 1.000000000000000000, 0.8660254037844387076, 1.000000000000000000, 0.8660254037844387076, 1.000000000000000000, 0.8660254037844387076, 1.000000000000000000, 0.8660254037844387076, 1.000000000000000000, 0.8660254037844387076, 1.000000000000000000, 0.8660254037844387076, 1.000000000000000000, 0.8660254037844387076, 1.000000000000000000, 0.8660254037844387076, 1.000000000000000000, 0.8660254037844387076, 1.000000000000000000, 0.8660254037844387076, 1.000000000000000000, 0.8660254037844387076, 1.000000000000000000, 0.8660254037844387076, 1.000000000000000000, 0.8660254037844387076, 1.000000000000000000, 0.8660254037844387076, 1.000000000000000000, 0.8660254037844387076, 1.000000000000000000, 0.8660254037844387076, 1.000000000000000000, 0.8660254037844387076, 1.000000000000000000, 0.8660254037844387076, 1.000000000000000000, 0.8660254037844387076, 1.000000000000000000, 0.8660254037844387076, 1.000000000000000000, 0.8660254037844387076, 1.000000000000000000, 0.8660254037844387076, 1.000000000000000000, 0.8660254037844387076, 1.000000000000000000, 0.8660254037844387076, 1.000000000000000000, 0.8660254037844387076, 1.000000000000000000, 0.8660254037844387076, 1.000000000000000000, 0.8660254037844387076, 1.000000000000000000, 0.8660254037844387076, 1.000000000000000000, 0.8660254037844387076, 1.000000000000000000, 0.8660254037844387076, 1.000000000000000000, 0.8660254037844387076, 1.000000000000000000, 0.8660254037844387076, 1.000000000000000000, 0.8660254037844387076, 1.000000000000000000, 0.8660254037844387076, 1.000000000000000000, 0.8660254037844387076, 1.000000000000000000, 0.8660254037844387076, 1.000000000000000000, 0.8660254037844387076, 1.000000000000000000, 0.8660254037844387076, 1.000000000000000000, 0.8660254037844387076, 1.000000000000000000, 0.8660254037844387076, 1.000000000000000000, 0.8660254037844387076, 1.000000000000000000, 0.8660254037844387076, 1.000000000000000000, 0.8660254037844387076, 1.000000000000000000, 0.8660254037844387076, 1.000000000000000000, 0.8660254037844387076, 1.000000000000000000, 0.8660254037844387076, 1.000000000000000000, 0.8660254037844387076, 1.000000000000000000, 0.8660254037844387076, 1.000000000000000000, 0.8660254037844387076, 1.000000000000000000, 0.8660254037844387076, 1.000000000000000000, 0.8660254037844387076, 1.000000000000000000, 0.8660254037844387076, 1.000000000000000000, 0.8660254037844387076, 1.000000000000000000, 0.8660254037844387076, 1.000000000000000000, 0.8660254037844387076, 1.000000000000000000, 0.8660254037844387076, 1.000000000000000000, 0.8660254037844387076, 1.000000000000000000, 0.8660254037844387076, 1.000000000000000000, 0.8660254037844387076, 1.000000000000000000, 0.8660254037844387076, 1.000000000000000000, 0.8660254037844387076, 1.000000000000000000, 0.8660254037844387076, 1.000000000000000000, 0.8660254037844387076, 1.000000000000000000, 0.8660254037844387076, 1.000000000000000000, 0.8660254037844387076, 1.000000000000000000, 0.8660254037844387076, 1.000000000000000000, 0.8660254037844387076, 1.000000000000000000, 0.8660254037844387076, 1.000000000000000000, 0.8660254037844387076, 1.000000000000000000, 0.8660254037844387076, 1.000000000000000000, 0.8660254037844387076, 1.000000000000000000, 0.8660254037844387076, 1.000000000000000000, 0.8660254037844387076, 1.000000000000000000, 0.8660254037844387076, 1.000000000000000000, 0.8660254037844387076, 1.000000000000000000, 0.8660254037844387076, 1.000000000000000000, 0.8660254037844387076, 1.000000000000000000, 0.8660254037844387076, 1.000000000000000000, 0.8660254037844387076, 1.000000000000000000, 0.8660254037844387076, 1.000000000000000000, 0.8660254037844387076, 1.000000000000000000, 0.8660254037844387076, 1.000000000000000000, 0.8660254037844387076, 1.000000000000000000, 0.8660254037844387076, 1.000000000000000000, 0.8660254037844387076, 1.000000000000000000, 0.8660254037844387076, 1.000000000000000000, 0.8660254037844387076, 1.000000000000000000, 0.8660254037844387076, 1.000000000000000000, 0.8660254037844387076, 1.000000000000000000, 0.8660254037844387076, 1.000000000000000000, 0.8660254037844387076, 1.000000000000000000, 0.8660254037844387076, 1.000000000000000000, 0.8660254037844387076, 1.000000000000000000, 0.8660254037844387076, 1.000000000000000000, 0.8660254037844387076, 1.000000000000000000, 0.8660254037844387076, 1.000000000000000000, 0.8660254037844387076, 1.000000000000000000, 0.8660254037844387076, 1.000000000000000000, 0.8660254037844387076, 1.000000000000000000, 0.8660254037844387076, 1.000000000000000000, 0.8660254037844387076, 1.000000000000000000, 0.8660254037844387076, 1.000000000000000000, 0.8660254037844387076, 1.000000000000000000, 0.8660254037844387076, 1.000000000000000000, 0.8660254037844387076, 1.000000000000000000, 0.8660254037844387076, 1.000000000000000000, 0.8660254037844387076, 1.000000000000000000, 0.8660254037844387076, 1.000000000000000000, 0.8660254037844387076, 1.000000000000000000, 0.8660254037844387076, 1.000000000000000000, 0.8660254037844387076, 1.000000000000000000, 0.8660254037844387076, 1.000000000000000000, 0.8660254037844387076, 1.000000000000000000, 0.8660254037844387076, 1.000000000000000000, 0.8660254037844387076, 1.000000000000000000, 0.8660254037844387076, 1.000000000000000000, 0.8660254037844387076, 1.000000000000000000, 0.8660254037844387076, 1.000000000000000000, 0.8660254037844387076, 1.000000000000000000, 0.8660254037844387076, 1.000000000000000000, 0.8660254037844387076, 1.000000000000000000, 0.8660254037844387076, 1.000000000000000000, 0.8660254037844387076, 1.000000000000000000, 0.8660254037844387076, 1.000000000000000000, 0.8660254037844387076, 1.000000000000000000, 0.8660254037844387076, 1.000000000000000000, 0.8660254037844387076, 1.000000000000000000, 0.8660254037844387076, 1.000000000000000000, 0.8660254037844387076, 1.000000000000000000, 0.8660254037844387076, 1.000000000000000000, 0.8660254037844387076, 1.000000000000000000, 0.8660254037844387076, 1.000000000000000000, 0.8660254037844387076, 1.000000000000000000, 0.8660254037844387076, 1.000000000000000000, 0.8660254037844387076, 1.000000000000000000, 0.8660254037844387076, 1.000000000000000000, 0.8660254037844387076, 1.000000000000000000, 0.8660254037844387076, 1.000000000000000000, 0.8660254037844387076, 1.000000000000000000, 0.8660254037844387076, 1.000000000000000000, 0.8660254037844387076, 1.000000000000000000, 0.8660254037844387076, 1.000000000000000000, 0.8660254037844387076, 1.000000000000000000, 0.8660254037844387076, 1.000000000000000000, 0.8660254037844387076, 1.000000000000000000, 0.8660254037844387076, 1.000000000000000000, 0.8660254037844387076, 1.000000000000000000, 0.8660254037844387076, 1.000000000000000000, 0.8660254037844387076, 1.000000000000000000, 0.8660254037844387076, 1.000000000000000000, 0.8660254037844387076, 1.000000000000000000, 0.8660254037844387076, 1.000000000000000000, 0.8660254037844387076, 1.000000000000000000, 0.8660254037844387076, 1.000000000000000000, 0.8660254037844387076, 1.000000000000000000, 0.8660254037844387076, 1.000000000000000000, 0.8660254037844387076, 1.000000000000000000, 0.8660254037844387076, 1.000000000000000000, 0.8660254037844387076, 1.000000000000000000, 0.8660254037844387076, 1.000000000000000000, 0.8660254037844387076, 1.000000000000000000, 0.8660254037844387076, 1.000000000000000000, 0.8660254037844387076, 1.000000000000000000, 0.8660254037844387076, 1.000000000000000000, 0.8660254037844387076, 1.000000000000000000, 0.8660254037844387076, 1.000000000000000000, 0.8660254037844387076, 1.000000000000000000, 0.8660254037844387076, 1.000000000000000000, 0.8660254037844387076, 1.000000000000000000, 0.8660254037844387076, 1.000000000000000000, 0.8660254037844387076, 1.000000000000000000, 0.8660254037844387076, 1.000000000000000000, 0.8660254037844387076, 1.000000000000000000, 0.8660254037844387076, 1.000000000000000000, 0.8660254037844387076, 1.000000000000000000, 0.8660254037844387076, 1.000000000000000000, 0.8660254037844387076, 1.000000000000000000, 0.8660254037844387076, 1.000000000000000000, 0.8660254037844387076, 1.000000000000000000, 0.8660254037844387076, 1.000000000000000000, 0.8660254037844387076, 1.000000000000000000, 0.8660254037844387076, 1.000000000000000000, 0.8660254037844387076, 1.000000000000000000, 0.8660254037844387076, 1.000000000000000000, 0.8660254037844387076, 1.000000000000000000, 0.8660254037844387076, 1.000000000000000000, 0.8660254037844387076, 1.000000000000000000, 0.8660254037844387076, 1.000000000000000000, 0.8660254037844387076, 1.000000000000000000, 0.8660254037844387076, 1.000000000000000000, 0.8660254037844387076, 1.000000000000000000, 0.8660254037844387076, 1.000000000000000000, 0.8660254037844387076, 1.000000000000000000, 0.8660254037844387076, 1.000000000000000000, 0.8660254037844387076, 1.000000000000000000, 0.8660254037844387076, 1.000000000000000000, 0.8660254037844387076, 1.000000000000000000, 0.8660254037844387076, 1.000000000000000000, 0.8660254037844387076, 1.000000000000000000, 0.8660254037844387076, 1.000000000000000000, 0.8660254037844387076, 1.000000000000000000, 0.8660254037844387076, 1.000000000000000000, 0.8660254037844387076, 1.000000000000000000, 0.8660254037844387076, 1.000000000000000000, 0.8660254037844387076, 1.000000000000000000, 0.8660254037844387076, 1.000000000000000000, 0.8660254037844387076, 1.000000000000000000, 0.8660254037844387076, 1.000000000000000000, 0.8660254037844387076, 1.000000000000000000, 0.8660254037844387076, 1.000000000000000000, 0.8660254037844387076, 1.000000000000000000, 0.8660254037844387076, 1.000000000000000000, 0.8660254037844387076, 1.000000000000000000, 0.8660254037844387076, 1.000000000000000000, 0.8660254037844387076, 1.000000000000000000, 0.8660254037844387076, 1.000000000000000000, 0.8660254037844387076, 1.000000000000000000, 0.8660254037844387076, 1.000000000000000000, 0.8660254037844387076, 1.000000000000000000, 0.8660254037844387076, 1.000000000000000000, 0.8660254037844387076, 1.000000000000000000, 0.8660254037844387076, 1.000000000000000000, 0.8660254037844387076, 1.000000000000000000, 0.8660254037844387076, 1.000000000000000000, 0.8660254037844387076, 1.000000000000000000, 0.8660254037844387076, 1.000000000000000000, 0.8660254037844387076, 1.000000000000000000, 0.8660254037844387076, 1.000000000000000000, 0.8660254037844387076, 1.000000000000000000, 0.8660254037844387076, 1.000000000000000000, 0.8660254037844387076, 1.000000000000000000, 0.8660254037844387076, 1.000000000000000000, 0.8660254037844387076, 1.000000000000000000, 0.8660254037844387076, 1.000000000000000000, 0.8660254037844387076, 1.000000000000000000, 0.8660254037844387076, 1.000000000000000000, 0.8660254037844387076, 1.000000000000000000, 0.8660254037844387076, 1.000000000000000000, 0.8660254037844387076, 1.000000000000000000, 0.8660254037844387076, 1.000000000000000000, 0.8660254037844387076, 1.000000000000000000, 0.8660254037844387076, 1.000000000000000000, 0.8660254037844387076, 1.000000000000000000, 0.8660254037844387076, 1.000000000000000000, 0.8660254037844387076, 1.000000000000000000, 0.8660254037844387076, 1.000000000000000000, 0.8660254037844387076, 1.000000000000000000, 0.8660254037844387076, 1.000000000000000000, 0.8660254037844387076, 1.000000000000000000, 0.8660254037844387076, 1.000000000000000000, 0.8660254037844387076, 1.000000000000000000, 0.8660254037844387076, 1.000000000000000000, 0.8660254037844387076, 1.000000000000000000, 0.8660254037844387076, 1.000000000000000000, 0.8660254037844387076, 1.000000000000000000, 0.8660254037844387076, 1.000000000000000000, 0.8660254037844387076, 1.000000000000000000, 0.8660254037844387076, 1.000000000000000000, 0.8660254037844387076, 1.000000000000000000, 0.8660254037844387076, 1.000000000000000000, 0.8660254037844387076, 1.000000000000000000, 0.8660254037844387076, 1.000000000000000000, 0.8660254037844387076, 1.000000000000000000, 0.8660254037844387076, 1.000000000000000000, 0.8660254037844387076, 1.000000000000000000, 0.8660254037844387076, 1.000000000000000000, 0.8660254037844387076, 1.000000000000000000, 0.8660254037844387076, 1.000000000000000000, 0.8660254037844387076, 1.000000000000000000, 0.8660254037844387076, 1.000000000000000000, 0.8660254037844387076, 1.000000000000000000, 0.8660254037844387076, 1.000000000000000000, 0.8660254037844387076, 1.000000000000000000, 0.8660254037844387076, 1.000000000000000000, 0.8660254037844387076, 1.000000000000000000, 0.8660254037844387076, 1.000000000000000000, 0.8660254037844387076, 1.000000000000000000, 0.8660254037844387076, 1.000000000000000000, 0.8660254037844387076, 1.000000000000000000, 0.8660254037844387076, 1.000000000000000000, 0.8660254037844387076, 1.000000000000000000, 0.8660254037844387076, 1.000000000000000000, 0.8660254037844387076, 1.000000000000000000, 0.8660254037844387076, 1.000000000000000000, 0.8660254037844387076, 1.000000000000000000, 0.8660254037844387076, 1.000000000000000000, 0.8660254037844387076, 1.000000000000000000, 0.8660254037844387076, 1.000000000000000000, 0.8660254037844387076, 1.000000000000000000, 0.8660254037844387076, 1.000000000000000000, 0.8660254037844387076, 1.000000000000000000, 0.8660254037844387076, 1.000000000000000000, 0.8660254037844387076, 1.000000000000000000, 0.8660254037844387076, 1.000000000000000000, 0.8660254037844387076, 1.000000000000000000, 0.8660254037844387076, 1.000000000000000000, 0.8660254037844387076, 1.000000000000000000, 0.8660254037844387076, 1.000000000000000000, 0.8660254037844387076, 1.000000000000000000, 0.8660254037844387076, 1.000000000000000000, 0.8660254037844387076, 1.000000000000000000, 0.8660254037844387076, 1.000000000000000000, 0.8660254037844387076, 1.000000000000000000, 0.8660254037844387076, 1.000000000000000000, 0.8660254037844387076, 1.000000000000000000, 0.8660254037844387076, 1.000000000000000000, 0.8660254037844387076, 1.000000000000000000, 0.8660254037844387076, 1.000000000000000000, 0.8660254037844387076, 1.000000000000000000, 0.8660254037844387076, 1.000000000000000000, 0.8660254037844387076, 1.000000000000000000),
 ( 1.000000000000000000, 0.8660254037844387076, 1.000000000000000000, 0.8660254037844387076, 1.000000000000000000, 0.8660254037844387076, 1.000000000000000000, 0.8660254037844387076, 1.000000000000000000, 0.8660254037844387076, 1.000000000000000000, 0.8660254037844387076, 1.000000000000000000, 0.8660254037844387076, 1.000000000000000000, 0.8660254037844387076, 1.000000000000000000, 0.8660254037844387076, 1.000000000000000000, 0.8660254037844387076, 1.000000000000000000, 0.8660254037844387076, 1.000000000000000000, 0.8660254037844387076, 1.000000000000000000, 0.8660254037844387076, 1.000000000000000000, 0.8660254037844387076, 1.000000000000000000, 0.8660254037844387076, 1.000000000000000000, 0.8660254037844387076, 1.000000000000000000, 0.8660254037844387076, 1.000000000000000000, 0.8660254037844387076, 1.000000000000000000, 0.8660254037844387076, 1.000000000000000000, 0.8660254037844387076, 1.000000000000000000, 0.8660254037844387076, 1.000000000000000000, 0.8660254037844387076, 1.000000000000000000, 0.8660254037844387076, 1.000000000000000000, 0.8660254037844387076, 1.000000000000000000, 0.8660254037844387076, 1.000000000000000000, 0.8660254037844387076, 1.000000000000000000, 0.8660254037844387076, 1.000000000000000000, 0.8660254037844387076, 1.000000000000000000, 0.8660254037844387076, 1.000000000000000000, 0.8660254037844387076, 1.000000000000000000, 0.8660254037844387076, 1.000000000000000000, 0.8660254037844387076, 1.000000000000000000, 0.8660254037844387076, 1.000000000000000000, 0.8660254037844387076, 1.000000000000000000, 0.8660254037844387076, 1.000000000000000000, 0.8660254037844387076, 1.000000000000000000, 0.8660254037844387076, 1.000000000000000000, 0.8660254037844387076, 1.000000000000000000, 0.8660254037844387076, 1.000000000000000000, 0.8660254037844387076, 1.000000000000000000, 0.8660254037844387076, 1.000000000000000000, 0.8660254037844387076, 1.000000000000000000, 0.8660254037844387076, 1.000000000000000000, 0.8660254037844387076, 1.000000000000000000, 0.8660254037844387076, 1.000000000000000000, 0.8660254037844387076, 1.000000000000000000, 0.8660254037844387076, 1.000000000000000000, 0.8660254037844387076, 1.000000000000000000, 0.8660254037844387076, 1.000000000000000000, 0.8660254037844387076, 1.000000000000000000, 0.8660254037844387076, 1.000000000000000000, 0.8660254037844387076, 1.000000000000000000, 0.8660254037844387076, 1.000000000000000000, 0.8660254037844387076, 1.000000000000000000, 0.8660254037844387076, 1.000000000000000000, 0.8660254037844387076, 1.000000000000000000, 0.8660254037844387076, 1.000000000000000000, 0.8660254037844387076, 1.000000000000000000, 0.8660254037844387076, 1.000000000000000000, 0.8660254037844387076, 1.000000000000000000, 0.8660254037844387076, 1.000000000000000000, 0.8660254037844387076, 1.000000000000000000, 0.8660254037844387076, 1.000000000000000000, 0.8660254037844387076, 1.000000000000000000, 0.8660254037844387076, 1.000000000000000000, 0.8660254037844387076, 1.000000000000000000, 0.8660254037844387076, 1.000000000000000000, 0.8660254037844387076, 1.000000000000000000, 0.8660254037844387076, 1.000000000000000000, 0.8660254037844387076, 1.000000000000000000, 0.8660254037844387076, 1.000000000000000000, 0.8660254037844387076, 1.000000000000000000, 0.8660254037844387076, 1.000000000000000000, 0.8660254037844387076, 1.000000000000000000, 0.8660254037844387076, 1.000000000000000000, 0.8660254037844387076, 1.000000000000000000, 0.8660254037844387076, 1.000000000000000000, 0.8660254037844387076, 1.000000000000000000, 0.8660254037844387076, 1.000000000000000000, 0.8660254037844387076, 1.000000000000000000, 0.8660254037844387076, 1.000000000000000000, 0.8660254037844387076, 1.000000000000000000, 0.8660254037844387076, 1.000000000000000000, 0.8660254037844387076, 1.000000000000000000, 0.8660254037844387076, 1.000000000000000000, 0.8660254037844387076, 1.000000000000000000, 0.8660254037844387076, 1.000000000000000000, 0.8660254037844387076, 1.000000000000000000, 0.8660254037844387076, 1.000000000000000000, 0.8660254037844387076, 1.000000000000000000, 0.8660254037844387076, 1.000000000000000000, 0.8660254037844387076, 1.000000000000000000, 0.8660254037844387076, 1.000000000000000000, 0.8660254037844387076, 1.000000000000000000, 0.8660254037844387076, 1.000000000000000000, 0.8660254037844387076, 1.000000000000000000, 0.8660254037844387076, 1.000000000000000000, 0.8660254037844387076, 1.000000000000000000, 0.8660254037844387076, 1.000000000000000000, 0.8660254037844387076, 1.000000000000000000, 0.8660254037844387076, 1.000000000000000000, 0.8660254037844387076, 1.000000000000000000, 0.8660254037844387076, 1.000000000000000000, 0.8660254037844387076, 1.000000000000000000, 0.8660254037844387076, 1.000000000000000000, 0.8660254037844387076, 1.000000000000000000, 0.8660254037844387076, 1.000000000000000000, 0.8660254037844387076, 1.000000000000000000, 0.8660254037844387076, 1.000000000000000000, 0.8660254037844387076, 1.000000000000000000, 0.8660254037844387076, 1.000000000000000000, 0.8660254037844387076, 1.000000000000000000, 0.8660254037844387076, 1.000000000000000000, 0.8660254037844387076, 1.000000000000000000, 0.8660254037844387076, 1.000000000000000000, 0.8660254037844387076, 1.000000000000000000, 0.8660254037844387076, 1.000000000000000000, 0.8660254037844387076, 1.000000000000000000, 0.8660254037844387076, 1.000000000000000000, 0.8660254037844387076, 1.000000000000000000, 0.8660254037844387076, 1.000000000000000000, 0.8660254037844387076, 1.000000000000000000, 0.8660254037844387076, 1.000000000000000000, 0.8660254037844387076, 1.000000000000000000, 0.8660254037844387076, 1.000000000000000000, 0.8660254037844387076, 1.000000000000000000, 0.8660254037844387076, 1.000000000000000000, 0.8660254037844387076, 1.000000000000000000, 0.8660254037844387076, 1.000000000000000000, 0.8660254037844387076, 1.000000000000000000, 0.8660254037844387076, 1.000000000000000000, 0.8660254037844387076, 1.000000000000000000, 0.8660254037844387076, 1.000000000000000000, 0.8660254037844387076, 1.000000000000000000, 0.8660254037844387076, 1.000000000000000000, 0.8660254037844387076, 1.000000000000000000, 0.8660254037844387076, 1.000000000000000000, 0.8660254037844387076, 1.000000000000000000, 0.8660254037844387076, 1.000000000000000000, 0.8660254037844387076, 1.000000000000000000, 0.8660254037844387076, 1.000000000000000000, 0.8660254037844387076, 1.000000000000000000, 0.8660254037844387076, 1.000000000000000000, 0.8660254037844387076, 1.000000000000000000, 0.8660254037844387076, 1.000000000000000000, 0.8660254037844387076, 1.000000000000000000, 0.8660254037844387076, 1.000000000000000000, 0.8660254037844387076, 1.000000000000000000, 0.8660254037844387076, 1.000000000000000000, 0.8660254037844387076, 1.000000000000000000, 0.8660254037844387076, 1.000000000000000000, 0.8660254037844387076, 1.000000000000000000, 0.8660254037844387076, 1.000000000000000000, 0.8660254037844387076, 1.000000000000000000, 0.8660254037844387076, 1.000000000000000000, 0.8660254037844387076, 1.000000000000000000, 0.8660254037844387076, 1.000000000000000000, 0.8660254037844387076, 1.000000000000000000, 0.8660254037844387076, 1.000000000000000000, 0.8660254037844387076, 1.000000000000000000, 0.8660254037844387076, 1.000000000000000000, 0.8660254037844387076, 1.000000000000000000, 0.8660254037844387076, 1.000000000000000000, 0.8660254037844387076, 1.000000000000000000, 0.8660254037844387076, 1.000000000000000000, 0.8660254037844387076, 1.000000000000000000, 0.8660254037844387076, 1.000000000000000000, 0.8660254037844387076, 1.000000000000000000, 0.8660254037844387076, 1.000000000000000000, 0.8660254037844387076, 1.000000000000000000, 0.8660254037844387076, 1.000000000000000000, 0.8660254037844387076, 1.000000000000000000, 0.8660254037844387076, 1.000000000000000000, 0.8660254037844387076, 1.000000000000000000, 0.8660254037844387076, 1.000000000000000000, 0.8660254037844387076, 1.000000000000000000, 0.8660254037844387076, 1.000000000000000000, 0.8660254037844387076, 1.000000000000000000, 0.8660254037844387076, 1.000000000000000000, 0.8660254037844387076, 1.000000000000000000, 0.8660254037844387076, 1.000000000000000000, 0.8660254037844387076, 1.000000000000000000, 0.8660254037844387076, 1.000000000000000000, 0.8660254037844387076, 1.000000000000000000, 0.8660254037844387076, 1.000000000000000000, 0.8660254037844387076, 1.000000000000000000, 0.8660254037844387076, 1.000000000000000000, 0.8660254037844387076, 1.000000000000000000, 0.8660254037844387076, 1.000000000000000000, 0.8660254037844387076, 1.000000000000000000, 0.8660254037844387076, 1.000000000000000000, 0.8660254037844387076, 1.000000000000000000, 0.8660254037844387076, 1.000000000000000000, 0.8660254037844387076, 1.000000000000000000, 0.8660254037844387076, 1.000000000000000000, 0.8660254037844387076, 1.000000000000000000, 0.8660254037844387076, 1.000000000000000000, 0.8660254037844387076, 1.000000000000000000, 0.8660254037844387076, 1.000000000000000000, 0.8660254037844387076, 1.000000000000000000, 0.8660254037844387076, 1.000000000000000000, 0.8660254037844387076, 1.000000000000000000, 0.8660254037844387076, 1.000000000000000000, 0.8660254037844387076, 1.000000000000000000, 0.8660254037844387076, 1.000000000000000000, 0.8660254037844387076, 1.000000000000000000, 0.8660254037844387076, 1.000000000000000000, 0.8660254037844387076, 1.000000000000000000, 0.8660254037844387076, 1.000000000000000000, 0.8660254037844387076, 1.000000000000000000, 0.8660254037844387076, 1.000000000000000000, 0.8660254037844387076, 1.000000000000000000, 0.8660254037844387076, 1.000000000000000000, 0.8660254037844387076, 1.000000000000000000, 0.8660254037844387076, 1.000000000000000000, 0.8660254037844387076, 1.000000000000000000, 0.8660254037844387076, 1.000000000000000000, 0.8660254037844387076, 1.000000000000000000, 0.8660254037844387076, 1.000000000000000000, 0.8660254037844387076, 1.000000000000000000, 0.8660254037844387076, 1.000000000000000000, 0.8660254037844387076, 1.000000000000000000, 0.8660254037844387076, 1.000000000000000000, 0.8660254037844387076, 1.000000000000000000, 0.8660254037844387076, 1.000000000000000000, 0.8660254037844387076, 1.000000000000000000, 0.8660254037844387076, 1.000000000000000000, 0.8660254037844387076, 1.000000000000000000, 0.8660254037844387076, 1.000000000000000000, 0.8660254037844387076, 1.000000000000000000, 0.8660254037844387076, 1.000000000000000000, 0.8660254037844387076, 1.000000000000000000, 0.8660254037844387076, 1.000000000000000000, 0.8660254037844387076, 1.000000000000000000, 0.8660254037844387076, 1.000000000000000000, 0.8660254037844387076, 1.000000000000000000, 0.8660254037844387076, 1.000000000000000000, 0.8660254037844387076, 1.000000000000000000, 0.8660254037844387076, 1.000000000000000000, 0.8660254037844387076, 1.000000000000000000, 0.8660254037844387076, 1.000000000000000000, 0.8660254037844387076, 1.000000000000000000, 0.8660254037844387076, 1.000000000000000000, 0.8660254037844387076, 1.000000000000000000, 0.8660254037844387076, 1.000000000000000000, 0.8660254037844387076, 1.000000000000000000, 0.8660254037844387076, 1.000000000000000000, 0.8660254037844387076, 1.000000000000000000, 0.8660254037844387076, 1.000000000000000000, 0.8660254037844387076, 1.000000000000000000, 0.8660254037844387076, 1.000000000000000000, 0.8660254037844387076, 1.000000000000000000, 0.8660254037844387076, 1.000000000000000000, 0.8660254037844387076, 1.000000000000000000, 0.8660254037844387076, 1.000000000000000000, 0.8660254037844387076, 1.000000000000000000, 0.8660254037844387076, 1.000000000000000000, 0.8660254037844387076, 1.000000000000000000, 0.8660254037844387076, 1.000000000000000000, 0.8660254037844387076, 1.000000000000000000, 0.8660254037844387076, 1.000000000000000000, 0.8660254037844387076, 1.000000000000000000, 0.8660254037844387076, 1.000000000000000000, 0.8660254037844387076, 1.000000000000000000, 0.8660254037844387076, 1.000000000000000000, 0.8660254037844387076, 1.000000000000000000, 0.8660254037844387076, 1.000000000000000000, 0.8660254037844387076, 1.000000000000000000, 0.8660254037844387076, 1.000000000000000000, 0.8660254037844387076, 1.000000000000000000, 0.8660254037844387076, 1.000000000000000000, 0.8660254037844387076, 1.000000000000000000, 0.8660254037844387076, 1.000000000000000000, 0.8660254037844387076, 1.000000000000000000, 0.8660254037844387076, 1.000000000000000000, 0.8660254037844387076, 1.000000000000000000, 0.8660254037844387076, 1.000000000000000000, 0.8660254037844387076, 1.000000000000000000, 0.8660254037844387076, 1.000000000000000000, 0.8660254037844387076, 1.000000000000000000, 0.8660254037844387076, 1.000000000000000000, 0.8660254037844387076, 1.000000000000000000, 0.8660254037844387076, 1.000000000000000000, 0.8660254037844387076, 1.000000000000000000, 0.8660254037844387076, 1.000000000000000000, 0.8660254037844387076, 1.000000000000000000, 0.8660254037844387076, 1.000000000000000000, 0.8660254037844387076, 1.000000000000000000, 0.8660254037844387076, 1.000000000000000000, 0.8660254037844387076, 1.000000000000000000, 0.8660254037844387076, 1.000000000000000000, 0.8660254037844387076, 1.000000000000000000, 0.8660254037844387076, 1.000000000000000000, 0.8660254037844387076, 1.000000000000000000, 0.8660254037844387076, 1.000000000000000000, 0.8660254037844387076, 1.000000000000000000, 0.8660254037844387076, 1.000000000000000000, 0.8660254037844387076, 1.000000000000000000, 0.8660254037844387076, 1.000000000000000000, 0.8660254037844387076, 1.000000000000000000, 0.8660254037844387076, 1.000000000000000000, 0.8660254037844387076, 1.000000000000000000, 0.8660254037844387076, 1.000000000000000000, 0.8660254037844387076, 1.000000000000000000, 0.8660254037844387076, 1.000000000000000000, 0.8660254037844387076, 1.000000000000000000, 0.8660254037844387076, 1.000000000000000000, 0.8660254037844387076, 1.000000000000000000, 0.8660254037844387076, 1.000000000000000000, 0.8660254037844387076, 1.000000000000000000, 0.8660254037844387076, 1.000000000000000000, 0.8660254037844387076, 1.000000000000000000, 0.8660254037844387076, 1.000000000000000000, 0.8660254037844387076, 1.000000000000000000, 0.8660254037844387076, 1.000000000000000000, 0.8660254037844387076, 1.000000000000000000, 0.8660254037844387076, 1.000000000000000000, 0.8660254037844387076, 1.000000000000000000, 0.8660254037844387076, 1.000000000000000000, 0.8660254037844387076, 1.000000000000000000, 0.8660254037844387076, 1.000000000000000000, 0.8660254037844387076, 1.000000000000000000, 0.8660254037844387076, 1.000000000000000000, 0.8660254037844387076, 1.000000000000000000, 0.8660254037844387076, 1.000000000000000000, 0.8660254037844387076, 1.000000000000000000, 0.8660254037844387076, 1.000000000000000000, 0.8660254037844387076, 1.000000000000000000, 0.8660254037844387076, 1.000000000000000000, 0.8660254037844387076, 1.000000000000000000, 0.8660254037844387076, 1.000000000000000000, 0.8660254037844387076, 1.000000000000000000, 0.8660254037844387076, 1.000000000000000000, 0.8660254037844387076, 1.000000000000000000, 0.8660254037844387076, 1.000000000000000000, 0.8660254037844387076, 1.000000000000000000, 0.8660254037844387076, 1.000000000000000000, 0.8660254037844387076, 1.000000000000000000, 0.8660254037844387076, 1.000000000000000000, 0.8660254037844387076, 1.000000000000000000, 0.8660254037844387076, 1.000000000000000000, 0.8660254037844387076, 1.000000000000000000, 0.8660254037844387076, 1.000000000000000000, 0.8660254037844387076, 1.000000000000000000, 0.8660254037844387076, 1.000000000000000000, 0.8660254037844387076, 1.000000000000000000, 0.8660254037844387076, 1.000000000000000000, 0.8660254037844387076, 1.000000000000000000, 0.8660254037844387076, 1.000000000000000000, 0.8660254037844387076, 1.000000000000000000, 0.8660254037844387076, 1.000000000000000000, 0.8660254037844387076, 1.000000000000000000, 0.8660254037844387076, 1.000000000000000000, 0.8660254037844387076, 1.000000000000000000, 0.8660254037844387076, 1.000000000000000000, 0.8660254037844387076, 1.000000000000000000, 0.8660254037844387076, 1.000000000000000000, 0.8660254037844387076, 1.000000000000000000, 0.8660254037844387076, 1.000000000000000000, 0.8660254037844387076, 1.000000000000000000) ) ) 
 REPRESENTATION_ITEM ( '' )  SURFACE ( )  );
#45453 = CARTESIAN_POINT ( 'NONE',  ( 26.85937500061451644, -4.541064518000417216, -2.621784821875001281 ) ) ;
#45454 = ORIENTED_EDGE ( 'NONE', *, *, #65842, .F. ) ;
#45455 = CARTESIAN_POINT ( 'NONE',  ( 21.17812500061451431, 4.541064518000418104, 2.621784821874999949 ) ) ;
#45456 = CARTESIAN_POINT ( 'NONE',  ( 21.60937500061451644, 4.541064518000418104, -2.621784821874998173 ) ) ;
#45457 = CARTESIAN_POINT ( 'NONE',  ( 6.487499999999999822, 5.773502691896255534, 3.535250795749688894E-16 ) ) ;
#45458 = CARTESIAN_POINT ( 'NONE',  ( 10.37812500061451715, 4.541064518000418104, 2.621784821874999949 ) ) ;
#45459 = CARTESIAN_POINT ( 'NONE',  ( 24.70312500061451644, 4.541064518000418104, -2.621784821874998173 ) ) ;
#45460 = CARTESIAN_POINT ( 'NONE',  ( 11.97187500061451892, -6.054752690667223547, -1.112240025338166033E-15 ) ) ;
#45461 = CARTESIAN_POINT ( 'NONE',  ( 17.03437500061451715, 6.421520780324663323E-16, -5.243569643749999010 ) ) ;
#45462 = FACE_OUTER_BOUND ( 'NONE', #62100, .T. ) ;
#45463 = CARTESIAN_POINT ( 'NONE',  ( -3.000416591977282496E-16, 18.34062500061451928, 25.09994784771203058 ) ) ;
#45464 = CARTESIAN_POINT ( 'NONE',  ( 20.73750000122903359, -4.330127018922194537, 2.499999999999995559 ) ) ;
#45465 = CARTESIAN_POINT ( 'NONE',  ( 15.57187500061451857, -5.492252693125287522, -1.008910452111647106E-15 ) ) ;
#45466 = CARTESIAN_POINT ( 'NONE',  ( 11.01562500061451644, -6.054752690667223547, -1.112240025338166033E-15 ) ) ;
#45467 = CARTESIAN_POINT ( 'NONE',  ( 4.884375000614518569, 6.421520780324663323E-16, -5.243569643749999010 ) ) ;
#45468 = CARTESIAN_POINT ( 'NONE',  ( 5.184375000614516615, -4.541064518000419881, 2.621784821874995952 ) ) ;
#45469 = EDGE_LOOP ( 'NONE', ( #54998, #24799, #7603, #22935 ) ) ;
#45470 = CARTESIAN_POINT ( 'NONE',  ( 26.48437500061451644, 6.421520780324663323E-16, -5.243569643749999010 ) ) ;
#45471 = CARTESIAN_POINT ( 'NONE',  ( 16.07812500061451289, 6.421520780324663323E-16, -5.243569643749999010 ) ) ;
#45472 = CARTESIAN_POINT ( 'NONE',  ( 28.16250000122903074, 4.330127018922192761, -2.499999999999997780 ) ) ;
#45473 = CARTESIAN_POINT ( 'NONE',  ( 28.71562500061451573, 3.027376345333613106, -5.243569643749998122 ) ) ;
#45474 = CARTESIAN_POINT ( 'NONE',  ( 22.58437500061451431, 4.541064518000418104, 2.621784821874999949 ) ) ;
#45475 = CARTESIAN_POINT ( 'NONE',  ( 16.19062500061451715, 6.054752690667223547, 3.707466751127219781E-16 ) ) ;
#45476 = CARTESIAN_POINT ( 'NONE',  ( -3.999999999999997335, 10.58750000000000213, 32.30940107675850470 ) ) ;
#45477 = AXIS2_PLACEMENT_3D ( 'NONE', #28023, #9563, #10657 ) ;
#45478 = CARTESIAN_POINT ( 'NONE',  ( 22.56562500061451715, 3.027376345333611329, 5.243569643749999010 ) ) ;
#45479 = CARTESIAN_POINT ( 'NONE',  ( 4.575000001229033941, -5.773502691896255534, -1.060575238724906372E-15 ) ) ;
#45480 = ORIENTED_EDGE ( 'NONE', *, *, #22055, .F. ) ;
#45481 = CARTESIAN_POINT ( 'NONE',  ( 27.86249999999999716, -5.773502691896255534, -1.060575238724906372E-15 ) ) ;
#45482 = CARTESIAN_POINT ( 'NONE',  ( 3.999999999999998668, 12.61250000000000071, -32.30940107675850470 ) ) ;
#45483 = CARTESIAN_POINT ( 'NONE',  ( -3.756430356249999214, 17.89062499938548356, 27.83122392262697531 ) ) ;
#45484 = CARTESIAN_POINT ( 'NONE',  ( 28.79062500061451502, 6.054752690667223547, 3.707466751127219781E-16 ) ) ;
#45485 = CARTESIAN_POINT ( 'NONE',  ( 11.09062500061451573, -3.027376345333610441, -5.243569643749999898 ) ) ;
#45486 = CARTESIAN_POINT ( 'NONE',  ( 21.07500000122903572, 2.886751345948126879, 4.999999999999999112 ) ) ;
#45487 = AXIS2_PLACEMENT_3D ( 'NONE', #23625, #40631, #46171 ) ;
#45488 = CARTESIAN_POINT ( 'NONE',  ( 13.73437500061451821, -4.541064518000419881, 2.621784821874995952 ) ) ;
#45489 = CARTESIAN_POINT ( 'NONE',  ( 27.77812500061451573, 6.421520780324663323E-16, -5.243569643749999010 ) ) ;
#45490 = CARTESIAN_POINT ( 'NONE',  ( 27.33750000000000213, -2.886751345948129988, 4.999999999999997335 ) ) ;
#45491 = CARTESIAN_POINT ( 'NONE',  ( -1.999999999999997113, 19.28750000122903430, -26.53589838486224295 ) ) ;
#45492 = CARTESIAN_POINT ( 'NONE',  ( 12.77812500061451750, -4.541064518000419881, 2.621784821874995952 ) ) ;
#45493 = ORIENTED_EDGE ( 'NONE', *, *, #32022, .F. ) ;
#45494 = EDGE_CURVE ( 'NONE', #37790, #1400, #45406, .T. ) ;
#45495 = VECTOR ( 'NONE', #52784, 1000.000000000000000 ) ;
#45496 = CARTESIAN_POINT ( 'NONE',  ( 7.715625000614515727, 3.027376345333611329, 5.243569643749999010 ) ) ;
#45497 = AXIS2_PLACEMENT_3D ( 'NONE', #72256, #45275, #15360 ) ;
#45498 = CARTESIAN_POINT ( 'NONE',  ( 6.740625000614516082, 6.054752690667223547, 3.707466751127219781E-16 ) ) ;
#45499 = CARTESIAN_POINT ( 'NONE',  ( 16.28437500061452070, 4.119189519843966529, 2.378215178124999607 ) ) ;
#45500 = EDGE_CURVE ( 'NONE', #52141, #11866, #50901, .T. ) ;
#45501 = CARTESIAN_POINT ( 'NONE',  ( 2.700000001229035718, -2.886751345948129988, 4.999999999999997335 ) ) ;
#45502 = CARTESIAN_POINT ( 'NONE',  ( 16.61250000000000426, -5.773502691896255534, -1.060575238724906372E-15 ) ) ;
#45503 = ADVANCED_FACE ( 'NONE', ( #45728 ), #67539, .T. ) ;
#45504 = CARTESIAN_POINT ( 'NONE',  ( 15.79687500061451821, 6.054752690667223547, 3.707466751127219781E-16 ) ) ;
#45505 = CARTESIAN_POINT ( 'NONE',  ( 12.33750000122903145, 6.123233995736764310E-16, -4.999999999999998224 ) ) ;
#45506 = CARTESIAN_POINT ( 'NONE',  ( 20.48437500061451289, -4.541064518000419881, 2.621784821874995952 ) ) ;
#45507 = CARTESIAN_POINT ( 'NONE',  ( 19.79999999999999716, -4.330127018922190985, -2.500000000000001332 ) ) ;
#45508 = CARTESIAN_POINT ( 'NONE',  ( 19.92187500061451644, 3.027376345333611329, 5.243569643749999010 ) ) ;
#45509 = CARTESIAN_POINT ( 'NONE',  ( 9.001249775931846008E-16, 14.96562500061451750, -25.09994784771203058 ) ) ;
#45510 = FACE_OUTER_BOUND ( 'NONE', #31902, .T. ) ;
#45511 = CARTESIAN_POINT ( 'NONE',  ( 26.59687500061451360, 0.000000000000000000, 4.756430356249998326 ) ) ;
#45512 = CARTESIAN_POINT ( 'NONE',  ( 30.00000000000000000, 0.000000000000000000, 0.000000000000000000 ) ) ;
#45513 = CARTESIAN_POINT ( 'NONE',  ( 26.57812500061451644, 4.541064518000418104, 2.621784821874999949 ) ) ;
#45514 = CYLINDRICAL_SURFACE ( 'NONE', #19557, 4.999999999999998224 ) ;
#45515 = CARTESIAN_POINT ( 'NONE',  ( 28.73437500061451644, 6.421520780324663323E-16, -5.243569643749999010 ) ) ;
#45516 = CARTESIAN_POINT ( 'NONE',  ( 25.08749999999999858, -2.886751345948129988, 4.999999999999997335 ) ) ;
#45517 = CARTESIAN_POINT ( 'NONE',  ( 9.890625000614516438, 6.054752690667223547, 3.707466751127219781E-16 ) ) ;
#45518 = CARTESIAN_POINT ( 'NONE',  ( 25.54687500061451644, 4.119189519843966529, -2.378215178124998275 ) ) ;
#45519 = CARTESIAN_POINT ( 'NONE',  ( 18.75937500061451857, -4.541064518000417216, -2.621784821875001281 ) ) ;
#45520 = CARTESIAN_POINT ( 'NONE',  ( 10.47187500061451715, -4.119189519843968306, 2.378215178124996054 ) ) ;
#45521 = AXIS2_PLACEMENT_3D ( 'NONE', #70813, #59717, #32021 ) ;
#45522 = CARTESIAN_POINT ( 'NONE',  ( 6.290625000614517681, 6.054752690667223547, 3.707466751127219781E-16 ) ) ;
#45523 = CARTESIAN_POINT ( 'NONE',  ( 10.58437500061451964, -4.541064518000419881, 2.621784821874995952 ) ) ;
#45524 = ORIENTED_EDGE ( 'NONE', *, *, #17942, .T. ) ;
#45525 = CARTESIAN_POINT ( 'NONE',  ( 21.79687500061451644, -3.027376345333614438, 5.243569643749998122 ) ) ;
#45526 = CARTESIAN_POINT ( 'NONE',  ( 8.193750001229032520, -2.886751345948181946, -4.999999999999904077 ) ) ;
#45527 = CARTESIAN_POINT ( 'NONE',  ( 28.76249999999999929, -5.773502691896255534, -1.060575238724906372E-15 ) ) ;
#45529 = ADVANCED_FACE ( 'NONE', ( #67896 ), #22453, .T. ) ;
#45528 = CARTESIAN_POINT ( 'NONE',  ( 29.59687500061451715, -3.027376345333610441, -5.243569643749999898 ) ) ;
#45530 = CARTESIAN_POINT ( 'NONE',  ( 14.81250000122903288, 0.000000000000000000, 4.999999999999998224 ) ) ;
#45531 = CARTESIAN_POINT ( 'NONE',  ( 18.05625000122903501, -4.330127018922190985, -2.500000000000001332 ) ) ;
#45532 = CARTESIAN_POINT ( 'NONE',  ( 10.16250000000000320, 2.886751345948126879, 4.999999999999998224 ) ) ;
#45533 = ORIENTED_EDGE ( 'NONE', *, *, #16255, .T. ) ;
#45534 = CARTESIAN_POINT ( 'NONE',  ( 12.97499999999999964, -4.330127018922194537, 2.499999999999995559 ) ) ;
#45535 = CARTESIAN_POINT ( 'NONE',  ( 13.35937500061451644, 2.746126346562645981, -4.756430356249997438 ) ) ;
#45536 = CARTESIAN_POINT ( 'NONE',  ( 24.02812500061451573, -4.541064518000419881, 2.621784821874995952 ) ) ;
#45537 = CARTESIAN_POINT ( 'NONE',  ( 14.55000000000000071, 4.330127018922192761, -2.499999999999997780 ) ) ;
#45538 = CARTESIAN_POINT ( 'NONE',  ( 10.50000000122903465, -2.886751345948125991, -5.000000000000000000 ) ) ;
#45539 = CARTESIAN_POINT ( 'NONE',  ( 9.365625000614519635, 3.027376345333613106, -5.243569643749998122 ) ) ;
#45540 = CARTESIAN_POINT ( 'NONE',  ( 9.899999999999998579, -4.330127018922190985, -2.500000000000001332 ) ) ;
#45541 = DIRECTION ( 'NONE',  ( 0.000000000000000000, 1.000000000000000000, 0.000000000000000000 ) ) ;
#45542 = CARTESIAN_POINT ( 'NONE',  ( 27.67500000122903359, 2.886751345948129099, -4.999999999999998224 ) ) ;
#45543 = CARTESIAN_POINT ( 'NONE',  ( -7.967954043666661671E-16, 17.02812499938548285, 34.33755215474603517 ) ) ;
#45544 = CARTESIAN_POINT ( 'NONE',  ( 7.050000000000000711, 0.000000000000000000, 4.999999999999998224 ) ) ;
#45545 = ORIENTED_EDGE ( 'NONE', *, *, #62566, .T. ) ;
#45546 = CARTESIAN_POINT ( 'NONE',  ( 21.92812500061451431, 6.421520780324663323E-16, -5.243569643749999010 ) ) ;
#45547 = CARTESIAN_POINT ( 'NONE',  ( 28.34062500061451928, 6.054752690667223547, 3.707466751127219781E-16 ) ) ;
#45548 = AXIS2_PLACEMENT_3D ( 'NONE', #39728, #15709, #55615 ) ;
#45549 = CARTESIAN_POINT ( 'NONE',  ( 29.74687500061451217, 6.054752690667223547, 3.707466751127219781E-16 ) ) ;
#45550 = CARTESIAN_POINT ( 'NONE',  ( 20.18437500061451573, 6.421520780324663323E-16, -5.243569643749999010 ) ) ;
#45551 = CARTESIAN_POINT ( 'NONE',  ( 16.52812500061451573, 6.421520780324663323E-16, -5.243569643749999010 ) ) ;
#45552 = CARTESIAN_POINT ( 'NONE',  ( 2.121784821874999061, 11.55312500061459424, -33.67503911421598417 ) ) ;
#45553 = CARTESIAN_POINT ( 'NONE',  ( 5.728125000614515905, 6.421520780324663323E-16, -5.243569643749999010 ) ) ;
#45554 = CARTESIAN_POINT ( 'NONE',  ( 2.803125000614518747, 0.000000000000000000, 5.243569643749999010 ) ) ;
#45555 = CARTESIAN_POINT ( 'NONE',  ( 20.78437500061451715, 4.119189519843966529, 2.378215178124999607 ) ) ;
#45556 = CARTESIAN_POINT ( 'NONE',  ( 19.41562500061451502, 3.027376345333611329, 5.243569643749999010 ) ) ;
#45557 = DIRECTION ( 'NONE',  ( 0.000000000000000000, 0.000000000000000000, 1.000000000000000000 ) ) ;
#45558 = CARTESIAN_POINT ( 'NONE',  ( 3.187500001229033764, -4.330127018922194537, 2.499999999999995559 ) ) ;
#45559 = CARTESIAN_POINT ( 'NONE',  ( 12.30937500061451573, 0.000000000000000000, 5.243569643749999010 ) ) ;
#45560 = CARTESIAN_POINT ( 'NONE',  ( 11.40937500061451892, 0.000000000000000000, 5.243569643749999010 ) ) ;
#45561 = CARTESIAN_POINT ( 'NONE',  ( 20.55937500061451573, -4.541064518000417216, -2.621784821875001281 ) ) ;
#45562 = EDGE_LOOP ( 'NONE', ( #68813, #16357, #8830, #58850 ) ) ;
#45563 = CARTESIAN_POINT ( 'NONE',  ( -4.757043123249223626, 8.797129135976163639, 26.33838535627023347 ) ) ;
#45564 = CARTESIAN_POINT ( 'NONE',  ( 25.04062500061451502, -3.027376345333610441, -5.243569643749999898 ) ) ;
#45565 = CARTESIAN_POINT ( 'NONE',  ( 18.38437500061451857, 6.421520780324663323E-16, -5.243569643749999010 ) ) ;
#45566 = CARTESIAN_POINT ( 'NONE',  ( 25.45312500061451644, -4.541064518000417216, -2.621784821875001281 ) ) ;
#45567 = CARTESIAN_POINT ( 'NONE',  ( 17.30625000122903145, 4.330127018922192761, -2.499999999999997780 ) ) ;
#45568 = CARTESIAN_POINT ( 'NONE',  ( 3.999999999999999112, 17.07499999999999929, 30.00000000000000000 ) ) ;
#45569 = CARTESIAN_POINT ( 'NONE',  ( 4.996875000614516615, 6.054752690667223547, 3.707466751127219781E-16 ) ) ;
#45570 = CARTESIAN_POINT ( 'NONE',  ( 10.91250000122903252, -4.330127018922190985, -2.500000000000001332 ) ) ;
#45571 = CARTESIAN_POINT ( 'NONE',  ( 8.175000001229031810, -5.773502691896255534, -1.060575238724906372E-15 ) ) ;
#45572 = CARTESIAN_POINT ( 'NONE',  ( 28.91250000122903074, -4.330127018922190985, -2.500000000000001332 ) ) ;
#45573 = CARTESIAN_POINT ( 'NONE',  ( 27.93750000122903288, -4.330127018922194537, 2.499999999999995559 ) ) ;
#45574 = CARTESIAN_POINT ( 'NONE',  ( -4.000000000000000000, 18.51874999877096784, 30.00000000000000000 ) ) ;
#45575 = CARTESIAN_POINT ( 'NONE',  ( 15.95625000122903181, 4.330127018922192761, -2.499999999999997780 ) ) ;
#45576 = CARTESIAN_POINT ( 'NONE',  ( 10.69687500061451679, -3.027376345333610441, -5.243569643749999898 ) ) ;
#45577 = CARTESIAN_POINT ( 'NONE',  ( 17.84062500061451573, -3.027376345333610441, -5.243569643749999898 ) ) ;
#45578 = CARTESIAN_POINT ( 'NONE',  ( 13.65937500061451715, 0.000000000000000000, 5.243569643749999010 ) ) ;
#45579 = CARTESIAN_POINT ( 'NONE',  ( 29.02500000122903145, 2.886751345948129099, -4.999999999999998224 ) ) ;
#45580 = CARTESIAN_POINT ( 'NONE',  ( 20.29687500061451289, 6.054752690667223547, 3.707466751127219781E-16 ) ) ;
#45581 = CARTESIAN_POINT ( 'NONE',  ( 10.47187500061451715, 3.027376345333611329, 5.243569643749999010 ) ) ;
#45582 = CARTESIAN_POINT ( 'NONE',  ( 3.093393010629925666, -3.928220930877811767, -3.281160880885886311 ) ) ;
#45583 = CARTESIAN_POINT ( 'NONE',  ( 1.999999999999997335, 16.02500000000000213, 33.46410161513775705 ) ) ;
#45584 = CARTESIAN_POINT ( 'NONE',  ( 20.12812500061451715, 6.421520780324663323E-16, -5.243569643749999010 ) ) ;
#45585 = ORIENTED_EDGE ( 'NONE', *, *, #12396, .F. ) ;
#45586 = CARTESIAN_POINT ( 'NONE',  ( 6.750000001229033764, -2.886751345948129988, 4.999999999999997335 ) ) ;
#45587 = CARTESIAN_POINT ( 'NONE',  ( 17.27812500061451217, -4.541064518000419881, 2.621784821874995952 ) ) ;
#45588 = CARTESIAN_POINT ( 'NONE',  ( 12.51562500061451821, 3.027376345333613106, -5.243569643749998122 ) ) ;
#45589 = CARTESIAN_POINT ( 'NONE',  ( 25.13437500061451502, 5.824947211148865298E-16, -4.756430356249998326 ) ) ;
#45590 = CARTESIAN_POINT ( 'NONE',  ( 14.40000000000000036, -4.330127018922190985, -2.500000000000001332 ) ) ;
#45591 = CARTESIAN_POINT ( 'NONE',  ( 9.375000001229036428, 2.886751345948126879, 4.999999999999999112 ) ) ;
#45592 = PRODUCT ( 'MAS-181', 'MAS-181', '', ( #15288 ) ) ;
#45593 = CARTESIAN_POINT ( 'NONE',  ( 6.515625000614516438, -6.054752690667223547, -1.112240025338166033E-15 ) ) ;
#45594 =( BOUNDED_CURVE ( )  B_SPLINE_CURVE ( 3, ( #350, #37964, #23224, #34673 ),
 .UNSPECIFIED., .F., .F. ) 
 B_SPLINE_CURVE_WITH_KNOTS ( ( 4, 4 ),
 ( 3.765666616430975555, 3.802312977632561708 ),
 .UNSPECIFIED. ) 
 CURVE ( )  GEOMETRIC_REPRESENTATION_ITEM ( )  RATIONAL_B_SPLINE_CURVE ( ( 1.000000000000000000, 0.9998880901486507655, 0.9998880901486507655, 1.000000000000000000 ) ) 
 REPRESENTATION_ITEM ( '' )  );
#45595 = EDGE_CURVE ( 'NONE', #25370, #675, #38727, .T. ) ;
#45596 = CARTESIAN_POINT ( 'NONE',  ( 18.78750000122903430, 4.330127018922191873, 2.499999999999999556 ) ) ;
#45597 = CARTESIAN_POINT ( 'NONE',  ( 28.08749999999999858, 5.773502691896255534, 3.535250795749688894E-16 ) ) ;
#45598 = CARTESIAN_POINT ( 'NONE',  ( -2.121784821874996840, 11.38437500061451679, -26.32496088578401583 ) ) ;
#45599 = CARTESIAN_POINT ( 'NONE',  ( 4.494741915665277254, -2.190272839526016924, 4.494741915664858922 ) ) ;
#45600 = CARTESIAN_POINT ( 'NONE',  ( 3.562500001229033764, 0.000000000000000000, 4.999999999999998224 ) ) ;
#45601 = CARTESIAN_POINT ( 'NONE',  ( 5.810221930991193690E-16, 18.40624999877096357, 26.00000000000000000 ) ) ;
#45602 = CARTESIAN_POINT ( 'NONE',  ( 18.42187500061451644, 3.027376345333613106, -5.243569643749998122 ) ) ;
#45603 = CARTESIAN_POINT ( 'NONE',  ( 21.56250000122903288, 0.000000000000000000, 4.999999999999998224 ) ) ;
#45604 = CARTESIAN_POINT ( 'NONE',  ( 16.37812500061451715, -4.541064518000419881, 2.621784821874995952 ) ) ;
#45605 = CARTESIAN_POINT ( 'NONE',  ( 9.093750001229032875, -2.886751345948125991, -5.000000000000000000 ) ) ;
#45606 = CARTESIAN_POINT ( 'NONE',  ( 28.47187500061451715, 3.027376345333611329, 5.243569643749999010 ) ) ;
#45607 = CARTESIAN_POINT ( 'NONE',  ( 26.29687500061451644, -3.027376345333614438, 5.243569643749998122 ) ) ;
#45608 = CARTESIAN_POINT ( 'NONE',  ( 18.75937500061451857, 2.746126346562645981, -4.756430356249997438 ) ) ;
#45609 = CARTESIAN_POINT ( 'NONE',  ( 13.64062500061451644, -3.027376345333614438, 5.243569643749998122 ) ) ;
#45610 = CARTESIAN_POINT ( 'NONE',  ( 10.09687500061451715, -3.027376345333614438, 5.243569643749998122 ) ) ;
#45611 = VERTEX_POINT ( 'NONE', #40185 ) ;
#45612 = CIRCLE ( 'NONE', #30249, 1.500000000000000444 ) ;
#45613 = CARTESIAN_POINT ( 'NONE',  ( 29.39062500061451289, -3.027376345333614438, 5.243569643749998122 ) ) ;
#45614 = CARTESIAN_POINT ( 'NONE',  ( 20.27812500061451573, 4.541064518000418104, 2.621784821874999949 ) ) ;
#45615 = CARTESIAN_POINT ( 'NONE',  ( 27.86249999999999716, -5.773502691896255534, -1.060575238724906372E-15 ) ) ;
#45616 = CARTESIAN_POINT ( 'NONE',  ( 20.85000000000000142, 4.330127018922192761, -2.499999999999997780 ) ) ;
#45617 = CARTESIAN_POINT ( 'NONE',  ( 10.83750000000000036, -2.886751345948125991, -5.000000000000000000 ) ) ;
#45618 = CARTESIAN_POINT ( 'NONE',  ( 21.41250000122903074, 4.330127018922192761, -2.499999999999997780 ) ) ;
#45619 = CARTESIAN_POINT ( 'NONE',  ( 16.75312500061451715, 0.000000000000000000, 5.243569643749999010 ) ) ;
#45620 = CARTESIAN_POINT ( 'NONE',  ( 13.09687500061451715, 0.000000000000000000, 4.756430356249998326 ) ) ;
#45621 = ORIENTED_EDGE ( 'NONE', *, *, #39082, .T. ) ;
#45622 = CARTESIAN_POINT ( 'NONE',  ( 19.16250000000000142, 2.886751345948126879, 4.999999999999999112 ) ) ;
#45623 = CARTESIAN_POINT ( 'NONE',  ( 21.48750000000000071, -2.886751345948129988, 4.999999999999997335 ) ) ;
#45624 = CARTESIAN_POINT ( 'NONE',  ( 20.25937500061451857, 4.541064518000418104, -2.621784821874998173 ) ) ;
#45625 = CARTESIAN_POINT ( 'NONE',  ( 25.94062500061451715, -3.027376345333610441, -5.243569643749999898 ) ) ;
#45626 = ORIENTED_EDGE ( 'NONE', *, *, #31751, .F. ) ;
#45627 = CARTESIAN_POINT ( 'NONE',  ( 28.64999999999999858, 0.000000000000000000, 4.999999999999998224 ) ) ;
#45628 = CARTESIAN_POINT ( 'NONE',  ( 9.028125000614517504, 4.541064518000418104, 2.621784821874999949 ) ) ;
#45629 = CARTESIAN_POINT ( 'NONE',  ( 1.999999999999998668, 12.20000000000000107, 26.53589838486224650 ) ) ;
#45630 = AXIS2_PLACEMENT_3D ( 'NONE', #10784, #62118, #22586 ) ;
#45631 = CARTESIAN_POINT ( 'NONE',  ( 14.13750000000000107, 5.773502691896255534, 3.535250795749688894E-16 ) ) ;
#45632 = CARTESIAN_POINT ( 'NONE',  ( 2.121784821874999061, 16.95312500061451999, 26.32496088578401583 ) ) ;
#45633 = CARTESIAN_POINT ( 'NONE',  ( 28.30312500061451431, 4.541064518000418104, -2.621784821874998173 ) ) ;
#45634 = CARTESIAN_POINT ( 'NONE',  ( 27.19687500061451857, -3.027376345333614438, 5.243569643749998122 ) ) ;
#45635 = EDGE_LOOP ( 'NONE', ( #48697, #36536, #15948, #25226 ) ) ;
#45636 = CARTESIAN_POINT ( 'NONE',  ( 24.40312500061451573, 0.000000000000000000, 5.243569643749999010 ) ) ;
#45637 = CARTESIAN_POINT ( 'NONE',  ( 24.15937500061451715, -4.541064518000417216, -2.621784821875001281 ) ) ;
#45638 = ADVANCED_FACE ( 'NONE', ( #62706 ), #57152, .T. ) ;
#45639 = CARTESIAN_POINT ( 'NONE',  ( 9.001249775931846008E-16, 18.56562500061459886, -25.09994784771203058 ) ) ;
#45640 = CARTESIAN_POINT ( 'NONE',  ( 12.22499999999999964, 6.123233995736764310E-16, -4.999999999999998224 ) ) ;
#45641 = CARTESIAN_POINT ( 'NONE',  ( 8.878125000614515372, 6.421520780324663323E-16, -5.243569643749999010 ) ) ;
#45642 = CARTESIAN_POINT ( 'NONE',  ( 28.62187500061451573, -5.492252693125287522, -1.008910452111647106E-15 ) ) ;
#45643 = CARTESIAN_POINT ( 'NONE',  ( 26.84062500061451573, -3.027376345333610441, -5.243569643749999898 ) ) ;
#45644 = CARTESIAN_POINT ( 'NONE',  ( 22.51875000122903003, -5.773502691896255534, -1.060575238724906372E-15 ) ) ;
#45645 = CARTESIAN_POINT ( 'NONE',  ( 13.35937500061451821, -4.119189519843965641, -2.378215178125001383 ) ) ;
#45646 = CARTESIAN_POINT ( 'NONE',  ( 20.29687500061451644, 6.054752690667223547, 3.707466751127219781E-16 ) ) ;
#45647 = CARTESIAN_POINT ( 'NONE',  ( -4.243569643749999898, 15.77187500061451608, 27.54997392385601529 ) ) ;
#45648 = CARTESIAN_POINT ( 'NONE',  ( 19.50937500061451857, 0.000000000000000000, 5.243569643749999010 ) ) ;
#45649 = CARTESIAN_POINT ( 'NONE',  ( 27.45937500061451786, 4.541064518000418104, -2.621784821874998173 ) ) ;
#45650 = CARTESIAN_POINT ( 'NONE',  ( -4.243569643749999898, 17.15937500061451715, 30.00000000000000000 ) ) ;
#45651 = CARTESIAN_POINT ( 'NONE',  ( 8.990625000614516082, 6.054752690667223547, 3.707466751127219781E-16 ) ) ;
#45653 =( BOUNDED_CURVE ( )  B_SPLINE_CURVE ( 2, ( #10565, #6109, #67456, #22724, #67095, #5388, #61526, #51178, #582 ),
 .UNSPECIFIED., .F., .F. ) 
 B_SPLINE_CURVE_WITH_KNOTS ( ( 3, 2, 2, 2, 3 ),
 ( 0.1630434782608695676, 0.1666666666666666574, 0.1739130434782608647, 0.1811594202898550721, 0.1847826086956521896 ),
 .UNSPECIFIED. ) 
 CURVE ( )  GEOMETRIC_REPRESENTATION_ITEM ( )  RATIONAL_B_SPLINE_CURVE ( ( 0.9330127018922194093, 0.9330127018922196314, 1.000000000000000000, 0.8660254037844387076, 1.000000000000000000, 0.8660254037844387076, 1.000000000000000000, 0.9330127018922190762, 0.9330127018922194093 ) ) 
 REPRESENTATION_ITEM ( '' )  );
#45652 = CARTESIAN_POINT ( 'NONE',  ( 65.00000000000000000, -8.874999999999998224, 1.494782592887675232 ) ) ;
#45654 = CARTESIAN_POINT ( 'NONE',  ( 4.621875000614516615, 3.027376345333611329, 5.243569643749999010 ) ) ;
#45655 = CARTESIAN_POINT ( 'NONE',  ( 45.00000000000000000, 0.000000000000000000, 0.000000000000000000 ) ) ;
#45656 = CARTESIAN_POINT ( 'NONE',  ( 7.153125000614518392, 4.541064518000418104, -2.621784821874998173 ) ) ;
#45657 = CARTESIAN_POINT ( 'NONE',  ( 10.92187500061451644, 3.027376345333611329, 5.243569643749999010 ) ) ;
#45658 = CARTESIAN_POINT ( 'NONE',  ( 19.16250000122903430, 4.330127018922192761, -2.499999999999997780 ) ) ;
#45659 = CARTESIAN_POINT ( 'NONE',  ( 6.646875000614518747, -3.027376345333610441, -5.243569643749999898 ) ) ;
#45660 = CARTESIAN_POINT ( 'NONE',  ( 6.740625000614516082, 6.054752690667223547, 3.707466751127219781E-16 ) ) ;
#45661 = CARTESIAN_POINT ( 'NONE',  ( 5.353125000614515905, 4.541064518000418104, -2.621784821874998173 ) ) ;
#45662 = CARTESIAN_POINT ( 'NONE',  ( 23.68125000122903145, 4.330127018922191873, 2.499999999999999556 ) ) ;
#45663 = CARTESIAN_POINT ( 'NONE',  ( 19.80937500061451573, 4.541064518000418104, -2.621784821874998173 ) ) ;
#45664 = CARTESIAN_POINT ( 'NONE',  ( 4.428044609675158227, 2.322158679919935409, 4.428044609675073850 ) ) ;
#45665 = VERTEX_POINT ( 'NONE', #22094 ) ;
#45666 = CARTESIAN_POINT ( 'NONE',  ( 23.69062500061451004, -3.027376345333610441, -5.243569643749999898 ) ) ;
#45667 = CARTESIAN_POINT ( 'NONE',  ( 11.72812500061451857, 4.541064518000418104, 2.621784821874999949 ) ) ;
#45668 = CARTESIAN_POINT ( 'NONE',  ( 25.77187500061451431, 3.027376345333611329, 5.243569643749999010 ) ) ;
#45669 = CARTESIAN_POINT ( 'NONE',  ( 9.253125000614517148, -4.541064518000417216, -2.621784821875001281 ) ) ;
#45670 = CARTESIAN_POINT ( 'NONE',  ( 12.67500000122903536, -5.773502691896255534, -1.060575238724906372E-15 ) ) ;
#45671 = CARTESIAN_POINT ( 'NONE',  ( 26.24062500061451431, -3.027376345333614438, 5.243569643749998122 ) ) ;
#45672 = CARTESIAN_POINT ( 'NONE',  ( -4.243569643749997233, 13.09062500061451750, -27.54997392385601174 ) ) ;
#45673 = CARTESIAN_POINT ( 'NONE',  ( 14.55000000122903181, -2.886751345948125991, -5.000000000000000000 ) ) ;
#45674 = CARTESIAN_POINT ( 'NONE',  ( 10.76250000000000107, -5.773502691896255534, -1.060575238724906372E-15 ) ) ;
#45675 = CARTESIAN_POINT ( 'NONE',  ( 21.02812500061451573, 6.421520780324663323E-16, -5.243569643749999010 ) ) ;
#45676 = CARTESIAN_POINT ( 'NONE',  ( 8.409375000614518925, -4.541064518000417216, -2.621784821875001281 ) ) ;
#45677 = CARTESIAN_POINT ( 'NONE',  ( 7.875000001229034652, 2.886751345948129099, -4.999999999999998224 ) ) ;
#45678 = EDGE_CURVE ( 'NONE', #65643, #46924, #63729, .T. ) ;
#45679 = CARTESIAN_POINT ( 'NONE',  ( 17.10000000122903430, -2.886751345948129988, 4.999999999999997335 ) ) ;
#45680 = AXIS2_PLACEMENT_3D ( 'NONE', #37055, #59580, #65500 ) ;
#45681 = CARTESIAN_POINT ( 'NONE',  ( 13.79062500061451502, -3.027376345333610441, -5.243569643749999898 ) ) ;
#45682 = CARTESIAN_POINT ( 'NONE',  ( 16.22812500061451857, 4.541064518000418104, 2.621784821874999949 ) ) ;
#45683 = ADVANCED_FACE ( 'NONE', ( #52710 ), #24628, .F. ) ;
#45684 = CARTESIAN_POINT ( 'NONE',  ( 26.51250000122903216, 0.000000000000000000, 4.999999999999998224 ) ) ;
#45685 = CARTESIAN_POINT ( 'NONE',  ( 20.13749999999999929, -2.886751345948129988, 4.999999999999997335 ) ) ;
#45686 = CARTESIAN_POINT ( 'NONE',  ( 22.47187500061451715, 3.027376345333613106, -5.243569643749998122 ) ) ;
#45687 = CARTESIAN_POINT ( 'NONE',  ( 2.000000000000000444, 13.92500000000000071, 26.53589838486224650 ) ) ;
#45688 = CARTESIAN_POINT ( 'NONE',  ( 9.225000001229034297, 2.886751345948129099, -4.999999999999998224 ) ) ;
#45689 = CARTESIAN_POINT ( 'NONE',  ( 8.259375000614518569, 0.000000000000000000, 5.243569643749999010 ) ) ;
#45690 = CARTESIAN_POINT ( 'NONE',  ( 29.14687500061451075, -3.027376345333610441, -5.243569643749999898 ) ) ;
#45691 = CARTESIAN_POINT ( 'NONE',  ( 23.81250000000000000, -5.773502691896255534, -1.060575238724906372E-15 ) ) ;
#45692 = CARTESIAN_POINT ( 'NONE',  ( 24.55312500061451786, -4.541064518000417216, -2.621784821875001281 ) ) ;
#45693 = CARTESIAN_POINT ( 'NONE',  ( 1.878215178125000495, 15.07812499938548179, 26.74683588394047007 ) ) ;
#45694 = CARTESIAN_POINT ( 'NONE',  ( 26.04375000122903216, -2.886751345948143310, 4.999999999999972466 ) ) ;
#45695 = CARTESIAN_POINT ( 'NONE',  ( 8.934375000614517504, 6.421520780324663323E-16, -5.243569643749999010 ) ) ;
#45696 = CARTESIAN_POINT ( 'NONE',  ( 23.58750000122903145, 6.123233995736764310E-16, -4.999999999999998224 ) ) ;
#45697 = CARTESIAN_POINT ( 'NONE',  ( 27.36562500061451786, 3.027376345333613106, -5.243569643749998122 ) ) ;
#45698 = CARTESIAN_POINT ( 'NONE',  ( 6.909375000614518036, 0.000000000000000000, 5.243569643749999010 ) ) ;
#45699 = DIRECTION ( 'NONE',  ( 0.000000000000000000, -0.000000000000000000, 1.000000000000000000 ) ) ;
#45700 = CARTESIAN_POINT ( 'NONE',  ( 25.20937500061451431, 4.541064518000418104, -2.621784821874998173 ) ) ;
#45701 = CARTESIAN_POINT ( 'NONE',  ( -4.243569643749999898, 11.21562500061459389, 27.54997392385601529 ) ) ;
#45702 = CARTESIAN_POINT ( 'NONE',  ( 18.63749999999999929, 5.773502691896255534, 3.535250795749688894E-16 ) ) ;
#45703 = EDGE_LOOP ( 'NONE', ( #60924, #60124, #28814, #57730 ) ) ;
#45704 = CARTESIAN_POINT ( 'NONE',  ( 26.77499999999999858, 4.330127018922191873, 2.499999999999999556 ) ) ;
#45705 = CARTESIAN_POINT ( 'NONE',  ( 27.79687500061451999, -3.027376345333610441, -5.243569643749999898 ) ) ;
#45706 = ORIENTED_EDGE ( 'NONE', *, *, #10971, .T. ) ;
#45707 = CARTESIAN_POINT ( 'NONE',  ( 14.42812500061451786, 4.541064518000418104, 2.621784821874999949 ) ) ;
#45708 = CARTESIAN_POINT ( 'NONE',  ( 7.828125000614517326, -4.541064518000419881, 2.621784821874995952 ) ) ;
#45709 = CARTESIAN_POINT ( 'NONE',  ( 17.85937500061451644, 2.746126346562645981, -4.756430356249997438 ) ) ;
#45710 = CARTESIAN_POINT ( 'NONE',  ( 5.746875000614517504, -3.027376345333610441, -5.243569643749999898 ) ) ;
#45711 = CARTESIAN_POINT ( 'NONE',  ( 18.45000000122903216, -2.886751345948129988, 4.999999999999997335 ) ) ;
#45712 = CARTESIAN_POINT ( 'NONE',  ( 22.83749999999999858, -2.886751345948129988, 4.999999999999997335 ) ) ;
#45713 = CARTESIAN_POINT ( 'NONE',  ( 29.13749999999999929, -2.886751345948129988, 4.999999999999997335 ) ) ;
#45714 = CARTESIAN_POINT ( 'NONE',  ( 4.246875000614519280, -3.027376345333614438, 5.243569643749998122 ) ) ;
#45715 = CARTESIAN_POINT ( 'NONE',  ( 12.68437500061451573, 4.541064518000418104, 2.621784821874999949 ) ) ;
#45716 = CARTESIAN_POINT ( 'NONE',  ( 22.47187500061451715, 3.027376345333613106, -5.243569643749998122 ) ) ;
#45717 = DIRECTION ( 'NONE',  ( -0.000000000000000000, -1.000000000000000000, -0.000000000000000000 ) ) ;
#45718 = ORIENTED_EDGE ( 'NONE', *, *, #7133, .F. ) ;
#45719 = CARTESIAN_POINT ( 'NONE',  ( 4.396875000614516971, -3.027376345333610441, -5.243569643749999898 ) ) ;
#45720 = CARTESIAN_POINT ( 'NONE',  ( 8.071875000614518569, 3.027376345333613106, -5.243569643749998122 ) ) ;
#45721 = CARTESIAN_POINT ( 'NONE',  ( 17.73750000000000071, 5.773502691896255534, 3.535250795749688894E-16 ) ) ;
#45722 = CARTESIAN_POINT ( 'NONE',  ( 16.07812500061451289, 6.421520780324663323E-16, -5.243569643749999010 ) ) ;
#45723 = CARTESIAN_POINT ( 'NONE',  ( 4.000000000000000000, 20.18750000000000000, 27.69059892324149530 ) ) ;
#45724 = CARTESIAN_POINT ( 'NONE',  ( 45.00000000000000000, 0.000000000000000000, 0.000000000000000000 ) ) ;
#45725 = CARTESIAN_POINT ( 'NONE',  ( 19.69687500061451857, -2.746126346562642428, -4.756430356249999214 ) ) ;
#45726 = CARTESIAN_POINT ( 'NONE',  ( 9.740625000614516082, -3.027376345333610441, -5.243569643749999898 ) ) ;
#45727 = CARTESIAN_POINT ( 'NONE',  ( 25.58437500061451431, 6.421520780324663323E-16, -5.243569643749999010 ) ) ;
#45728 = FACE_OUTER_BOUND ( 'NONE', #60690, .T. ) ;
#45729 = CARTESIAN_POINT ( 'NONE',  ( 25.47187500061451715, -6.054752690667223547, -1.112240025338166033E-15 ) ) ;
#45730 = CARTESIAN_POINT ( 'NONE',  ( 6.337499999999998579, -2.886751345948125991, -5.000000000000000000 ) ) ;
#45731 = CARTESIAN_POINT ( 'NONE',  ( 8.484601909799253346E-16, 12.57500000122903216, 34.61880215351700230 ) ) ;
#45732 = CARTESIAN_POINT ( 'NONE',  ( 8.062500001229034652, 0.000000000000000000, 4.999999999999998224 ) ) ;
#45733 = CARTESIAN_POINT ( 'NONE',  ( 20.89687500061452141, -3.027376345333614438, 5.243569643749998122 ) ) ;
#45734 = CARTESIAN_POINT ( 'NONE',  ( 12.12187500061451573, 3.027376345333613106, -5.243569643749998122 ) ) ;
#45735 = CARTESIAN_POINT ( 'NONE',  ( -3.462385672708551798, 3.612013013662439764, -32.01854131409610460 ) ) ;
#45736 = VERTEX_POINT ( 'NONE', #68623 ) ;
#45737 = CARTESIAN_POINT ( 'NONE',  ( 15.17812500061451608, 6.421520780324663323E-16, -5.243569643749999010 ) ) ;
#45738 = CARTESIAN_POINT ( 'NONE',  ( 25.53750000122903074, 4.330127018922191873, 2.499999999999999556 ) ) ;
#45739 = CARTESIAN_POINT ( 'NONE',  ( 12.87187500061451750, -6.054752690667223547, -1.112240025338166033E-15 ) ) ;
#45740 = CARTESIAN_POINT ( 'NONE',  ( 3.999999999999999112, 12.68750000122903465, 30.00000000000000000 ) ) ;
#45741 = CARTESIAN_POINT ( 'NONE',  ( 16.94062500061451715, -3.027376345333610441, -5.243569643749999898 ) ) ;
#45742 = CARTESIAN_POINT ( 'NONE',  ( 26.40000000122903145, 5.773502691896255534, 3.535250795749688401E-16 ) ) ;
#45743 = CARTESIAN_POINT ( 'NONE',  ( 27.15937500061451360, 0.000000000000000000, 5.243569643749999010 ) ) ;
#45744 = CARTESIAN_POINT ( 'NONE',  ( 2.121784821875001281, 11.40312500061451750, 33.67503911421598417 ) ) ;
#45745 = CARTESIAN_POINT ( 'NONE',  ( 10.68750000122903288, 4.330127018922191873, 2.499999999999999556 ) ) ;
#45746 = CARTESIAN_POINT ( 'NONE',  ( 8.184375000614515727, 4.119189519843966529, 2.378215178124999607 ) ) ;
#45747 = CARTESIAN_POINT ( 'NONE',  ( -2.121784821874996840, 17.23437500061451999, -26.32496088578401583 ) ) ;
#45748 = CARTESIAN_POINT ( 'NONE',  ( 17.18437500061451573, 4.541064518000418104, 2.621784821874999949 ) ) ;
#45749 = CARTESIAN_POINT ( 'NONE',  ( 20.36250000122903359, -4.330127018922190985, -2.500000000000001332 ) ) ;
#45750 = CARTESIAN_POINT ( 'NONE',  ( 14.82187500061451679, 3.027376345333613106, -5.243569643749998122 ) ) ;
#45751 = EDGE_CURVE ( 'NONE', #13665, #69611, #71294, .T. ) ;
#45752 = CARTESIAN_POINT ( 'NONE',  ( 4.243569643749999898, 19.57812500061451644, -30.00000000000000000 ) ) ;
#45753 = CARTESIAN_POINT ( 'NONE',  ( 22.95000000122903216, -2.886751345948129988, 4.999999999999997335 ) ) ;
#45754 = CARTESIAN_POINT ( 'NONE',  ( 14.69062500061451537, -3.027376345333610441, -5.243569643749999898 ) ) ;
#45755 = CARTESIAN_POINT ( 'NONE',  ( 29.46562500061451573, -6.054752690667223547, -1.112240025338166033E-15 ) ) ;
#45756 = ORIENTED_EDGE ( 'NONE', *, *, #48081, .T. ) ;
#45757 = ORIENTED_EDGE ( 'NONE', *, *, #51752, .F. ) ;
#45758 = CARTESIAN_POINT ( 'NONE',  ( 19.31250000000000000, -5.773502691896255534, -1.060575238724906372E-15 ) ) ;
#45759 = CARTESIAN_POINT ( 'NONE',  ( -4.243569643749999898, 19.85937500061451644, 30.00000000000000000 ) ) ;
#45760 = CARTESIAN_POINT ( 'NONE',  ( 3.628125000614518036, 4.541064518000418104, 2.621784821874999949 ) ) ;
#45761 = CARTESIAN_POINT ( 'NONE',  ( 15.00000000122903465, -2.886751345948125991, -5.000000000000000000 ) ) ;
#45762 = CARTESIAN_POINT ( 'NONE',  ( 20.24062500061451431, 6.054752690667223547, 3.707466751127219781E-16 ) ) ;
#45763 = CARTESIAN_POINT ( 'NONE',  ( 23.87812500061451715, 4.541064518000418104, 2.621784821874999949 ) ) ;
#45764 = CARTESIAN_POINT ( 'NONE',  ( 3.965625000614515727, 3.027376345333613106, -5.243569643749998122 ) ) ;
#45765 = ADVANCED_FACE ( 'NONE', ( #47535 ), #18460, .T. ) ;
#45766 = CARTESIAN_POINT ( 'NONE',  ( 1.592000809091587073E-14, 16.40000000122903501, 26.00000000000000000 ) ) ;
#45767 = CARTESIAN_POINT ( 'NONE',  ( 23.02499999999999858, 6.123233995736764310E-16, -4.999999999999998224 ) ) ;
#45768 = CARTESIAN_POINT ( 'NONE',  ( 8.671875000614518214, 2.746126346562643317, 4.756430356249998326 ) ) ;
#45769 = CARTESIAN_POINT ( 'NONE',  ( 29.63437500061451502, 6.421520780324663323E-16, -5.243569643749999010 ) ) ;
#45770 = CARTESIAN_POINT ( 'NONE',  ( 2.000000000000001332, 10.36250000122903359, -26.53589838486224650 ) ) ;
#45771 = CARTESIAN_POINT ( 'NONE',  ( -4.243569643749999898, 19.40937500061451715, -30.00000000000000000 ) ) ;
#45772 = CARTESIAN_POINT ( 'NONE',  ( 6.000000001229033764, -2.886751345948125991, -5.000000000000000000 ) ) ;
#45773 = CARTESIAN_POINT ( 'NONE',  ( 8.400000000000000355, 0.000000000000000000, 4.999999999999998224 ) ) ;
#45774 = EDGE_CURVE ( 'NONE', #26212, #38561, #39302, .T. ) ;
#45775 = CARTESIAN_POINT ( 'NONE',  ( 4.950000001229033941, -2.886751345948129988, 4.999999999999997335 ) ) ;
#45776 = CARTESIAN_POINT ( 'NONE',  ( 12.30937500061451573, 0.000000000000000000, 5.243569643749999010 ) ) ;
#45777 = CARTESIAN_POINT ( 'NONE',  ( 1.071796769724484344, 16.64509619066136992, -25.99999999999999645 ) ) ;
#45778 = CARTESIAN_POINT ( 'NONE',  ( 2.934375000614518392, -4.541064518000419881, 2.621784821874995952 ) ) ;
#45779 = CARTESIAN_POINT ( 'NONE',  ( 3.999999999999998668, 19.02500000122903501, 27.69059892324149530 ) ) ;
#45780 = CARTESIAN_POINT ( 'NONE',  ( 1.999999999999998668, 19.51250000122903216, 26.53589838486224650 ) ) ;
#45781 = CARTESIAN_POINT ( 'NONE',  ( 10.32187500061451679, 3.027376345333613106, -5.243569643749998122 ) ) ;
#45782 = CARTESIAN_POINT ( 'NONE',  ( 13.13437500061451857, 4.541064518000418104, 2.621784821874999949 ) ) ;
#45783 = CARTESIAN_POINT ( 'NONE',  ( 9.528763966825557376E-15, 17.07500000122903572, -26.00000000000000000 ) ) ;
#45784 = CARTESIAN_POINT ( 'NONE',  ( 6.675000000000000711, -4.330127018922194537, 2.499999999999995559 ) ) ;
#45785 = CARTESIAN_POINT ( 'NONE',  ( 9.001249775931846008E-16, 16.76562500061459815, 34.90005215228797653 ) ) ;
#45786 = CARTESIAN_POINT ( 'NONE',  ( 21.30937500061451573, 0.000000000000000000, 5.243569643749999010 ) ) ;
#45787 = CYLINDRICAL_SURFACE ( 'NONE', #68591, 3.999999999999996447 ) ;
#45788 = CARTESIAN_POINT ( 'NONE',  ( 27.30000000122903359, 5.773502691896255534, 3.535250795749688894E-16 ) ) ;
#45789 = CARTESIAN_POINT ( 'NONE',  ( 17.07187500061451502, 4.119189519843966529, 2.378215178124999607 ) ) ;
#45790 = CARTESIAN_POINT ( 'NONE',  ( 23.16562500061451502, -6.054752690667223547, -1.112240025338166033E-15 ) ) ;
#45791 = CARTESIAN_POINT ( 'NONE',  ( 14.80312500061451608, 4.541064518000418104, -2.621784821874998173 ) ) ;
#45792 = CARTESIAN_POINT ( 'NONE',  ( 26.33437500061451431, -2.746126346562642428, -4.756430356249999214 ) ) ;
#45793 = CARTESIAN_POINT ( 'NONE',  ( 11.93437500061451573, -4.541064518000419881, 2.621784821874995952 ) ) ;
#45794 = CARTESIAN_POINT ( 'NONE',  ( 28.08749999999999858, 5.773502691896255534, 3.535250795749688894E-16 ) ) ;
#45795 = CARTESIAN_POINT ( 'NONE',  ( 24.37500000122903288, -5.773502691896255534, -1.060575238724906372E-15 ) ) ;
#45796 = CARTESIAN_POINT ( 'NONE',  ( 26.84999999999999787, 0.000000000000000000, 4.999999999999998224 ) ) ;
#45797 = CARTESIAN_POINT ( 'NONE',  ( 11.10937500061451644, -4.541064518000417216, -2.621784821875001281 ) ) ;
#45798 = CARTESIAN_POINT ( 'NONE',  ( 28.65937500061451715, -4.541064518000417216, -2.621784821875001281 ) ) ;
#45799 = CARTESIAN_POINT ( 'NONE',  ( 0.000000000000000000, 20.00000000000000000, 26.00000000000000000 ) ) ;
#45800 = CARTESIAN_POINT ( 'NONE',  ( 22.65937500061451715, 0.000000000000000000, 5.243569643749999010 ) ) ;
#45801 = CARTESIAN_POINT ( 'NONE',  ( 15.04687500061451644, -3.027376345333614438, 5.243569643749998122 ) ) ;
#45802 = CARTESIAN_POINT ( 'NONE',  ( 1.878215178125000495, 18.67812499938548143, 26.74683588394047007 ) ) ;
#45803 = CARTESIAN_POINT ( 'NONE',  ( 25.72499999999999787, 6.123233995736764310E-16, -4.999999999999998224 ) ) ;
#45804 = CARTESIAN_POINT ( 'NONE',  ( -1.999999999999999112, 13.10000000000000142, 26.53589838486224650 ) ) ;
#45805 = CARTESIAN_POINT ( 'NONE',  ( 28.05937500061451573, 0.000000000000000000, 4.756430356249998326 ) ) ;
#45806 = CARTESIAN_POINT ( 'NONE',  ( 18.21562500061451573, -6.054752690667223547, -1.112240025338166033E-15 ) ) ;
#45807 = CARTESIAN_POINT ( 'NONE',  ( 7.875000000000000000, 4.330127018922191873, 2.499999999999999556 ) ) ;
#45808 = CARTESIAN_POINT ( 'NONE',  ( 13.57500000122903572, -5.773502691896255534, -1.060575238724906372E-15 ) ) ;
#45809 = CARTESIAN_POINT ( 'NONE',  ( 16.57499999999999929, -4.330127018922194537, 2.499999999999995559 ) ) ;
#45810 = CARTESIAN_POINT ( 'NONE',  ( -4.243569643749997233, 12.19062500061451715, 32.45002607614398471 ) ) ;
#45811 = CARTESIAN_POINT ( 'NONE',  ( -1.626862140677534273E-15, 16.43750000000000000, 34.00000000000000000 ) ) ;
#45812 = CARTESIAN_POINT ( 'NONE',  ( 28.09687500061451360, -3.027376345333614438, 5.243569643749998122 ) ) ;
#45813 = ORIENTED_EDGE ( 'NONE', *, *, #14306, .T. ) ;
#45814 = CARTESIAN_POINT ( 'NONE',  ( 22.11562500061451786, 3.027376345333611329, 5.243569643749999010 ) ) ;
#45815 = CARTESIAN_POINT ( 'NONE',  ( 20.33437500061451786, 4.541064518000418104, 2.621784821874999949 ) ) ;
#45816 = CARTESIAN_POINT ( 'NONE',  ( 4.875000000000000888, -4.330127018922194537, 2.499999999999995559 ) ) ;
#45817 = CARTESIAN_POINT ( 'NONE',  ( 6.403125000614517504, 0.000000000000000000, 5.243569643749999010 ) ) ;
#45818 = CARTESIAN_POINT ( 'NONE',  ( 24.02812500061451573, -4.541064518000419881, 2.621784821874995952 ) ) ;
#45819 = CARTESIAN_POINT ( 'NONE',  ( 11.78437500061451892, 4.541064518000418104, 2.621784821874999949 ) ) ;
#45820 = CARTESIAN_POINT ( 'NONE',  ( 17.29687500061451999, -3.027376345333614438, 5.243569643749998122 ) ) ;
#45821 = CARTESIAN_POINT ( 'NONE',  ( 2.121784821875001281, 16.80312500061451786, 33.67503911421598417 ) ) ;
#45822 = CARTESIAN_POINT ( 'NONE',  ( 18.07500000122903216, -5.773502691896255534, -1.060575238724906372E-15 ) ) ;
#45823 = CARTESIAN_POINT ( 'NONE',  ( 15.87187500061451573, 2.746126346562643317, 4.756430356249998326 ) ) ;
#45824 = CARTESIAN_POINT ( 'NONE',  ( 10.60312500061451679, -4.541064518000417216, -2.621784821875001281 ) ) ;
#45825 = CARTESIAN_POINT ( 'NONE',  ( 5.709375000614517859, -4.541064518000417216, -2.621784821875001281 ) ) ;
#45826 = CARTESIAN_POINT ( 'NONE',  ( 4.134375000614517681, 4.541064518000418104, 2.621784821874999949 ) ) ;
#45827 = ORIENTED_EDGE ( 'NONE', *, *, #43153, .F. ) ;
#45828 = CARTESIAN_POINT ( 'NONE',  ( 24.49687500061451573, -3.027376345333614438, 5.243569643749998122 ) ) ;
#45829 = CARTESIAN_POINT ( 'NONE',  ( 17.20312500061451644, 0.000000000000000000, 5.243569643749999010 ) ) ;
#45830 = CARTESIAN_POINT ( 'NONE',  ( 26.43750000122903288, 4.330127018922191873, 2.499999999999999556 ) ) ;
#45831 = CARTESIAN_POINT ( 'NONE',  ( 28.15312500061451573, -4.541064518000417216, -2.621784821875001281 ) ) ;
#45832 = CARTESIAN_POINT ( 'NONE',  ( 22.05937500061451573, 4.541064518000418104, -2.621784821874998173 ) ) ;
#45833 = CARTESIAN_POINT ( 'NONE',  ( 17.69062500061451715, -3.027376345333614438, 5.243569643749998122 ) ) ;
#45834 = CARTESIAN_POINT ( 'NONE',  ( -2.121784821874996840, 19.48437500061451644, 33.67503911421598417 ) ) ;
#45835 = CARTESIAN_POINT ( 'NONE',  ( 21.81562500061451004, -6.054752690667223547, -1.112240025338166033E-15 ) ) ;
#45836 = CARTESIAN_POINT ( 'NONE',  ( 2.812500001229033320, -4.330127018922190985, -2.500000000000001332 ) ) ;
#45837 = ORIENTED_EDGE ( 'NONE', *, *, #43566, .T. ) ;
#45838 = CARTESIAN_POINT ( 'NONE',  ( 28.94999999999999929, 4.330127018922192761, -2.499999999999997780 ) ) ;
#45839 = CARTESIAN_POINT ( 'NONE',  ( 3.999999999999999112, 13.02500000000000213, -30.00000000000000000 ) ) ;
#45840 = CARTESIAN_POINT ( 'NONE',  ( 3.756430356250000102, 16.35312499938548569, 30.00000000000000000 ) ) ;
#45841 = ADVANCED_FACE ( 'NONE', ( #5129 ), #27663, .F. ) ;
#45842 = CARTESIAN_POINT ( 'NONE',  ( 29.57812500061451644, 6.421520780324663323E-16, -5.243569643749999010 ) ) ;
#45843 = CARTESIAN_POINT ( 'NONE',  ( 9.140625000614518214, -3.027376345333614438, 5.243569643749998122 ) ) ;
#45844 = CARTESIAN_POINT ( 'NONE',  ( 21.30000000122903359, -2.886751345948125991, -5.000000000000000000 ) ) ;
#45845 =( BOUNDED_CURVE ( )  B_SPLINE_CURVE ( 2, ( #70789, #8003, #20164, #20526, #14999, #36805, #8365 ),
 .UNSPECIFIED., .F., .F. ) 
 B_SPLINE_CURVE_WITH_KNOTS ( ( 3, 2, 2, 3 ),
 ( 0.8800000000000000044, 0.8833333333333333037, 0.8866666666666667140, 0.8900000000000000133 ),
 .UNSPECIFIED. ) 
 CURVE ( )  GEOMETRIC_REPRESENTATION_ITEM ( )  RATIONAL_B_SPLINE_CURVE ( ( 1.000000000000000000, 0.8660254037844387076, 1.000000000000000000, 0.8660254037844387076, 1.000000000000000000, 0.8660254037844387076, 1.000000000000000000 ) ) 
 REPRESENTATION_ITEM ( '' )  );
#45846 = CARTESIAN_POINT ( 'NONE',  ( 27.85312500061451502, 4.541064518000418104, -2.621784821874998173 ) ) ;
#45847 = CARTESIAN_POINT ( 'NONE',  ( 27.71250000000000568, 2.886751345948126879, 4.999999999999999112 ) ) ;
#45848 = CARTESIAN_POINT ( 'NONE',  ( -3.999999999999999112, 19.21250000122903501, -30.00000000000000000 ) ) ;
#45849 = CARTESIAN_POINT ( 'NONE',  ( 22.57499999999999929, 6.123233995736764310E-16, -4.999999999999998224 ) ) ;
#45850 = CARTESIAN_POINT ( 'NONE',  ( 10.37812500061451715, 4.541064518000418104, 2.621784821874999949 ) ) ;
#45851 = VERTEX_POINT ( 'NONE', #6940 ) ;
#45852 = CARTESIAN_POINT ( 'NONE',  ( 6.515625000614516438, -6.054752690667223547, -1.112240025338166033E-15 ) ) ;
#45853 = CARTESIAN_POINT ( 'NONE',  ( 5.915625000614515905, 3.027376345333611329, 5.243569643749999010 ) ) ;
#45854 = CARTESIAN_POINT ( 'NONE',  ( 16.84687500061451715, -2.746126346562646425, 4.756430356249996549 ) ) ;
#45855 = CARTESIAN_POINT ( 'NONE',  ( 14.71875000122903288, 2.886751345948126879, 4.999999999999998224 ) ) ;
#45856 = CARTESIAN_POINT ( 'NONE',  ( 14.81250000000000000, -5.773502691896255534, -1.060575238724906372E-15 ) ) ;
#45857 =( BOUNDED_CURVE ( )  B_SPLINE_CURVE ( 2, ( #56014, #40118, #62989, #17201, #12384 ),
 .UNSPECIFIED., .F., .F. ) 
 B_SPLINE_CURVE_WITH_KNOTS ( ( 3, 2, 3 ),
 ( 0.000000000000000000, 0.009259259259259258745, 0.01388888888888888985 ),
 .UNSPECIFIED. ) 
 CURVE ( )  GEOMETRIC_REPRESENTATION_ITEM ( )  RATIONAL_B_SPLINE_CURVE ( ( 1.000000000000000000, 0.8660254037844387076, 1.000000000000000000, 0.9330127018922192983, 0.9330127018922194093 ) ) 
 REPRESENTATION_ITEM ( '' )  );
#45858 = CARTESIAN_POINT ( 'NONE',  ( 15.30937500061451750, 4.541064518000418104, -2.621784821874998173 ) ) ;
#45859 = CARTESIAN_POINT ( 'NONE',  ( 12.37500000122903465, 2.886751345948129099, -4.999999999999998224 ) ) ;
#45860 = CARTESIAN_POINT ( 'NONE',  ( 19.50937500061451857, 0.000000000000000000, 5.243569643749999010 ) ) ;
#45861 = CARTESIAN_POINT ( 'NONE',  ( 18.37500000000000355, -4.330127018922194537, 2.499999999999995559 ) ) ;
#45862 = CARTESIAN_POINT ( 'NONE',  ( 21.08437500061451786, 6.421520780324663323E-16, -5.243569643749999010 ) ) ;
#45863 = CARTESIAN_POINT ( 'NONE',  ( 4.243569643749999010, 13.31562500061451537, -32.45002607614398471 ) ) ;
#45864 = CARTESIAN_POINT ( 'NONE',  ( 7.425000000000000711, 4.330127018922191873, 2.499999999999999556 ) ) ;
#45865 = CARTESIAN_POINT ( 'NONE',  ( 26.40937500061451360, 2.746126346562645981, -4.756430356249997438 ) ) ;
#45866 = CARTESIAN_POINT ( 'NONE',  ( -3.137519842735245283E-14, 11.56250000000000178, -26.00000000000000711 ) ) ;
#45867 = PRODUCT_DEFINITION ( 'UNKNOWN', '', #19065, #14402 ) ;
#45868 = CARTESIAN_POINT ( 'NONE',  ( 26.16562500061451502, 3.027376345333611329, 5.243569643749999010 ) ) ;
#45869 = CARTESIAN_POINT ( 'NONE',  ( 29.92968750030725644, 0.000000000000000000, 4.878215178124998275 ) ) ;
#45870 = CARTESIAN_POINT ( 'NONE',  ( 27.90937500061451715, 4.541064518000418104, -2.621784821874998173 ) ) ;
#45871 = CARTESIAN_POINT ( 'NONE',  ( 23.47499999999999787, 6.123233995736764310E-16, -4.999999999999998224 ) ) ;
#45872 = CARTESIAN_POINT ( 'NONE',  ( 5.990625000614517859, -3.027376345333614438, 5.243569643749998122 ) ) ;
#45873 = CARTESIAN_POINT ( 'NONE',  ( 25.84687500061451360, -4.119189519843965641, -2.378215178125001383 ) ) ;
#45874 =( BOUNDED_CURVE ( )  B_SPLINE_CURVE ( 2, ( #46862, #35761, #18757, #47581, #63831, #2162, #53487 ),
 .UNSPECIFIED., .F., .F. ) 
 B_SPLINE_CURVE_WITH_KNOTS ( ( 3, 2, 2, 3 ),
 ( 0.9684976324287967175, 0.9694444444444444420, 0.9722222222222222099, 0.9730832832466256299 ),
 .UNSPECIFIED. ) 
 CURVE ( )  GEOMETRIC_REPRESENTATION_ITEM ( )  RATIONAL_B_SPLINE_CURVE ( ( 0.9397993142837226532, 0.9543344473041595055, 1.000000000000000000, 0.8660254037844387076, 1.000000000000000000, 0.9584702908978937064, 0.9426875037768851495 ) ) 
 REPRESENTATION_ITEM ( '' )  );
#45875 = CARTESIAN_POINT ( 'NONE',  ( 18.87187500061451573, 3.027376345333613106, -5.243569643749998122 ) ) ;
#45876 = CARTESIAN_POINT ( 'NONE',  ( 10.24687500061451395, 4.119189519843966529, -2.378215178124998275 ) ) ;
#45877 = CARTESIAN_POINT ( 'NONE',  ( 5.878125000614517148, 4.541064518000418104, 2.621784821874999949 ) ) ;
#45878 = CARTESIAN_POINT ( 'NONE',  ( 11.93437500061451573, -4.541064518000419881, 2.621784821874995952 ) ) ;
#45879 = EDGE_LOOP ( 'NONE', ( #28342, #30753, #17161, #9324 ) ) ;
#45880 = CARTESIAN_POINT ( 'NONE',  ( 21.38437500061451502, -4.541064518000419881, 2.621784821874995952 ) ) ;
#45881 = CARTESIAN_POINT ( 'NONE',  ( 0.000000000000000000, 20.00000000000000000, -30.00000000000000000 ) ) ;
#45882 = CARTESIAN_POINT ( 'NONE',  ( 28.83749999999999858, -2.886751345948125991, -5.000000000000000000 ) ) ;
#45883 = CARTESIAN_POINT ( 'NONE',  ( 28.73437500061451644, 6.421520780324663323E-16, -5.243569643749999010 ) ) ;
#45884 = CARTESIAN_POINT ( 'NONE',  ( 26.23125000122903216, 6.123233995736764310E-16, -4.999999999999998224 ) ) ;
#45885 = CARTESIAN_POINT ( 'NONE',  ( 17.77499999999999858, 4.330127018922191873, 2.499999999999999556 ) ) ;
#45886 = ORIENTED_EDGE ( 'NONE', *, *, #67290, .T. ) ;
#45887 = CARTESIAN_POINT ( 'NONE',  ( 10.05000000000000071, 4.330127018922192761, -2.499999999999997780 ) ) ;
#45888 = CARTESIAN_POINT ( 'NONE',  ( 12.23437500061451644, -2.746126346562646425, 4.756430356249996549 ) ) ;
#45889 = CARTESIAN_POINT ( 'NONE',  ( 23.31562500061451715, 3.027376345333613106, -5.243569643749998122 ) ) ;
#45890 = CARTESIAN_POINT ( 'NONE',  ( 13.57500000000000107, 6.123233995736764310E-16, -4.999999999999998224 ) ) ;
#45891 = CARTESIAN_POINT ( 'NONE',  ( 10.57500000122903572, 2.886751345948129099, -4.999999999999998224 ) ) ;
#45892 = CARTESIAN_POINT ( 'NONE',  ( 9.778125000614517504, 6.421520780324663323E-16, -5.243569643749999010 ) ) ;
#45893 = CARTESIAN_POINT ( 'NONE',  ( 23.73749999999999716, -2.886751345948129988, 4.999999999999997335 ) ) ;
#45894 = EDGE_CURVE ( 'NONE', #38096, #7083, #20849, .T. ) ;
#45895 = CARTESIAN_POINT ( 'NONE',  ( 19.90312500061451573, 0.000000000000000000, 5.243569643749999010 ) ) ;
#45896 = FACE_OUTER_BOUND ( 'NONE', #45635, .T. ) ;
#45897 = CARTESIAN_POINT ( 'NONE',  ( 28.12500000122902932, 2.886751345948129099, -4.999999999999998224 ) ) ;
#45898 = CARTESIAN_POINT ( 'NONE',  ( 3.756430356250000102, 16.24062499938548143, 30.00000000000000000 ) ) ;
#45899 = CARTESIAN_POINT ( 'NONE',  ( 6.712500000000000355, -5.773502691896255534, -1.060575238724906372E-15 ) ) ;
#45900 = ORIENTED_EDGE ( 'NONE', *, *, #15195, .T. ) ;
#45901 = CARTESIAN_POINT ( 'NONE',  ( 21.89062500061451289, -3.027376345333610441, -5.243569643749999898 ) ) ;
#45902 = CARTESIAN_POINT ( 'NONE',  ( 29.42812500061451431, -4.541064518000419881, 2.621784821874995952 ) ) ;
#45903 = CARTESIAN_POINT ( 'NONE',  ( 18.90000000122903145, -2.886751345948197045, 4.999999999999880096 ) ) ;
#45904 = CARTESIAN_POINT ( 'NONE',  ( 18.27187500061451431, -6.054752690667223547, -1.112240025338166033E-15 ) ) ;
#45905 = CARTESIAN_POINT ( 'NONE',  ( 15.92812500061451608, -4.541064518000419881, 2.621784821874995952 ) ) ;
#45906 = CARTESIAN_POINT ( 'NONE',  ( -2.121784821874999949, 10.27812500061459566, -33.67503911421598417 ) ) ;
#45907 = CARTESIAN_POINT ( 'NONE',  ( 27.45000000122903572, -2.886751345948129988, 4.999999999999997335 ) ) ;
#45908 = CARTESIAN_POINT ( 'NONE',  ( 23.07187500061452212, 2.746126346562643317, 4.756430356249998326 ) ) ;
#45909 = CARTESIAN_POINT ( 'NONE',  ( 16.45312500061451289, -4.541064518000417216, -2.621784821875001281 ) ) ;
#45910 = CARTESIAN_POINT ( 'NONE',  ( 50.00000000000000000, 5.218601775200110815, -7.332543590861103411 ) ) ;
#45911 = CARTESIAN_POINT ( 'NONE',  ( 4.012500001229033053, 0.000000000000000000, 4.999999999999998224 ) ) ;
#45912 = CARTESIAN_POINT ( 'NONE',  ( 13.84687500061451537, -3.027376345333610441, -5.243569643749999898 ) ) ;
#45913 = CARTESIAN_POINT ( 'NONE',  ( 12.19687500061451679, 6.054752690667223547, 3.707466751127219781E-16 ) ) ;
#45914 = CARTESIAN_POINT ( 'NONE',  ( 19.50937500061451857, 0.000000000000000000, 5.243569643749999010 ) ) ;
#45915 = ORIENTED_EDGE ( 'NONE', *, *, #10750, .F. ) ;
#45916 = CARTESIAN_POINT ( 'NONE',  ( -6.000139530219997575, 7.999895352344702282, 30.40432978294467858 ) ) ;
#45917 = CARTESIAN_POINT ( 'NONE',  ( 24.47812500061451502, -4.541064518000419881, 2.621784821874995952 ) ) ;
#45918 = CARTESIAN_POINT ( 'NONE',  ( 17.82187500061451502, -6.054752690667223547, -1.112240025338166033E-15 ) ) ;
#45919 = CARTESIAN_POINT ( 'NONE',  ( 25.41562500061451146, -6.054752690667223547, -1.112240025338166033E-15 ) ) ;
#45920 = CARTESIAN_POINT ( 'NONE',  ( 30.00000000000000000, 0.000000000000000000, 4.999999999999998224 ) ) ;
#45921 = CARTESIAN_POINT ( 'NONE',  ( 4.000000000000000000, 15.68750000000000000, 32.30940107675849049 ) ) ;
#45922 = CARTESIAN_POINT ( 'NONE',  ( 28.52812500061451573, -4.541064518000419881, 2.621784821874995952 ) ) ;
#45923 = CARTESIAN_POINT ( 'NONE',  ( 9.862500001229033586, 0.000000000000000000, 4.999999999999998224 ) ) ;
#45924 = CARTESIAN_POINT ( 'NONE',  ( 6.675000001229034474, 2.886751345948126879, 4.999999999999999112 ) ) ;
#45925 = CARTESIAN_POINT ( 'NONE',  ( 28.95000000122903927, -2.886751345948095793, -5.000000000000054179 ) ) ;
#45926 = CARTESIAN_POINT ( 'NONE',  ( 27.03750000122903430, -4.330127018922194537, 2.499999999999995559 ) ) ;
#45927 = CARTESIAN_POINT ( 'NONE',  ( -4.000000000000000000, 19.41874999877096641, 30.00000000000000000 ) ) ;
#45928 = CARTESIAN_POINT ( 'NONE',  ( 17.38125000122903074, 4.330127018922191873, 2.499999999999999556 ) ) ;
#45929 = EDGE_CURVE ( 'NONE', #66635, #12333, #46466, .T. ) ;
#45930 = CARTESIAN_POINT ( 'NONE',  ( 9.646875000614516082, -3.027376345333614438, 5.243569643749998122 ) ) ;
#45931 = FACE_OUTER_BOUND ( 'NONE', #44125, .T. ) ;
#45932 = CARTESIAN_POINT ( 'NONE',  ( 16.79062500061451857, -3.027376345333614438, 5.243569643749998122 ) ) ;
#45933 = CARTESIAN_POINT ( 'NONE',  ( 11.89687500061451608, -3.027376345333614438, 5.243569643749998122 ) ) ;
#45934 = CARTESIAN_POINT ( 'NONE',  ( 3.290625000614516793, -3.027376345333614438, 5.243569643749998122 ) ) ;
#45935 = CARTESIAN_POINT ( 'NONE',  ( 19.50937500061451857, 0.000000000000000000, 5.243569643749999010 ) ) ;
#45936 = CARTESIAN_POINT ( 'NONE',  ( 6.721875000614518925, 3.027376345333613106, -5.243569643749998122 ) ) ;
#45937 = CARTESIAN_POINT ( 'NONE',  ( 3.365625000614516082, -6.054752690667223547, -1.112240025338166033E-15 ) ) ;
#45938 = CARTESIAN_POINT ( 'NONE',  ( -3.999999999999997335, 17.78750000000000142, 32.30940107675850470 ) ) ;
#45939 = CARTESIAN_POINT ( 'NONE',  ( 8.653125000614515727, 0.000000000000000000, 5.243569643749999010 ) ) ;
#45940 = CARTESIAN_POINT ( 'NONE',  ( 19.26562500061451644, 3.027376345333613106, -5.243569643749998122 ) ) ;
#45941 = ORIENTED_EDGE ( 'NONE', *, *, #3480, .T. ) ;
#45942 = CARTESIAN_POINT ( 'NONE',  ( 4.800000001229032698, 5.773502691896255534, 3.535250795749688894E-16 ) ) ;
#45943 = CARTESIAN_POINT ( 'NONE',  ( 14.27812500061451573, 6.421520780324663323E-16, -5.243569643749999010 ) ) ;
#45944 = CARTESIAN_POINT ( 'NONE',  ( 13.52812500061451750, 4.541064518000418104, 2.621784821874999949 ) ) ;
#45945 = CARTESIAN_POINT ( 'NONE',  ( 23.78437500061451360, 5.824947211148865298E-16, -4.756430356249998326 ) ) ;
#45946 = CARTESIAN_POINT ( 'NONE',  ( 13.83749999999999858, -2.886751345948129988, 4.999999999999997335 ) ) ;
#45947 = CARTESIAN_POINT ( 'NONE',  ( 8.137500001229033941, -4.330127018922194537, 2.499999999999995559 ) ) ;
#45948 = ADVANCED_FACE ( 'NONE', ( #23917 ), #70452, .F. ) ;
#45949 = CARTESIAN_POINT ( 'NONE',  ( 5.990625000614517859, -3.027376345333614438, 5.243569643749998122 ) ) ;
#45950 = CARTESIAN_POINT ( 'NONE',  ( 19.46250000122903145, -4.330127018922190985, -2.500000000000001332 ) ) ;
#45951 = CARTESIAN_POINT ( 'NONE',  ( 24.82499999999999929, 6.123233995736764310E-16, -4.999999999999998224 ) ) ;
#45952 = CARTESIAN_POINT ( 'NONE',  ( -4.243569643749999898, 11.75937500061451857, -30.00000000000000000 ) ) ;
#45953 = CARTESIAN_POINT ( 'NONE',  ( 3.712500001229034563, -4.330127018922190985, -2.500000000000001332 ) ) ;
#45954 = CARTESIAN_POINT ( 'NONE',  ( 3.242103837493086330E-14, 11.33750000000000213, -34.00000000000000000 ) ) ;
#45955 = CARTESIAN_POINT ( 'NONE',  ( 30.00000000000000000, 0.000000000000000000, 0.000000000000000000 ) ) ;
#45956 = CARTESIAN_POINT ( 'NONE',  ( 19.02187500061451786, 3.027376345333611329, 5.243569643749999010 ) ) ;
#45957 = CARTESIAN_POINT ( 'NONE',  ( 10.61250000122903536, 4.330127018922192761, -2.499999999999997780 ) ) ;
#45958 = CARTESIAN_POINT ( 'NONE',  ( 13.52812500061451750, 4.541064518000418104, 2.621784821874999949 ) ) ;
#45959 = CARTESIAN_POINT ( 'NONE',  ( 9.731250001229033941, 4.330127018922191873, 2.499999999999999556 ) ) ;
#45960 = FACE_OUTER_BOUND ( 'NONE', #51241, .T. ) ;
#45961 = CARTESIAN_POINT ( 'NONE',  ( 29.18437500061451573, 6.421520780324663323E-16, -5.243569643749999010 ) ) ;
#45962 = CARTESIAN_POINT ( 'NONE',  ( 27.19687500061451857, -3.027376345333614438, 5.243569643749998122 ) ) ;
#45963 = CARTESIAN_POINT ( 'NONE',  ( 18.34687500061451360, 4.119189519843966529, -2.378215178124998275 ) ) ;
#45964 = CARTESIAN_POINT ( 'NONE',  ( 13.07812500061451821, 4.541064518000418104, 2.621784821874999949 ) ) ;
#45965 = CARTESIAN_POINT ( 'NONE',  ( 10.65937500061451715, -4.541064518000417216, -2.621784821875001281 ) ) ;
#45966 = VERTEX_POINT ( 'NONE', #8026 ) ;
#45967 = CARTESIAN_POINT ( 'NONE',  ( 29.54062500061451502, -3.027376345333610441, -5.243569643749999898 ) ) ;
#45968 = CARTESIAN_POINT ( 'NONE',  ( 21.36562500061451431, -6.054752690667223547, -1.112240025338166033E-15 ) ) ;
#45969 = CARTESIAN_POINT ( 'NONE',  ( 3.120664071082557278, 3.906599426175572543, -3.497650499216746312 ) ) ;
#45970 = CARTESIAN_POINT ( 'NONE',  ( 3.999999999999998668, 14.86250000000000071, 27.69059892324149530 ) ) ;
#45971 = CARTESIAN_POINT ( 'NONE',  ( 10.27499999999999858, -4.330127018922194537, 2.499999999999995559 ) ) ;
#45972 = CARTESIAN_POINT ( 'NONE',  ( 21.48750000122903003, 4.330127018922191873, 2.499999999999999556 ) ) ;
#45973 = CARTESIAN_POINT ( 'NONE',  ( 14.99062500061451786, -3.027376345333614438, 5.243569643749998122 ) ) ;
#45974 = CARTESIAN_POINT ( 'NONE',  ( 10.50937500061451502, -5.492252693125287522, -1.008910452111647106E-15 ) ) ;
#45975 = EDGE_LOOP ( 'NONE', ( #46342, #47182, #42154, #35242 ) ) ;
#45976 = CARTESIAN_POINT ( 'NONE',  ( 17.69999999999999929, 4.330127018922192761, -2.499999999999997780 ) ) ;
#45977 = CARTESIAN_POINT ( 'NONE',  ( 20.88749999999999929, 5.773502691896255534, 3.535250795749688894E-16 ) ) ;
#45978 = CARTESIAN_POINT ( 'NONE',  ( 19.92187500061451644, 3.027376345333611329, 5.243569643749999010 ) ) ;
#45979 = CARTESIAN_POINT ( 'NONE',  ( 26.24062500061451431, -3.027376345333614438, 5.243569643749998122 ) ) ;
#45980 = ORIENTED_EDGE ( 'NONE', *, *, #30976, .F. ) ;
#45981 = CARTESIAN_POINT ( 'NONE',  ( 19.76249999999999929, -5.773502691896255534, -1.060575238724906372E-15 ) ) ;
#45982 = CARTESIAN_POINT ( 'NONE',  ( 8.465625000614515727, 3.027376345333613106, -5.243569643749998122 ) ) ;
#45983 = CARTESIAN_POINT ( 'NONE',  ( -1.071796769724480347, 19.06115380933863435, 34.00000000000000711 ) ) ;
#45984 = CARTESIAN_POINT ( 'NONE',  ( 15.67500000000000071, -4.330127018922194537, 2.499999999999995559 ) ) ;
#45985 = CARTESIAN_POINT ( 'NONE',  ( 2.121784821875001281, 18.15312500061451928, 33.67503911421598417 ) ) ;
#45986 = CARTESIAN_POINT ( 'NONE',  ( 29.09062500061451573, -3.027376345333610441, -5.243569643749999898 ) ) ;
#45987 = CARTESIAN_POINT ( 'NONE',  ( -7.967954043666661671E-16, 14.32812499938548179, 34.33755215474603517 ) ) ;
#45988 = CARTESIAN_POINT ( 'NONE',  ( 26.03437500061451715, 6.421520780324663323E-16, -5.243569643749999010 ) ) ;
#45989 = EDGE_LOOP ( 'NONE', ( #60859, #15244, #69228, #55207 ) ) ;
#45990 = CARTESIAN_POINT ( 'NONE',  ( 23.80312500061451786, 4.541064518000418104, -2.621784821874998173 ) ) ;
#45991 = CARTESIAN_POINT ( 'NONE',  ( 24.64687500061451431, -3.027376345333610441, -5.243569643749999898 ) ) ;
#45992 = CARTESIAN_POINT ( 'NONE',  ( 4.243569643749999898, 18.22812500061459318, -30.00000000000000000 ) ) ;
#45993 = CARTESIAN_POINT ( 'NONE',  ( 10.83750000000000036, -2.886751345948125991, -5.000000000000000000 ) ) ;
#45994 = CARTESIAN_POINT ( 'NONE',  ( 9.328125000614518214, 6.421520780324663323E-16, -5.243569643749999010 ) ) ;
#45995 = CARTESIAN_POINT ( 'NONE',  ( 3.836658989281606313, 3.881372312241275768, 3.277265952107013547 ) ) ;
#45996 = CARTESIAN_POINT ( 'NONE',  ( 29.50312500061451360, -4.541064518000417216, -2.621784821875001281 ) ) ;
#45997 = CARTESIAN_POINT ( 'NONE',  ( 27.17812500061451786, -4.541064518000419881, 2.621784821874995952 ) ) ;
#45998 = CARTESIAN_POINT ( 'NONE',  ( 28.24687500061451217, 4.119189519843966529, -2.378215178124998275 ) ) ;
#45999 = CARTESIAN_POINT ( 'NONE',  ( 12.87187500061451750, -5.492252693125287522, -1.008910452111647106E-15 ) ) ;
#46000 = CARTESIAN_POINT ( 'NONE',  ( 20.18437500061451573, 6.421520780324663323E-16, -5.243569643749999010 ) ) ;
#46001 = CARTESIAN_POINT ( 'NONE',  ( 4.243569643749999010, 12.92187500061451644, 27.54997392385601174 ) ) ;
#46002 = ADVANCED_FACE ( 'NONE', ( #19828 ), #57539, .T. ) ;
#46003 = CARTESIAN_POINT ( 'NONE',  ( 18.42187500061451644, 3.027376345333613106, -5.243569643749998122 ) ) ;
#46004 = CARTESIAN_POINT ( 'NONE',  ( 26.74687500061451573, -3.027376345333614438, 5.243569643749998122 ) ) ;
#46005 = CARTESIAN_POINT ( 'NONE',  ( -3.000416591977282496E-16, 16.14687500061451786, 25.09994784771203058 ) ) ;
#46006 = CARTESIAN_POINT ( 'NONE',  ( 8.165625000614516793, 3.027376345333611329, 5.243569643749999010 ) ) ;
#46007 = CARTESIAN_POINT ( 'NONE',  ( 3.999999999999999112, 10.43750000122903465, -30.00000000000000000 ) ) ;
#46008 = CARTESIAN_POINT ( 'NONE',  ( 3.571875000614517237, 3.027376345333613106, -5.243569643749998122 ) ) ;
#46009 = CARTESIAN_POINT ( 'NONE',  ( -2.672702088255949472E-15, 13.51250000000000107, 26.00000000000000000 ) ) ;
#46010 = CARTESIAN_POINT ( 'NONE',  ( 4.978125000614518569, 4.541064518000418104, 2.621784821874999949 ) ) ;
#46011 = CARTESIAN_POINT ( 'NONE',  ( 9.984375000614518214, 4.541064518000418104, 2.621784821874999949 ) ) ;
#46012 = DIRECTION ( 'NONE',  ( 1.000000000000000000, 0.000000000000000000, 0.000000000000000000 ) ) ;
#46013 = CARTESIAN_POINT ( 'NONE',  ( 18.03750000122903430, -4.330127018922194537, 2.499999999999995559 ) ) ;
#46014 = CARTESIAN_POINT ( 'NONE',  ( 6.046875000614519102, -3.027376345333614438, 5.243569643749998122 ) ) ;
#46015 = CARTESIAN_POINT ( 'NONE',  ( 7.490625000614516082, -3.027376345333610441, -5.243569643749999898 ) ) ;
#46016 = CARTESIAN_POINT ( 'NONE',  ( 5.728125000614515905, 6.421520780324663323E-16, -5.243569643749999010 ) ) ;
#46017 = CARTESIAN_POINT ( 'NONE',  ( 24.24375000122903145, -2.886751345948129988, 4.999999999999997335 ) ) ;
#46018 = CARTESIAN_POINT ( 'NONE',  ( 17.48437500061451999, 6.421520780324663323E-16, -5.243569643749999010 ) ) ;
#46019 = DIRECTION ( 'NONE',  ( -0.000000000000000000, -1.000000000000000000, -0.000000000000000000 ) ) ;
#46020 = VERTEX_POINT ( 'NONE', #36466 ) ;
#46021 = CARTESIAN_POINT ( 'NONE',  ( 23.95312500061451289, 0.000000000000000000, 5.243569643749999010 ) ) ;
#46022 = CARTESIAN_POINT ( 'NONE',  ( 10.67812500061451608, 6.421520780324663323E-16, -5.243569643749999010 ) ) ;
#46023 = CARTESIAN_POINT ( 'NONE',  ( 27.72187500061451715, -6.054752690667223547, -1.112240025338166033E-15 ) ) ;
#46024 = CARTESIAN_POINT ( 'NONE',  ( 10.37812500061451715, 4.541064518000418104, 2.621784821874999949 ) ) ;
#46025 = CARTESIAN_POINT ( 'NONE',  ( 4.400918202330496243, -2.373166445152071535, -4.675799785326651303 ) ) ;
#46026 =( BOUNDED_CURVE ( )  B_SPLINE_CURVE ( 2, ( #69038, #69755, #68677, #29506, #1446, #42048, #59018 ),
 .UNSPECIFIED., .F., .F. ) 
 B_SPLINE_CURVE_WITH_KNOTS ( ( 3, 2, 2, 3 ),
 ( 0.8916666666666667185, 0.8944444444444444864, 0.8972222222222223653, 0.9000000000000001332 ),
 .UNSPECIFIED. ) 
 CURVE ( )  GEOMETRIC_REPRESENTATION_ITEM ( )  RATIONAL_B_SPLINE_CURVE ( ( 1.000000000000000000, 0.8660254037844387076, 1.000000000000000000, 0.8660254037844387076, 1.000000000000000000, 0.8660254037844333785, 1.000000000000005329 ) ) 
 REPRESENTATION_ITEM ( '' )  );
#46027 = CARTESIAN_POINT ( 'NONE',  ( 13.87500000122903465, 2.886751345948126879, 4.999999999999999112 ) ) ;
#46028 = CARTESIAN_POINT ( 'NONE',  ( 28.04062500061451502, -3.027376345333614438, 5.243569643749998122 ) ) ;
#46029 = CARTESIAN_POINT ( 'NONE',  ( 4.243569643749999898, 11.89062500061451644, -27.54997392385601529 ) ) ;
#46030 = CARTESIAN_POINT ( 'NONE',  ( 12.78750000122903430, 6.123233995736764310E-16, -4.999999999999998224 ) ) ;
#46031 = CARTESIAN_POINT ( 'NONE',  ( 11.84999999999999964, 4.330127018922192761, -2.499999999999997780 ) ) ;
#46032 = CARTESIAN_POINT ( 'NONE',  ( 21.25312500061451715, 0.000000000000000000, 5.243569643749999010 ) ) ;
#46033 = CARTESIAN_POINT ( 'NONE',  ( 5.671875000614519102, -6.054752690667223547, -1.112240025338166033E-15 ) ) ;
#46034 = CARTESIAN_POINT ( 'NONE',  ( 19.53749999999999432, 5.773502691896255534, 3.535250795749688894E-16 ) ) ;
#46035 = CARTESIAN_POINT ( 'NONE',  ( 8.250000001229034652, -2.886751345948125991, -5.000000000000000000 ) ) ;
#46036 = CARTESIAN_POINT ( 'NONE',  ( 16.65000000122903501, -2.886751345948129988, 4.999999999999997335 ) ) ;
#46037 = CARTESIAN_POINT ( 'NONE',  ( 13.26562500061451644, -6.054752690667223547, -1.112240025338166033E-15 ) ) ;
#46038 = CARTESIAN_POINT ( 'NONE',  ( 16.75312500061451715, 0.000000000000000000, 5.243569643749999010 ) ) ;
#46039 = CARTESIAN_POINT ( 'NONE',  ( 24.97500000122903430, 2.886751345948129099, -4.999999999999998224 ) ) ;
#46040 = CARTESIAN_POINT ( 'NONE',  ( 20.88749999999999929, 5.773502691896255534, 3.535250795749688894E-16 ) ) ;
#46041 = CARTESIAN_POINT ( 'NONE',  ( 23.93437500061451573, 4.541064518000418104, 2.621784821874999949 ) ) ;
#46042 = CARTESIAN_POINT ( 'NONE',  ( -4.999999999999998224, 2.928932188134522718, -4.999999999999998224 ) ) ;
#46043 = ADVANCED_FACE ( 'NONE', ( #1770 ), #19454, .F. ) ;
#46044 = CARTESIAN_POINT ( 'NONE',  ( 10.05000000122903181, -2.886751345948125991, -5.000000000000000000 ) ) ;
#46045 = CARTESIAN_POINT ( 'NONE',  ( 8.634375000614518569, 4.541064518000418104, 2.621784821874999949 ) ) ;
#46046 = CARTESIAN_POINT ( 'NONE',  ( 26.70937500061451431, 0.000000000000000000, 5.243569643749999010 ) ) ;
#46047 = CYLINDRICAL_SURFACE ( 'NONE', #5602, 4.999999999999998224 ) ;
#46048 = CARTESIAN_POINT ( 'NONE',  ( 23.46562500061451573, 3.027376345333611329, 5.243569643749999010 ) ) ;
#46049 = CARTESIAN_POINT ( 'NONE',  ( 26.18437500061451573, 4.541064518000418104, 2.621784821874999949 ) ) ;
#46050 = CARTESIAN_POINT ( 'NONE',  ( -3.756430356250000990, 17.96562499938548285, 32.16877607737301048 ) ) ;
#46051 = CARTESIAN_POINT ( 'NONE',  ( 3.310802318797580579, -3.746810377620464205, 3.668301323911666412 ) ) ;
#46052 = CARTESIAN_POINT ( 'NONE',  ( 8.521875000614516082, 3.027376345333613106, -5.243569643749998122 ) ) ;
#46053 = CARTESIAN_POINT ( 'NONE',  ( 18.85312500061451502, 4.541064518000418104, -2.621784821874998173 ) ) ;
#46054 = CARTESIAN_POINT ( 'NONE',  ( 30.00000000000000000, 6.123233995736764310E-16, -4.999999999999998224 ) ) ;
#46055 = CARTESIAN_POINT ( 'NONE',  ( 28.19062500061451715, -3.027376345333610441, -5.243569643749999898 ) ) ;
#46056 = CARTESIAN_POINT ( 'NONE',  ( 4.921875000614518214, 3.027376345333613106, -5.243569643749998122 ) ) ;
#46057 = CARTESIAN_POINT ( 'NONE',  ( 29.55000000000000071, 0.000000000000000000, 4.999999999999998224 ) ) ;
#46058 = CARTESIAN_POINT ( 'NONE',  ( 4.003125000614518925, 4.541064518000418104, -2.621784821874998173 ) ) ;
#46059 = CARTESIAN_POINT ( 'NONE',  ( 18.00000000000000355, -4.330127018922190985, -2.500000000000001332 ) ) ;
#46060 = EDGE_LOOP ( 'NONE', ( #66264, #4549, #14599, #7048 ) ) ;
#46061 = CARTESIAN_POINT ( 'NONE',  ( 27.75000000000000000, 0.000000000000000000, 4.999999999999998224 ) ) ;
#46062 =( BOUNDED_CURVE ( )  B_SPLINE_CURVE ( 3, ( #4735, #72327, #54973, #286 ),
 .UNSPECIFIED., .F., .F. ) 
 B_SPLINE_CURVE_WITH_KNOTS ( ( 4, 4 ),
 ( 5.396747428351075015, 5.426701883967095519 ),
 .UNSPECIFIED. ) 
 CURVE ( )  GEOMETRIC_REPRESENTATION_ITEM ( )  RATIONAL_B_SPLINE_CURVE ( ( 1.000000000000000000, 0.9999252289467817079, 0.9999252289467817079, 1.000000000000000000 ) ) 
 REPRESENTATION_ITEM ( '' )  );
#46063 = CARTESIAN_POINT ( 'NONE',  ( 27.00937500061451857, 4.541064518000418104, -2.621784821874998173 ) ) ;
#46064 = ORIENTED_EDGE ( 'NONE', *, *, #26971, .T. ) ;
#46065 = CARTESIAN_POINT ( 'NONE',  ( 15.25312500061451715, 4.541064518000418104, -2.621784821874998173 ) ) ;
#46066 = CARTESIAN_POINT ( 'NONE',  ( 7.040625000614517681, -3.027376345333610441, -5.243569643749999898 ) ) ;
#46067 = CARTESIAN_POINT ( 'NONE',  ( 19.84687500061451360, 0.000000000000000000, 4.756430356249998326 ) ) ;
#46068 = CARTESIAN_POINT ( 'NONE',  ( 4.584375000614516971, 4.541064518000418104, 2.621784821874999949 ) ) ;
#46069 = CARTESIAN_POINT ( 'NONE',  ( 16.50000000122903288, 5.773502691896255534, 3.535250795749688894E-16 ) ) ;
#46070 = CARTESIAN_POINT ( 'NONE',  ( 21.22500000000000142, 6.123233995736764310E-16, -4.999999999999998224 ) ) ;
#46071 = CARTESIAN_POINT ( 'NONE',  ( 29.77499999999999858, 6.123233995736764310E-16, -4.999999999999998224 ) ) ;
#46072 = CARTESIAN_POINT ( 'NONE',  ( 4.059375000614519280, 4.541064518000418104, -2.621784821874998173 ) ) ;
#46073 = CARTESIAN_POINT ( 'NONE',  ( 10.47187500061451715, 3.027376345333611329, 5.243569643749999010 ) ) ;
#46074 = CARTESIAN_POINT ( 'NONE',  ( 21.83437500061451786, -4.541064518000419881, 2.621784821874995952 ) ) ;
#46075 = CARTESIAN_POINT ( 'NONE',  ( 1.626862140677534273E-15, 15.27500000122903501, -26.00000000000000355 ) ) ;
#46076 = VERTEX_POINT ( 'NONE', #24645 ) ;
#46077 = CARTESIAN_POINT ( 'NONE',  ( 5.221875000614519813, -6.054752690667223547, -1.112240025338166033E-15 ) ) ;
#46078 = CARTESIAN_POINT ( 'NONE',  ( 5.887500000000000178, -2.886751345948125991, -5.000000000000000000 ) ) ;
#46079 = CARTESIAN_POINT ( 'NONE',  ( 6.271875000614517859, 3.027376345333613106, -5.243569643749998122 ) ) ;
#46080 = CARTESIAN_POINT ( 'NONE',  ( 18.07499999999999929, 6.123233995736764310E-16, -4.999999999999998224 ) ) ;
#46081 = CARTESIAN_POINT ( 'NONE',  ( 16.41562500061451857, -6.054752690667223547, -1.112240025338166033E-15 ) ) ;
#46082 = CARTESIAN_POINT ( 'NONE',  ( 3.999999999999998668, 20.11249999999999716, 32.30940107675850470 ) ) ;
#46083 = CARTESIAN_POINT ( 'NONE',  ( 4.231215331025275361, 2.664084549475962405, 4.393375741670284107 ) ) ;
#46084 = CARTESIAN_POINT ( 'NONE',  ( 20.55937500061451573, -4.119189519843965641, -2.378215178125001383 ) ) ;
#46085 = CARTESIAN_POINT ( 'NONE',  ( 10.79062500061451679, 6.054752690667223547, 3.707466751127219781E-16 ) ) ;
#46086 = CARTESIAN_POINT ( 'NONE',  ( 27.19687500061451857, -3.027376345333614438, 5.243569643749998122 ) ) ;
#46087 = CARTESIAN_POINT ( 'NONE',  ( 4.243569643749999898, 19.14687500061451431, 32.45002607614398471 ) ) ;
#46088 = CARTESIAN_POINT ( 'NONE',  ( 26.03437500061451715, 6.421520780324663323E-16, -5.243569643749999010 ) ) ;
#46089 = CARTESIAN_POINT ( 'NONE',  ( 7.687500000000000000, -2.886751345948125991, -5.000000000000000000 ) ) ;
#46090 = CARTESIAN_POINT ( 'NONE',  ( 1.999999999999998668, 14.11250000122903359, 26.53589838486224650 ) ) ;
#46091 = CARTESIAN_POINT ( 'NONE',  ( 15.44062500061451537, -3.027376345333614438, 5.243569643749998122 ) ) ;
#46092 = CARTESIAN_POINT ( 'NONE',  ( 6.937500001229033764, 6.123233995736764310E-16, -4.999999999999998224 ) ) ;
#46093 = CARTESIAN_POINT ( 'NONE',  ( 16.73437500061451644, 4.541064518000418104, 2.621784821874999949 ) ) ;
#46094 = CARTESIAN_POINT ( 'NONE',  ( 12.04687500061451821, -3.027376345333610441, -5.243569643749999898 ) ) ;
#46095 = CARTESIAN_POINT ( 'NONE',  ( 10.00000000000000000, 1.224646799147353256E-15, 10.00000000000000178 ) ) ;
#46096 = ORIENTED_EDGE ( 'NONE', *, *, #37581, .F. ) ;
#46097 = CARTESIAN_POINT ( 'NONE',  ( 14.05312500061451431, 0.000000000000000000, 5.243569643749999010 ) ) ;
#46098 = CARTESIAN_POINT ( 'NONE',  ( 25.42500000122903359, 2.886751345948129099, -4.999999999999998224 ) ) ;
#46099 = CARTESIAN_POINT ( 'NONE',  ( 13.54687500061451999, 6.054752690667223547, 3.707466751127219781E-16 ) ) ;
#46100 = CARTESIAN_POINT ( 'NONE',  ( 14.76562500061451821, 3.027376345333613106, -5.243569643749998122 ) ) ;
#46101 = CARTESIAN_POINT ( 'NONE',  ( 20.86875000122903145, 2.886751345948129099, -4.999999999999997335 ) ) ;
#46102 = CARTESIAN_POINT ( 'NONE',  ( 23.63437500061451502, -4.541064518000419881, 2.621784821874995952 ) ) ;
#46103 = CARTESIAN_POINT ( 'NONE',  ( 4.243569643749999010, 10.61562500061451786, 27.54997392385601174 ) ) ;
#46104 = CARTESIAN_POINT ( 'NONE',  ( 10.72500000122903252, 2.886751345948126879, 4.999999999999999112 ) ) ;
#46105 = CARTESIAN_POINT ( 'NONE',  ( 0.000000000000000000, 20.00000000000000000, 26.00000000000000000 ) ) ;
#46106 = CARTESIAN_POINT ( 'NONE',  ( 22.78125000122903288, 4.330127018922191873, 2.499999999999999556 ) ) ;
#46107 = CARTESIAN_POINT ( 'NONE',  ( -4.243569643749999898, 16.25937500061451857, -30.00000000000000000 ) ) ;
#46108 = CARTESIAN_POINT ( 'NONE',  ( 17.25937500061451502, 0.000000000000000000, 5.243569643749999010 ) ) ;
#46109 = CARTESIAN_POINT ( 'NONE',  ( 20.77500000122903145, -5.773502691896255534, -1.060575238724906372E-15 ) ) ;
#46110 = CARTESIAN_POINT ( 'NONE',  ( 14.37187500061451928, 3.027376345333613106, -5.243569643749998122 ) ) ;
#46111 = CARTESIAN_POINT ( 'NONE',  ( 4.243569643749999010, 10.22187500061451892, 27.54997392385601174 ) ) ;
#46112 = CARTESIAN_POINT ( 'NONE',  ( 20.85000000122903430, -2.886751345948125991, -5.000000000000000000 ) ) ;
#46113 = CARTESIAN_POINT ( 'NONE',  ( 16.07812500061451289, 6.421520780324663323E-16, -5.243569643749999010 ) ) ;
#46114 = CARTESIAN_POINT ( 'NONE',  ( 1.626862140677534273E-15, 12.46250000000000213, 34.00000000000000000 ) ) ;
#46115 = ORIENTED_EDGE ( 'NONE', *, *, #52383, .T. ) ;
#46116 = ORIENTED_EDGE ( 'NONE', *, *, #3889, .T. ) ;
#46117 = CARTESIAN_POINT ( 'NONE',  ( 17.92500000000000071, -4.330127018922194537, 2.499999999999995559 ) ) ;
#46118 = CARTESIAN_POINT ( 'NONE',  ( 1.071796769724485232, 15.68615380933863257, 25.99999999999999645 ) ) ;
#46119 = CARTESIAN_POINT ( 'NONE',  ( 3.964577175323932057, 3.046748717458611644, 30.54880584332639160 ) ) ;
#46120 = CARTESIAN_POINT ( 'NONE',  ( 15.37500000122903465, -5.773502691896255534, -1.060575238724906372E-15 ) ) ;
#46121 = CARTESIAN_POINT ( 'NONE',  ( 27.53437500061451360, 4.541064518000418104, 2.621784821874999949 ) ) ;
#46122 = CARTESIAN_POINT ( 'NONE',  ( 19.67812500061451786, 6.421520780324663323E-16, -5.243569643749999010 ) ) ;
#46123 = CARTESIAN_POINT ( 'NONE',  ( 23.27812500061451573, 6.421520780324663323E-16, -5.243569643749999010 ) ) ;
#46124 = CARTESIAN_POINT ( 'NONE',  ( 29.62500000122903288, 2.886751345948126879, 4.999999999999999112 ) ) ;
#46125 = CARTESIAN_POINT ( 'NONE',  ( 27.86249999999999716, -5.773502691896255534, -1.060575238724906372E-15 ) ) ;
#46126 = CARTESIAN_POINT ( 'NONE',  ( 3.999999999999999112, 11.78750000122903430, 30.00000000000000000 ) ) ;
#46127 = CARTESIAN_POINT ( 'NONE',  ( 8.596875000614518925, 5.492252693125287522, 3.363034840372157021E-16 ) ) ;
#46128 = LINE ( 'NONE', #1799, #33544 ) ;
#46129 = CARTESIAN_POINT ( 'NONE',  ( 23.25000000000000000, 0.000000000000000000, 4.999999999999998224 ) ) ;
#46130 = CARTESIAN_POINT ( 'NONE',  ( -2.121784821874996840, 16.33437500061451786, -26.32496088578401583 ) ) ;
#46131 = CARTESIAN_POINT ( 'NONE',  ( 5.062500001229035540, -4.330127018922190985, -2.500000000000001332 ) ) ;
#46132 = CARTESIAN_POINT ( 'NONE',  ( 4.949999999999999289, -4.330127018922190985, -2.500000000000001332 ) ) ;
#46133 = EDGE_CURVE ( 'NONE', #50673, #32393, #29831, .T. ) ;
#46134 = CARTESIAN_POINT ( 'NONE',  ( 3.300000001229034918, -2.886751345948125991, -5.000000000000000000 ) ) ;
#46135 = CARTESIAN_POINT ( 'NONE',  ( 9.046875000614518214, 6.054752690667223547, 3.707466751127219781E-16 ) ) ;
#46136 = CYLINDRICAL_SURFACE ( 'NONE', #48953, 4.999999999999998224 ) ;
#46137 = CARTESIAN_POINT ( 'NONE',  ( 15.65625000122903465, 0.000000000000000000, 4.999999999999998224 ) ) ;
#46138 = CARTESIAN_POINT ( 'NONE',  ( -5.193763058582908876, 8.549021686977599899, -33.02854916113439998 ) ) ;
#46139 = DIRECTION ( 'NONE',  ( 0.000000000000000000, 0.000000000000000000, 1.000000000000000000 ) ) ;
#46140 = CARTESIAN_POINT ( 'NONE',  ( 6.571875000614517681, -6.054752690667223547, -1.112240025338166033E-15 ) ) ;
#46141 = CARTESIAN_POINT ( 'NONE',  ( 13.84687500061451537, -3.027376345333610441, -5.243569643749999898 ) ) ;
#46142 = CARTESIAN_POINT ( 'NONE',  ( 5.549999999999998934, 4.330127018922192761, -2.499999999999997780 ) ) ;
#46143 = CARTESIAN_POINT ( 'NONE',  ( 4.243569643749999898, 17.74062500061459602, 32.45002607614398471 ) ) ;
#46144 = CARTESIAN_POINT ( 'NONE',  ( 21.27187500061451786, 3.027376345333611329, 5.243569643749999010 ) ) ;
#46145 = CARTESIAN_POINT ( 'NONE',  ( 9.712500000000002132, 2.886751345948126879, 4.999999999999998224 ) ) ;
#46146 = CARTESIAN_POINT ( 'NONE',  ( 26.25000000122903288, -2.886751345948125991, -5.000000000000000000 ) ) ;
#46147 = CARTESIAN_POINT ( 'NONE',  ( 17.52187500061451431, 4.119189519843966529, 2.378215178124999607 ) ) ;
#46148 = CARTESIAN_POINT ( 'NONE',  ( 21.89062500061451289, -3.027376345333610441, -5.243569643749999898 ) ) ;
#46149 = CARTESIAN_POINT ( 'NONE',  ( 13.37812500061451715, 6.421520780324663323E-16, -5.243569643749999010 ) ) ;
#46150 = CARTESIAN_POINT ( 'NONE',  ( 26.97187500061451360, 4.119189519843966529, 2.378215178124999607 ) ) ;
#46151 = CARTESIAN_POINT ( 'NONE',  ( 11.14687500061451608, -3.027376345333610441, -5.243569643749999898 ) ) ;
#46152 = CARTESIAN_POINT ( 'NONE',  ( 27.78749999999999787, -2.886751345948129988, 4.999999999999997335 ) ) ;
#46153 = CARTESIAN_POINT ( 'NONE',  ( 21.48750000122903003, 4.330127018922191873, 2.499999999999999556 ) ) ;
#46154 = CARTESIAN_POINT ( 'NONE',  ( 26.88749999999999929, -2.886751345948130876, 4.999999999999996447 ) ) ;
#46155 = CARTESIAN_POINT ( 'NONE',  ( 10.77187500061451786, 3.027376345333613106, -5.243569643749998122 ) ) ;
#46156 = CARTESIAN_POINT ( 'NONE',  ( 28.80937500061451573, 4.541064518000418104, -2.621784821874998173 ) ) ;
#46157 = CARTESIAN_POINT ( 'NONE',  ( 2.934375000614518392, -4.541064518000419881, 2.621784821874995952 ) ) ;
#46158 = DIRECTION ( 'NONE',  ( 0.000000000000000000, 0.000000000000000000, 1.000000000000000000 ) ) ;
#46159 = CARTESIAN_POINT ( 'NONE',  ( 22.39687500061451075, -3.027376345333610441, -5.243569643749999898 ) ) ;
#46160 = CARTESIAN_POINT ( 'NONE',  ( 13.09687500061451892, 6.054752690667223547, 3.707466751127219781E-16 ) ) ;
#46161 = CARTESIAN_POINT ( 'NONE',  ( 3.756430356250000546, 17.29062499938548214, 27.83122392262697886 ) ) ;
#46162 = CARTESIAN_POINT ( 'NONE',  ( 26.69999999999999929, 4.330127018922192761, -2.499999999999997780 ) ) ;
#46163 = CARTESIAN_POINT ( 'NONE',  ( -3.756430356249999214, 20.47812499938548214, 27.83122392262697531 ) ) ;
#46164 = CARTESIAN_POINT ( 'NONE',  ( 28.28437500061451715, 5.824947211148865298E-16, -4.756430356249998326 ) ) ;
#46165 = CARTESIAN_POINT ( 'NONE',  ( 17.72812500061451502, -4.541064518000419881, 2.621784821874995952 ) ) ;
#46166 = CARTESIAN_POINT ( 'NONE',  ( 7.087499999999999467, -2.886751345948129988, 4.999999999999997335 ) ) ;
#46167 = CARTESIAN_POINT ( 'NONE',  ( -0.6945863667395647534, 9.663023495605401081, 26.06076786935074097 ) ) ;
#46168 = CARTESIAN_POINT ( 'NONE',  ( 14.51250000000000107, 2.886751345948129099, -4.999999999999998224 ) ) ;
#46169 = ADVANCED_FACE ( 'NONE', ( #42380 ), #12482, .T. ) ;
#46170 = CARTESIAN_POINT ( 'NONE',  ( -4.243569643749999898, 11.25312500061451892, 30.00000000000000000 ) ) ;
#46171 = DIRECTION ( 'NONE',  ( 0.000000000000000000, 0.000000000000000000, 1.000000000000000000 ) ) ;
#46172 = CARTESIAN_POINT ( 'NONE',  ( 25.84687500061451360, -3.027376345333614438, 5.243569643749998122 ) ) ;
#46173 = ORIENTED_EDGE ( 'NONE', *, *, #35222, .F. ) ;
#46174 = CARTESIAN_POINT ( 'NONE',  ( 22.90312500061451573, 4.541064518000418104, -2.621784821874998173 ) ) ;
#46175 = CARTESIAN_POINT ( 'NONE',  ( 19.13437500061451857, -4.541064518000419881, 2.621784821874995952 ) ) ;
#46176 = CARTESIAN_POINT ( 'NONE',  ( 4.462500000000001243, -5.773502691896255534, -1.060575238724906372E-15 ) ) ;
#46177 = CARTESIAN_POINT ( 'NONE',  ( 6.478125000614516793, -4.541064518000419881, 2.621784821874995952 ) ) ;
#46178 = CARTESIAN_POINT ( 'NONE',  ( 22.30312500061451431, -4.541064518000417216, -2.621784821875001281 ) ) ;
#46179 = CARTESIAN_POINT ( 'NONE',  ( 11.48437500061451644, -4.541064518000419881, 2.621784821874995952 ) ) ;
#46180 = CARTESIAN_POINT ( 'NONE',  ( 16.43437500061451573, -4.541064518000419881, 2.621784821874995952 ) ) ;
#46181 = CARTESIAN_POINT ( 'NONE',  ( -3.000416591977282496E-16, 16.99062500061451786, 25.09994784771203058 ) ) ;
#46182 = CARTESIAN_POINT ( 'NONE',  ( 19.87500000122903288, -5.773502691896255534, -1.060575238724906372E-15 ) ) ;
#46183 = CARTESIAN_POINT ( 'NONE',  ( 14.29687500061451821, -2.746126346562641984, -4.756430356249999214 ) ) ;
#46184 = CARTESIAN_POINT ( 'NONE',  ( 10.52812500061451750, -4.541064518000419881, 2.621784821874995952 ) ) ;
#46185 = CARTESIAN_POINT ( 'NONE',  ( 4.509375000614518569, 4.541064518000418104, -2.621784821874998173 ) ) ;
#46186 = CARTESIAN_POINT ( 'NONE',  ( 5.784375000614517148, 6.421520780324663323E-16, -5.243569643749999010 ) ) ;
#46187 = CARTESIAN_POINT ( 'NONE',  ( 25.62187500061451573, 3.027376345333613106, -5.243569643749998122 ) ) ;
#46188 = CARTESIAN_POINT ( 'NONE',  ( 17.61562500061451786, 3.027376345333611329, 5.243569643749999010 ) ) ;
#46189 = CARTESIAN_POINT ( 'NONE',  ( 27.30000000122903359, 5.773502691896255534, 3.535250795749688894E-16 ) ) ;
#46190 = CARTESIAN_POINT ( 'NONE',  ( 24.36562500061451786, 3.027376345333611329, 5.243569643749999010 ) ) ;
#46191 = CARTESIAN_POINT ( 'NONE',  ( 23.03437500061451715, 4.541064518000418104, 2.621784821874999949 ) ) ;
#46192 = CARTESIAN_POINT ( 'NONE',  ( 18.02812500061451573, 4.541064518000418104, 2.621784821874999949 ) ) ;
#46193 = CARTESIAN_POINT ( 'NONE',  ( 4.243569643749999898, 17.79687500061451999, 32.45002607614398471 ) ) ;
#46194 = CARTESIAN_POINT ( 'NONE',  ( 22.34062500061451573, -3.027376345333610441, -5.243569643749999898 ) ) ;
#46195 = CARTESIAN_POINT ( 'NONE',  ( 15.37500000000000000, 6.123233995736764310E-16, -4.999999999999998224 ) ) ;
#46196 = VERTEX_POINT ( 'NONE', #25008 ) ;
#46197 = CARTESIAN_POINT ( 'NONE',  ( 26.55000000000000071, -4.330127018922190985, -2.500000000000001332 ) ) ;
#46198 = CARTESIAN_POINT ( 'NONE',  ( -3.999999999999997335, 12.38750000000000107, -27.69059892324149175 ) ) ;
#46199 = CARTESIAN_POINT ( 'NONE',  ( -7.967954043666661671E-16, 18.94062499938548783, 34.33755215474603517 ) ) ;
#46200 = CARTESIAN_POINT ( 'NONE',  ( 29.69062500061451715, 6.054752690667223547, 3.707466751127219781E-16 ) ) ;
#46201 = CARTESIAN_POINT ( 'NONE',  ( 11.01562500061451821, -6.054752690667223547, -1.112240025338166033E-15 ) ) ;
#46202 = CARTESIAN_POINT ( 'NONE',  ( 22.31250000122903288, 4.330127018922192761, -2.499999999999997780 ) ) ;
#46203 = CARTESIAN_POINT ( 'NONE',  ( 26.76562500061451644, -6.054752690667223547, -1.112240025338166033E-15 ) ) ;
#46205 = CARTESIAN_POINT ( 'NONE',  ( 28.76249999999999929, -5.773502691896255534, -1.060575238724906372E-15 ) ) ;
#46204 = STYLED_ITEM ( 'NONE', ( #12380 ), #30285 ) ;
#46206 = CARTESIAN_POINT ( 'NONE',  ( -3.999999999999997335, 15.65000000122903501, -27.69059892324149175 ) ) ;
#46207 = FACE_OUTER_BOUND ( 'NONE', #36419, .T. ) ;
#46208 = CARTESIAN_POINT ( 'NONE',  ( 11.42812500061451608, -4.541064518000419881, 2.621784821874995952 ) ) ;
#46209 = ORIENTED_EDGE ( 'NONE', *, *, #12441, .T. ) ;
#46210 = CARTESIAN_POINT ( 'NONE',  ( 26.84062500061451573, -3.027376345333610441, -5.243569643749999898 ) ) ;
#46211 = CARTESIAN_POINT ( 'NONE',  ( 7.415625000614516793, -6.054752690667223547, -1.112240025338166033E-15 ) ) ;
#46212 = UNCERTAINTY_MEASURE_WITH_UNIT (LENGTH_MEASURE( 1.000000000000000082E-05 ), #53730, 'distance_accuracy_value', 'NONE');
#46213 = CARTESIAN_POINT ( 'NONE',  ( 4.903125000614516615, 4.541064518000418104, -2.621784821874998173 ) ) ;
#46214 = CARTESIAN_POINT ( 'NONE',  ( 16.95937500061451786, -4.119189519843965641, -2.378215178125001383 ) ) ;
#46215 = CARTESIAN_POINT ( 'NONE',  ( 30.00000000000000000, 1.224646799147353059E-15, -9.999999999999998224 ) ) ;
#46216 = CARTESIAN_POINT ( 'NONE',  ( 15.78749999999999964, -2.886751345948125991, -5.000000000000000000 ) ) ;
#46217 = SHAPE_REPRESENTATION ( 'pressure gauge', ( #23765 ), #24934 ) ;
#46218 = CARTESIAN_POINT ( 'NONE',  ( 16.99687500061451573, -3.027376345333610441, -5.243569643749999898 ) ) ;
#46219 = CARTESIAN_POINT ( 'NONE',  ( 12.30000000122903181, -2.886751345948125991, -5.000000000000000000 ) ) ;
#46220 = CARTESIAN_POINT ( 'NONE',  ( 18.15937500061451715, 0.000000000000000000, 5.243569643749999010 ) ) ;
#46221 = CARTESIAN_POINT ( 'NONE',  ( 18.30000000000000071, 0.000000000000000000, 4.999999999999998224 ) ) ;
#46222 = CARTESIAN_POINT ( 'NONE',  ( 21.45937500061451786, -4.541064518000417216, -2.621784821875001281 ) ) ;
#46223 = CARTESIAN_POINT ( 'NONE',  ( -4.243569643749999898, 14.85312500061451679, -30.00000000000000000 ) ) ;
#46224 = CARTESIAN_POINT ( 'NONE',  ( -3.999999999999999112, 16.85000000000000142, 30.00000000000000000 ) ) ;
#46225 = CARTESIAN_POINT ( 'NONE',  ( 24.12187500061451573, 5.824947211148865298E-16, -4.756430356249998326 ) ) ;
#46226 = CARTESIAN_POINT ( 'NONE',  ( 2.000000000000000444, 15.21874999877096535, 26.53589838486224650 ) ) ;
#46227 = CARTESIAN_POINT ( 'NONE',  ( 25.07812500061451644, 6.421520780324663323E-16, -5.243569643749999010 ) ) ;
#46228 = FILL_AREA_STYLE_COLOUR ( '', #47891 ) ;
#46229 = CARTESIAN_POINT ( 'NONE',  ( 28.47187500061451715, 3.027376345333611329, 5.243569643749999010 ) ) ;
#46230 = CARTESIAN_POINT ( 'NONE',  ( 24.78750000000000497, -2.886751345948125991, -5.000000000000000000 ) ) ;
#46231 = CARTESIAN_POINT ( 'NONE',  ( 6.328125000614515550, 4.541064518000418104, 2.621784821874999949 ) ) ;
#46232 = CARTESIAN_POINT ( 'NONE',  ( 25.20937500061451431, 2.746126346562643317, 4.756430356249998326 ) ) ;
#46233 = CARTESIAN_POINT ( 'NONE',  ( 18.64687500061451786, -3.027376345333614438, 5.243569643749998122 ) ) ;
#46234 = CARTESIAN_POINT ( 'NONE',  ( 11.74687500061451573, 0.000000000000000000, 4.756430356249998326 ) ) ;
#46235 = CARTESIAN_POINT ( 'NONE',  ( 4.903125000614516615, 4.541064518000418104, -2.621784821874998173 ) ) ;
#46236 = CARTESIAN_POINT ( 'NONE',  ( 7.996875000614519280, -3.027376345333610441, -5.243569643749999898 ) ) ;
#46237 = ORIENTED_EDGE ( 'NONE', *, *, #16958, .F. ) ;
#46238 = CARTESIAN_POINT ( 'NONE',  ( 18.72187500061451360, -6.054752690667223547, -1.112240025338166033E-15 ) ) ;
#46239 = CARTESIAN_POINT ( 'NONE',  ( 29.38125000122903074, 6.123233995736764310E-16, -4.999999999999998224 ) ) ;
#46240 = CARTESIAN_POINT ( 'NONE',  ( 26.17500000000000071, 6.123233995736764310E-16, -4.999999999999998224 ) ) ;
#46241 = CARTESIAN_POINT ( 'NONE',  ( 29.22187500061451715, 3.027376345333613106, -5.243569643749998122 ) ) ;
#46242 = CARTESIAN_POINT ( 'NONE',  ( 1.626862140677534273E-15, 12.12500000122903465, 34.00000000000000000 ) ) ;
#46243 = DIRECTION ( 'NONE',  ( -0.000000000000000000, -1.000000000000000000, -0.000000000000000000 ) ) ;
#46244 = VERTEX_POINT ( 'NONE', #52727 ) ;
#46245 = CARTESIAN_POINT ( 'NONE',  ( 10.27499999999999858, -4.330127018922194537, 2.499999999999995559 ) ) ;
#46246 = CARTESIAN_POINT ( 'NONE',  ( 12.60937500061451289, 2.746126346562643317, 4.756430356249998326 ) ) ;
#46247 = CARTESIAN_POINT ( 'NONE',  ( 25.00312500061451715, -4.541064518000417216, -2.621784821875001281 ) ) ;
#46248 = CARTESIAN_POINT ( 'NONE',  ( 13.64999999999999858, 4.330127018922192761, -2.499999999999997780 ) ) ;
#46249 = CARTESIAN_POINT ( 'NONE',  ( 10.05000000122903181, -2.886751345948125991, -5.000000000000000000 ) ) ;
#46250 = CARTESIAN_POINT ( 'NONE',  ( 9.178125000614517859, -4.541064518000419881, 2.621784821874995952 ) ) ;
#46251 = CARTESIAN_POINT ( 'NONE',  ( 21.89999999999999858, 0.000000000000000000, 4.999999999999998224 ) ) ;
#46252 = ADVANCED_FACE ( 'NONE', ( #13192 ), #35009, .F. ) ;
#46253 = CARTESIAN_POINT ( 'NONE',  ( 21.21562500061451573, 3.027376345333611329, 5.243569643749999010 ) ) ;
#46254 = CARTESIAN_POINT ( 'NONE',  ( 18.63750000122903216, 6.123233995736764310E-16, -4.999999999999998224 ) ) ;
#46255 = AXIS2_PLACEMENT_3D ( 'NONE', #37643, #71264, #42466 ) ;
#46256 = CARTESIAN_POINT ( 'NONE',  ( 26.06250000122903288, 0.000000000000000000, 4.999999999999998224 ) ) ;
#46257 = CARTESIAN_POINT ( 'NONE',  ( -7.967954043666661671E-16, 17.47812499938548214, 34.33755215474603517 ) ) ;
#46258 = CARTESIAN_POINT ( 'NONE',  ( 8.437500000000000000, -2.886751345948129988, 4.999999999999997335 ) ) ;
#46259 = ORIENTED_EDGE ( 'NONE', *, *, #18286, .F. ) ;
#46260 = CARTESIAN_POINT ( 'NONE',  ( 22.82812500061451644, 6.421520780324663323E-16, -5.243569643749999010 ) ) ;
#46261 = CARTESIAN_POINT ( 'NONE',  ( 26.82187500061451857, -6.054752690667223547, -1.112240025338166033E-15 ) ) ;
#46262 = CARTESIAN_POINT ( 'NONE',  ( 17.89687500061451431, -3.027376345333610441, -5.243569643749999898 ) ) ;
#46263 = CARTESIAN_POINT ( 'NONE',  ( 14.24062500061451608, -3.027376345333610441, -5.243569643749999898 ) ) ;
#46264 = CARTESIAN_POINT ( 'NONE',  ( 4.243569643749999898, 10.12812500061459353, -30.00000000000000000 ) ) ;
#46265 =( BOUNDED_CURVE ( )  B_SPLINE_CURVE ( 2, ( #57869, #7278, #24259, #69344, #52703, #18702, #41266, #30172, #2109 ),
 .UNSPECIFIED., .F., .F. ) 
 B_SPLINE_CURVE_WITH_KNOTS ( ( 3, 2, 2, 2, 3 ),
 ( 0.5326086956521739468, 0.5362318840579710644, 0.5434782608695651884, 0.5507246376811594235, 0.5543478260869565410 ),
 .UNSPECIFIED. ) 
 CURVE ( )  GEOMETRIC_REPRESENTATION_ITEM ( )  RATIONAL_B_SPLINE_CURVE ( ( 0.9330127018922194093, 0.9330127018922194093, 1.000000000000000000, 0.8660254037844387076, 1.000000000000000000, 0.8660254037844387076, 1.000000000000000000, 0.9330127018922194093, 0.9330127018922194093 ) ) 
 REPRESENTATION_ITEM ( '' )  );
#46266 = CARTESIAN_POINT ( 'NONE',  ( 26.81250000122903288, 4.330127018922192761, -2.499999999999997780 ) ) ;
#46267 = CARTESIAN_POINT ( 'NONE',  ( 21.42187500061451644, -5.492252693125287522, -1.008910452111647106E-15 ) ) ;
#46268 = CARTESIAN_POINT ( 'NONE',  ( 15.62812500061451537, 6.421520780324663323E-16, -5.243569643749999010 ) ) ;
#46269 = CARTESIAN_POINT ( 'NONE',  ( 13.53750000000000142, -2.886751345948126435, -5.000000000000000000 ) ) ;
#46270 = CARTESIAN_POINT ( 'NONE',  ( 3.225000001229033408, -5.773502691896255534, -1.060575238724906372E-15 ) ) ;
#46271 = CARTESIAN_POINT ( 'NONE',  ( 11.85937500061451644, 0.000000000000000000, 5.243569643749999010 ) ) ;
#46272 = CARTESIAN_POINT ( 'NONE',  ( 12.57187500061451857, 3.027376345333613106, -5.243569643749998122 ) ) ;
#46273 = CARTESIAN_POINT ( 'NONE',  ( 19.58437500061451786, -4.541064518000419881, 2.621784821874995952 ) ) ;
#46274 = EDGE_LOOP ( 'NONE', ( #68599, #28998, #24532, #51521 ) ) ;
#46275 = CARTESIAN_POINT ( 'NONE',  ( 29.39999999999999858, 4.330127018922192761, -2.499999999999997780 ) ) ;
#46276 = CARTESIAN_POINT ( 'NONE',  ( 23.57812500061451289, -4.541064518000419881, 2.621784821874995952 ) ) ;
#46277 = CARTESIAN_POINT ( 'NONE',  ( 20.07187500061451857, -6.054752690667223547, -1.112240025338166033E-15 ) ) ;
#46278 = CARTESIAN_POINT ( 'NONE',  ( 23.42812500061451786, 4.541064518000418104, 2.621784821874999949 ) ) ;
#46279 = CARTESIAN_POINT ( 'NONE',  ( 4.000000000000000000, 14.33750000000000213, 32.30940107675849049 ) ) ;
#46280 = CARTESIAN_POINT ( 'NONE',  ( 28.30312500061451431, 4.541064518000418104, -2.621784821874998173 ) ) ;
#46281 = CARTESIAN_POINT ( 'NONE',  ( 9.787500001229036073, 4.330127018922191873, 2.499999999999999556 ) ) ;
#46282 = CARTESIAN_POINT ( 'NONE',  ( 3.787500001229033408, 6.123233995736764310E-16, -4.999999999999998224 ) ) ;
#46283 = CARTESIAN_POINT ( 'NONE',  ( 26.85000000122903430, 5.773502691896255534, 3.535250795749688894E-16 ) ) ;
#46284 = CARTESIAN_POINT ( 'NONE',  ( -8.484601909799255319E-16, 19.98124999877096641, 34.61880215351700940 ) ) ;
#46285 = CARTESIAN_POINT ( 'NONE',  ( 15.73125000122903216, -4.330127018922194537, 2.499999999999995559 ) ) ;
#46286 = CARTESIAN_POINT ( 'NONE',  ( 8.446875000614518569, -3.027376345333610441, -5.243569643749999898 ) ) ;
#46287 = CARTESIAN_POINT ( 'NONE',  ( 24.44999999999999929, 4.330127018922192761, -2.499999999999997780 ) ) ;
#46288 = CARTESIAN_POINT ( 'NONE',  ( 18.47812500061451857, 4.541064518000418104, 2.621784821874999949 ) ) ;
#46289 = CARTESIAN_POINT ( 'NONE',  ( 10.02187500061451964, 3.027376345333611329, 5.243569643749999010 ) ) ;
#46290 = CARTESIAN_POINT ( 'NONE',  ( 29.36250000122903003, -4.330127018922190985, -2.500000000000001332 ) ) ;
#46291 = CARTESIAN_POINT ( 'NONE',  ( 19.24687500061452283, -3.027376345333610441, -5.243569643749999898 ) ) ;
#46292 = CARTESIAN_POINT ( 'NONE',  ( 7.771875000614516971, 3.027376345333611329, 5.243569643749999010 ) ) ;
#46293 = CARTESIAN_POINT ( 'NONE',  ( 3.081468785175471403, -3.937611012629079976, -3.302521940835167591 ) ) ;
#46294 = CARTESIAN_POINT ( 'NONE',  ( 50.00000000000000000, 7.332543590861084759, -5.218601775200136572 ) ) ;
#46295 = CARTESIAN_POINT ( 'NONE',  ( 8.015625000614518214, 3.027376345333613106, -5.243569643749998122 ) ) ;
#46296 = CARTESIAN_POINT ( 'NONE',  ( 18.29062500061451502, -3.027376345333610441, -5.243569643749999898 ) ) ;
#46297 =( BOUNDED_CURVE ( )  B_SPLINE_CURVE ( 2, ( #42027, #25764, #13941, #71564, #30930, #8040, #15033 ),
 .UNSPECIFIED., .F., .F. ) 
 B_SPLINE_CURVE_WITH_KNOTS ( ( 3, 2, 2, 3 ),
 ( 0.4416666666666666519, 0.4444444444444444753, 0.4472222222222222987, 0.4500000000000001221 ),
 .UNSPECIFIED. ) 
 CURVE ( )  GEOMETRIC_REPRESENTATION_ITEM ( )  RATIONAL_B_SPLINE_CURVE ( ( 1.000000000000000000, 0.8660254037844387076, 1.000000000000000000, 0.8660254037844387076, 1.000000000000000000, 0.8660254037844333785, 1.000000000000005329 ) ) 
 REPRESENTATION_ITEM ( '' )  );
#46298 = ORIENTED_EDGE ( 'NONE', *, *, #25301, .T. ) ;
#46299 = CARTESIAN_POINT ( 'NONE',  ( 4.762500001229033941, 4.330127018922192761, -2.499999999999997780 ) ) ;
#46300 = CARTESIAN_POINT ( 'NONE',  ( 14.20312500061451644, -4.541064518000417216, -2.621784821875001281 ) ) ;
#46301 = CARTESIAN_POINT ( 'NONE',  ( 14.31562500061451537, 3.027376345333613106, -5.243569643749998122 ) ) ;
#46302 = CARTESIAN_POINT ( 'NONE',  ( 24.04687500061451644, -2.746126346562646425, 4.756430356249996549 ) ) ;
#46303 = CARTESIAN_POINT ( 'NONE',  ( 13.91249999999999964, -5.773502691896255534, -1.060575238724906372E-15 ) ) ;
#46304 = CARTESIAN_POINT ( 'NONE',  ( 7.012500001229035718, 4.330127018922192761, -2.499999999999997780 ) ) ;
#46305 = CARTESIAN_POINT ( 'NONE',  ( 6.403125000614517504, 0.000000000000000000, 5.243569643749999010 ) ) ;
#46306 = EDGE_CURVE ( 'NONE', #23351, #829, #43511, .T. ) ;
#46307 = AXIS2_PLACEMENT_3D ( 'NONE', #48819, #54724, #48088 ) ;
#46308 = CARTESIAN_POINT ( 'NONE',  ( 17.73750000122903359, 6.123233995736764310E-16, -4.999999999999998224 ) ) ;
#46309 = CARTESIAN_POINT ( 'NONE',  ( 24.41250000000000142, 2.886751345948129099, -4.999999999999998224 ) ) ;
#46310 =( BOUNDED_CURVE ( )  B_SPLINE_CURVE ( 2, ( #57996, #57639, #35116, #17745, #24750, #51753, #57279, #46936, #69473 ),
 .UNSPECIFIED., .F., .F. ) 
 B_SPLINE_CURVE_WITH_KNOTS ( ( 3, 2, 2, 2, 3 ),
 ( 0.6847826086956522174, 0.6884057971014492239, 0.6956521739130434590, 0.7028985507246376940, 0.7065217391304348116 ),
 .UNSPECIFIED. ) 
 CURVE ( )  GEOMETRIC_REPRESENTATION_ITEM ( )  RATIONAL_B_SPLINE_CURVE ( ( 0.9330127018922192983, 0.9330127018922202975, 1.000000000000000000, 0.8660254037844387076, 1.000000000000000000, 0.8660254037844387076, 1.000000000000000000, 0.9330127018922194093, 0.9330127018922194093 ) ) 
 REPRESENTATION_ITEM ( '' )  );
#46311 = ADVANCED_FACE ( 'NONE', ( #19090 ), #41645, .F. ) ;
#46312 = CARTESIAN_POINT ( 'NONE',  ( 2.121784821874999061, 10.70937500061451964, -33.67503911421598417 ) ) ;
#46313 = FACE_OUTER_BOUND ( 'NONE', #66611, .T. ) ;
#46314 = CARTESIAN_POINT ( 'NONE',  ( 4.400918202330496243, -2.373166445152071535, -4.675799785326651303 ) ) ;
#46315 = CARTESIAN_POINT ( 'NONE',  ( -1.626862140677534273E-15, 14.63749999999999929, 34.00000000000000000 ) ) ;
#46316 = CARTESIAN_POINT ( 'NONE',  ( 13.87500000000000178, -4.330127018922194537, 2.499999999999995559 ) ) ;
#46317 = CARTESIAN_POINT ( 'NONE',  ( 17.67187500061451644, 3.027376345333611329, 5.243569643749999010 ) ) ;
#46318 = EDGE_CURVE ( 'NONE', #57370, #33074, #13282, .T. ) ;
#46319 = CARTESIAN_POINT ( 'NONE',  ( 22.85625000122903216, 0.000000000000000000, 4.999999999999998224 ) ) ;
#46320 = CARTESIAN_POINT ( 'NONE',  ( 15.21562500061451750, 3.027376345333613106, -5.243569643749998122 ) ) ;
#46321 = CARTESIAN_POINT ( 'NONE',  ( 8.418750001229032165, 2.886751345948126879, 4.999999999999999112 ) ) ;
#46322 = CARTESIAN_POINT ( 'NONE',  ( 15.71250000122903501, 0.000000000000000000, 4.999999999999998224 ) ) ;
#46323 = CARTESIAN_POINT ( 'NONE',  ( 26.44687500061451502, -3.027376345333610441, -5.243569643749999898 ) ) ;
#46324 = CARTESIAN_POINT ( 'NONE',  ( 17.33437500061451431, -2.746126346562641984, -4.756430356249999214 ) ) ;
#46325 = CARTESIAN_POINT ( 'NONE',  ( 11.95312500061451644, -4.541064518000417216, -2.621784821875001281 ) ) ;
#46326 = CARTESIAN_POINT ( 'NONE',  ( 16.39687500061451786, -3.027376345333614438, 5.243569643749998122 ) ) ;
#46327 = ORIENTED_EDGE ( 'NONE', *, *, #65368, .F. ) ;
#46328 = CARTESIAN_POINT ( 'NONE',  ( 27.29062500061451502, -3.027376345333610441, -5.243569643749999898 ) ) ;
#46329 = CARTESIAN_POINT ( 'NONE',  ( 20.72812500061451502, 4.541064518000418104, 2.621784821874999949 ) ) ;
#46330 = DIRECTION ( 'NONE',  ( 0.000000000000000000, 0.000000000000000000, 1.000000000000000000 ) ) ;
#46331 = EDGE_CURVE ( 'NONE', #53529, #23511, #25752, .T. ) ;
#46332 = CARTESIAN_POINT ( 'NONE',  ( 30.00000000000000000, 6.123233995736764310E-16, -4.999999999999998224 ) ) ;
#46333 = CARTESIAN_POINT ( 'NONE',  ( 9.525000000000002132, 6.123233995736764310E-16, -4.999999999999998224 ) ) ;
#46334 = CARTESIAN_POINT ( 'NONE',  ( 19.65000000122902790, 5.773502691896255534, 3.535250795749688894E-16 ) ) ;
#46335 = FACE_OUTER_BOUND ( 'NONE', #72108, .T. ) ;
#46336 = CARTESIAN_POINT ( 'NONE',  ( 10.84687500061451715, 0.000000000000000000, 4.756430356249998326 ) ) ;
#46337 = EDGE_LOOP ( 'NONE', ( #30515, #13543, #19702, #37 ) ) ;
#46338 = CARTESIAN_POINT ( 'NONE',  ( 17.17500000000000071, 6.123233995736764310E-16, -4.999999999999998224 ) ) ;
#46339 = CARTESIAN_POINT ( 'NONE',  ( 20.21250000000000213, -5.773502691896255534, -1.060575238724906372E-15 ) ) ;
#46340 = CARTESIAN_POINT ( 'NONE',  ( 18.57187500061451857, 3.027376345333611329, 5.243569643749999010 ) ) ;
#46341 = CARTESIAN_POINT ( 'NONE',  ( 24.25312500061451715, 4.541064518000418104, -2.621784821874998173 ) ) ;
#46342 = ORIENTED_EDGE ( 'NONE', *, *, #7032, .T. ) ;
#46343 = DIRECTION ( 'NONE',  ( -0.000000000000000000, -1.000000000000000000, -0.000000000000000000 ) ) ;
#46344 = CARTESIAN_POINT ( 'NONE',  ( 9.403125000614517504, 4.541064518000418104, -2.621784821874998173 ) ) ;
#46345 = CARTESIAN_POINT ( 'NONE',  ( 3.152458665894561474, 4.261886542965685365, -3.105335258989349700 ) ) ;
#46346 = CARTESIAN_POINT ( 'NONE',  ( 15.48749999999999893, 5.773502691896255534, 3.535250795749688894E-16 ) ) ;
#46347 = CARTESIAN_POINT ( 'NONE',  ( -3.000416591977282496E-16, 18.79062500061451857, 25.09994784771203058 ) ) ;
#46348 = CARTESIAN_POINT ( 'NONE',  ( 29.46562500061451573, -6.054752690667223547, -1.112240025338166033E-15 ) ) ;
#46349 = CARTESIAN_POINT ( 'NONE',  ( 11.77500000000000036, 6.123233995736764310E-16, -4.999999999999998224 ) ) ;
#46350 = CARTESIAN_POINT ( 'NONE',  ( -3.756430356250001434, 17.40312499938548285, 32.16877607737301048 ) ) ;
#46351 = CARTESIAN_POINT ( 'NONE',  ( 27.34687500061451360, -3.027376345333610441, -5.243569643749999898 ) ) ;
#46352 = EDGE_LOOP ( 'NONE', ( #23152, #4067, #27274, #56422 ) ) ;
#46353 = CARTESIAN_POINT ( 'NONE',  ( 22.26562500061451644, -6.054752690667223547, -1.112240025338166033E-15 ) ) ;
#46354 = CARTESIAN_POINT ( 'NONE',  ( 22.99687500061451573, 6.054752690667223547, 3.707466751127219781E-16 ) ) ;
#46355 = CARTESIAN_POINT ( 'NONE',  ( 4.243569643749999010, 16.01562500061459460, -32.45002607614398471 ) ) ;
#46356 = CARTESIAN_POINT ( 'NONE',  ( 10.38750000000000107, -2.886751345948125991, -5.000000000000000000 ) ) ;
#46357 = CARTESIAN_POINT ( 'NONE',  ( 5.353125000614515905, 4.541064518000418104, -2.621784821874998173 ) ) ;
#46358 = CARTESIAN_POINT ( 'NONE',  ( 28.58437500061451786, -4.119189519843968306, 2.378215178124996054 ) ) ;
#46359 = CARTESIAN_POINT ( 'NONE',  ( 23.09062500061451573, -3.027376345333614438, 5.243569643749998122 ) ) ;
#46360 = CARTESIAN_POINT ( 'NONE',  ( 27.49687500061451573, 0.000000000000000000, 4.756430356249998326 ) ) ;
#46361 = CARTESIAN_POINT ( 'NONE',  ( 13.50937500061451679, 4.119189519843966529, -2.378215178124998275 ) ) ;
#46362 = CARTESIAN_POINT ( 'NONE',  ( 16.84687500061451715, -3.027376345333614438, 5.243569643749998122 ) ) ;
#46363 = CARTESIAN_POINT ( 'NONE',  ( -2.121784821874999949, 13.48437500061451821, 26.32496088578401938 ) ) ;
#46364 = CARTESIAN_POINT ( 'NONE',  ( 18.19687500061451502, -3.027376345333614438, 5.243569643749998122 ) ) ;
#46365 = CARTESIAN_POINT ( 'NONE',  ( 26.37187500061451217, -6.054752690667223547, -1.112240025338166033E-15 ) ) ;
#46366 = CARTESIAN_POINT ( 'NONE',  ( -2.121784821874996840, 15.88437500061451857, 33.67503911421598417 ) ) ;
#46367 = CARTESIAN_POINT ( 'NONE',  ( 7.828125000614517326, -4.541064518000419881, 2.621784821874995952 ) ) ;
#46368 = CYLINDRICAL_SURFACE ( 'NONE', #59596, 4.999999999999998224 ) ;
#46369 = CARTESIAN_POINT ( 'NONE',  ( 3.871875000614519280, -6.054752690667223547, -1.112240025338166033E-15 ) ) ;
#46370 = CARTESIAN_POINT ( 'NONE',  ( 45.00000000000000000, -1.494782592887594852, 8.875000000000012434 ) ) ;
#46371 = CARTESIAN_POINT ( 'NONE',  ( 4.940625000614515372, 6.054752690667223547, 3.707466751127219781E-16 ) ) ;
#46372 = CARTESIAN_POINT ( 'NONE',  ( 9.759375000614516793, -4.541064518000417216, -2.621784821875001281 ) ) ;
#46373 = CARTESIAN_POINT ( 'NONE',  ( 16.76250000122903216, -4.330127018922190985, -2.500000000000001332 ) ) ;
#46374 = CARTESIAN_POINT ( 'NONE',  ( 5.184375000614516615, -4.541064518000419881, 2.621784821874995952 ) ) ;
#46375 = CARTESIAN_POINT ( 'NONE',  ( 7.340625000614518392, -3.027376345333614438, 5.243569643749998122 ) ) ;
#46376 = CARTESIAN_POINT ( 'NONE',  ( 8.287500001229034297, 6.123233995736764310E-16, -4.999999999999998224 ) ) ;
#46377 = CARTESIAN_POINT ( 'NONE',  ( 23.86875000122903501, -5.773502691896255534, -1.060575238724906372E-15 ) ) ;
#46378 = CARTESIAN_POINT ( 'NONE',  ( 17.18437500061451573, 4.541064518000418104, 2.621784821874999949 ) ) ;
#46379 = CARTESIAN_POINT ( 'NONE',  ( 27.75000000000000000, 0.000000000000000000, 4.999999999999998224 ) ) ;
#46380 = ORIENTED_EDGE ( 'NONE', *, *, #42309, .F. ) ;
#46381 = CARTESIAN_POINT ( 'NONE',  ( 24.85312500061451502, 0.000000000000000000, 5.243569643749999010 ) ) ;
#46382 = CARTESIAN_POINT ( 'NONE',  ( 9.890625000614516438, 6.054752690667223547, 3.707466751127219781E-16 ) ) ;
#46383 = CARTESIAN_POINT ( 'NONE',  ( 26.33437500061451431, -4.541064518000419881, 2.621784821874995952 ) ) ;
#46384 = CARTESIAN_POINT ( 'NONE',  ( 9.928125000614517859, 4.541064518000418104, 2.621784821874999949 ) ) ;
#46385 = CARTESIAN_POINT ( 'NONE',  ( -1.394453263437886801E-15, 19.32500000122903216, -26.00000000000000000 ) ) ;
#46386 = CARTESIAN_POINT ( 'NONE',  ( 10.08750000122903323, 6.123233995736764310E-16, -4.999999999999998224 ) ) ;
#46387 = CARTESIAN_POINT ( 'NONE',  ( 25.34062500061451217, -3.027376345333614438, 5.243569643749998122 ) ) ;
#46388 = CARTESIAN_POINT ( 'NONE',  ( -2.121784821874996840, 14.02812500061451750, -26.32496088578401583 ) ) ;
#46389 = CARTESIAN_POINT ( 'NONE',  ( 11.92500000122903181, 2.886751345948129099, -4.999999999999998224 ) ) ;
#46390 = CARTESIAN_POINT ( 'NONE',  ( 23.09062500061451573, -3.027376345333614438, 5.243569643749998122 ) ) ;
#46391 = CARTESIAN_POINT ( 'NONE',  ( 11.66249999999999964, -5.773502691896255534, -1.060575238724906372E-15 ) ) ;
#46392 = CARTESIAN_POINT ( 'NONE',  ( 19.60312500061451502, -4.541064518000417216, -2.621784821875001281 ) ) ;
#46393 = CARTESIAN_POINT ( 'NONE',  ( 5.784375000614517148, 6.421520780324663323E-16, -5.243569643749999010 ) ) ;
#46394 = CARTESIAN_POINT ( 'NONE',  ( 19.87500000000000000, 6.123233995736764310E-16, -4.999999999999998224 ) ) ;
#46395 = CARTESIAN_POINT ( 'NONE',  ( 7.312500001229033764, -4.330127018922190985, -2.500000000000001332 ) ) ;
#46396 = CARTESIAN_POINT ( 'NONE',  ( 16.38750000122903216, 6.123233995736764310E-16, -4.999999999999998224 ) ) ;
#46397 = CARTESIAN_POINT ( 'NONE',  ( 11.80312500061451608, 0.000000000000000000, 5.243569643749999010 ) ) ;
#46398 = CARTESIAN_POINT ( 'NONE',  ( 15.29062500061451679, 6.054752690667223547, 3.707466751127219781E-16 ) ) ;
#46399 = CARTESIAN_POINT ( 'NONE',  ( 25.31250000122903288, -4.330127018922190985, -2.500000000000001332 ) ) ;
#46400 = CARTESIAN_POINT ( 'NONE',  ( 20.17499999999999716, -4.330127018922194537, 2.499999999999995559 ) ) ;
#46401 = CARTESIAN_POINT ( 'NONE',  ( 23.40937500061451715, 4.541064518000418104, -2.621784821874998173 ) ) ;
#46402 = CARTESIAN_POINT ( 'NONE',  ( 10.68750000122903288, 4.330127018922191873, 2.499999999999999556 ) ) ;
#46403 = CARTESIAN_POINT ( 'NONE',  ( 8.559375000614515727, 4.541064518000418104, -2.621784821874998173 ) ) ;
#46404 = CARTESIAN_POINT ( 'NONE',  ( 24.83437500061451431, 4.541064518000418104, 2.621784821874999949 ) ) ;
#46405 = ADVANCED_FACE ( 'NONE', ( #26114 ), #71178, .T. ) ;
#46406 = CARTESIAN_POINT ( 'NONE',  ( 3.234375000614516438, 4.541064518000418104, 2.621784821874999949 ) ) ;
#46407 = CARTESIAN_POINT ( 'NONE',  ( 21.62812500061451360, 4.541064518000418104, 2.621784821874999949 ) ) ;
#46408 = CARTESIAN_POINT ( 'NONE',  ( 26.33437500061451431, -4.541064518000419881, 2.621784821874995952 ) ) ;
#46409 = CARTESIAN_POINT ( 'NONE',  ( -1.878215178124999163, 18.30312499938548143, 26.74683588394047007 ) ) ;
#46410 = CARTESIAN_POINT ( 'NONE',  ( 19.29375000122903927, -2.886751345948130876, 4.999999999999996447 ) ) ;
#46411 = CARTESIAN_POINT ( 'NONE',  ( 6.721875000614518925, 3.027376345333613106, -5.243569643749998122 ) ) ;
#46412 = CARTESIAN_POINT ( 'NONE',  ( 20.12812500061451715, 6.421520780324663323E-16, -5.243569643749999010 ) ) ;
#46413 = ORIENTED_EDGE ( 'NONE', *, *, #22559, .T. ) ;
#46414 = CARTESIAN_POINT ( 'NONE',  ( 16.05000000000000071, 0.000000000000000000, 4.999999999999998224 ) ) ;
#46415 = CARTESIAN_POINT ( 'NONE',  ( 27.89062500061451289, 6.054752690667223547, 3.707466751127219781E-16 ) ) ;
#46416 = CARTESIAN_POINT ( 'NONE',  ( 3.496875000614518836, -3.027376345333610441, -5.243569643749999898 ) ) ;
#46417 = CARTESIAN_POINT ( 'NONE',  ( 6.675000000000000711, -4.330127018922194537, 2.499999999999995559 ) ) ;
#46418 = FACE_OUTER_BOUND ( 'NONE', #43523, .T. ) ;
#46419 = CARTESIAN_POINT ( 'NONE',  ( 17.69999999999999929, 4.330127018922192761, -2.499999999999997780 ) ) ;
#46420 = CARTESIAN_POINT ( 'NONE',  ( 20.91562500061451502, -6.054752690667223547, -1.112240025338166033E-15 ) ) ;
#46421 = ORIENTED_EDGE ( 'NONE', *, *, #50590, .T. ) ;
#46422 = CARTESIAN_POINT ( 'NONE',  ( 25.91250000000000142, 2.886751345948126879, 4.999999999999999112 ) ) ;
#46423 = CARTESIAN_POINT ( 'NONE',  ( 26.67187500061451644, 3.027376345333611329, 5.243569643749999010 ) ) ;
#46424 = ORIENTED_EDGE ( 'NONE', *, *, #68767, .T. ) ;
#46425 = CARTESIAN_POINT ( 'NONE',  ( 16.11562500061451786, 3.027376345333613106, -5.243569643749998122 ) ) ;
#46426 = CARTESIAN_POINT ( 'NONE',  ( 5.540625000614515905, -3.027376345333614438, 5.243569643749998122 ) ) ;
#46427 = CARTESIAN_POINT ( 'NONE',  ( 19.17187500061451289, 5.824947211148865298E-16, -4.756430356249998326 ) ) ;
#46428 = CARTESIAN_POINT ( 'NONE',  ( 28.07812500061451289, -4.541064518000419881, 2.621784821874995952 ) ) ;
#46429 = CARTESIAN_POINT ( 'NONE',  ( 14.32500000122903394, 2.886751345948126879, 4.999999999999999112 ) ) ;
#46430 = CARTESIAN_POINT ( 'NONE',  ( 21.11249999999999716, -5.773502691896255534, -1.060575238724906372E-15 ) ) ;
#46431 = CARTESIAN_POINT ( 'NONE',  ( 28.23750000000000426, -2.886751345948129988, 4.999999999999997335 ) ) ;
#46432 = CARTESIAN_POINT ( 'NONE',  ( 4.884375000614518569, 6.421520780324663323E-16, -5.243569643749999010 ) ) ;
#46433 = CARTESIAN_POINT ( 'NONE',  ( 8.934375000614517504, 6.421520780324663323E-16, -5.243569643749999010 ) ) ;
#46434 = CARTESIAN_POINT ( 'NONE',  ( 20.22187500061451715, 3.027376345333613106, -5.243569643749998122 ) ) ;
#46435 = CARTESIAN_POINT ( 'NONE',  ( 10.01250000122903394, -4.330127018922190985, -2.500000000000001332 ) ) ;
#46436 = ORIENTED_EDGE ( 'NONE', *, *, #39683, .F. ) ;
#46437 = CARTESIAN_POINT ( 'NONE',  ( 29.42812500061451431, -4.541064518000419881, 2.621784821874995952 ) ) ;
#46438 = CARTESIAN_POINT ( 'NONE',  ( 3.450000000000001510, 0.000000000000000000, 4.999999999999998224 ) ) ;
#46440 = ADVANCED_FACE ( 'NONE', ( #43479 ), #9124, .T. ) ;
#46439 = CARTESIAN_POINT ( 'NONE',  ( 5.409375000614516260, 4.541064518000418104, -2.621784821874998173 ) ) ;
#46441 = CARTESIAN_POINT ( 'NONE',  ( 19.27500000000000213, -4.330127018922194537, 2.499999999999995559 ) ) ;
#46442 = CARTESIAN_POINT ( 'NONE',  ( 16.97812500061451502, 6.421520780324663323E-16, -5.243569643749999010 ) ) ;
#46443 = CARTESIAN_POINT ( 'NONE',  ( -4.000000000000000888, 20.41250000000000142, 32.30940107675850470 ) ) ;
#46444 = DIRECTION ( 'NONE',  ( -0.000000000000000000, -1.000000000000000000, -0.000000000000000000 ) ) ;
#46445 = CARTESIAN_POINT ( 'NONE',  ( 19.50937500061451857, 0.000000000000000000, 4.756430356249998326 ) ) ;
#46446 = CARTESIAN_POINT ( 'NONE',  ( 7.453125000614516438, -4.541064518000417216, -2.621784821875001281 ) ) ;
#46447 = CARTESIAN_POINT ( 'NONE',  ( 26.44687500061451502, -3.027376345333610441, -5.243569643749999898 ) ) ;
#46448 = CARTESIAN_POINT ( 'NONE',  ( -4.243569643749999898, 18.50937500061451857, 30.00000000000000000 ) ) ;
#46449 = CARTESIAN_POINT ( 'NONE',  ( 26.67187500061451644, 3.027376345333611329, 5.243569643749999010 ) ) ;
#46450 = CARTESIAN_POINT ( 'NONE',  ( 6.975000000000002309, 4.330127018922191873, 2.499999999999999556 ) ) ;
#46451 = CARTESIAN_POINT ( 'NONE',  ( -3.999999999999999556, 11.97500000122903252, 27.69059892324149530 ) ) ;
#46452 = CARTESIAN_POINT ( 'NONE',  ( 14.95312500061451644, 0.000000000000000000, 5.243569643749999010 ) ) ;
#46453 = CARTESIAN_POINT ( 'NONE',  ( 7.387500001229032165, 6.123233995736764310E-16, -4.999999999999998224 ) ) ;
#46454 = CARTESIAN_POINT ( 'NONE',  ( 16.88437500061451502, -4.541064518000419881, 2.621784821874995952 ) ) ;
#46455 = CARTESIAN_POINT ( 'NONE',  ( 12.75937500061451857, 0.000000000000000000, 5.243569643749999010 ) ) ;
#46456 = CARTESIAN_POINT ( 'NONE',  ( 21.44999999999999929, 0.000000000000000000, 4.999999999999998224 ) ) ;
#46457 = ORIENTED_EDGE ( 'NONE', *, *, #40712, .F. ) ;
#46458 = CARTESIAN_POINT ( 'NONE',  ( 12.21562500061451573, 3.027376345333611329, 5.243569643749999010 ) ) ;
#46459 = CARTESIAN_POINT ( 'NONE',  ( 24.63750000122903216, 4.330127018922191873, 2.499999999999999556 ) ) ;
#46460 = CARTESIAN_POINT ( 'NONE',  ( 13.92187500061451644, 3.027376345333613106, -5.243569643749998122 ) ) ;
#46461 = CARTESIAN_POINT ( 'NONE',  ( 4.044621064622349493, 3.945521627023633293, -3.653295367133241545 ) ) ;
#46462 = CARTESIAN_POINT ( 'NONE',  ( 14.95312500061451644, 0.000000000000000000, 5.243569643749999010 ) ) ;
#46463 = CARTESIAN_POINT ( 'NONE',  ( 20.83125000122903359, 6.123233995736764310E-16, -4.999999999999998224 ) ) ;
#46464 = EDGE_CURVE ( 'NONE', #56819, #44169, #71338, .T. ) ;
#46465 = CARTESIAN_POINT ( 'NONE',  ( 24.94687500061451502, -3.027376345333614438, 5.243569643749998122 ) ) ;
#46466 = LINE ( 'NONE', #47190, #10080 ) ;
#46467 = CARTESIAN_POINT ( 'NONE',  ( 11.43750000122903465, 6.123233995736764310E-16, -4.999999999999998224 ) ) ;
#46468 = FACE_OUTER_BOUND ( 'NONE', #21701, .T. ) ;
#46469 = CARTESIAN_POINT ( 'NONE',  ( -1.071796769724490339, 19.64240381056766438, 34.00000000000000000 ) ) ;
#46470 = CARTESIAN_POINT ( 'NONE',  ( 4.243569643749999898, 16.03437500061451715, -30.00000000000000000 ) ) ;
#46471 = CARTESIAN_POINT ( 'NONE',  ( 17.22187500061451715, 3.027376345333611329, 5.243569643749999010 ) ) ;
#46472 = CARTESIAN_POINT ( 'NONE',  ( 17.17500000122903359, -5.773502691896255534, -1.060575238724906372E-15 ) ) ;
#46473 = CARTESIAN_POINT ( 'NONE',  ( 15.15937500061451715, -4.541064518000417216, -2.621784821875001281 ) ) ;
#46474 = CARTESIAN_POINT ( 'NONE',  ( 4.243569643749999010, 10.67187500061451644, 27.54997392385601174 ) ) ;
#46475 = CARTESIAN_POINT ( 'NONE',  ( 19.23750000122903714, 4.330127018922191873, 2.499999999999999556 ) ) ;
#46476 = CARTESIAN_POINT ( 'NONE',  ( 14.09062500061451750, -3.027376345333614438, 5.243569643749998122 ) ) ;
#46477 = ORIENTED_EDGE ( 'NONE', *, *, #60294, .F. ) ;
#46478 = ORIENTED_EDGE ( 'NONE', *, *, #40515, .T. ) ;
#46479 = CARTESIAN_POINT ( 'NONE',  ( 17.25000000000000000, 4.330127018922192761, -2.499999999999997780 ) ) ;
#46480 = CARTESIAN_POINT ( 'NONE',  ( 6.375000000000001776, 6.123233995736764310E-16, -4.999999999999998224 ) ) ;
#46481 = CARTESIAN_POINT ( 'NONE',  ( 0.2791130135581313398, 5.000000000000001776, 25.99999999999999645 ) ) ;
#46482 = CARTESIAN_POINT ( 'NONE',  ( 14.21250000122903323, 4.330127018922192761, -2.499999999999997780 ) ) ;
#46483 = CARTESIAN_POINT ( 'NONE',  ( 27.19687500061451857, -3.027376345333614438, 5.243569643749998122 ) ) ;
#46484 = CARTESIAN_POINT ( 'NONE',  ( 19.56562500061451715, -6.054752690667223547, -1.112240025338166033E-15 ) ) ;
#46485 = CARTESIAN_POINT ( 'NONE',  ( 22.22812500061451502, -4.541064518000419881, 2.621784821874995952 ) ) ;
#46486 = CARTESIAN_POINT ( 'NONE',  ( 4.415625000614518569, 3.027376345333613106, -5.243569643749998122 ) ) ;
#46487 = CARTESIAN_POINT ( 'NONE',  ( 26.81250000000000000, 2.886751345948126879, 4.999999999999999112 ) ) ;
#46488 = DIRECTION ( 'NONE',  ( -0.000000000000000000, -1.000000000000000000, -0.000000000000000000 ) ) ;
#46489 = CARTESIAN_POINT ( 'NONE',  ( 9.871875000614517504, 2.746126346562645981, -4.756430356249997438 ) ) ;
#46490 = CARTESIAN_POINT ( 'NONE',  ( 6.412500001229036073, -4.330127018922190985, -2.500000000000001332 ) ) ;
#46491 = CARTESIAN_POINT ( 'NONE',  ( 20.30625000122903145, -4.330127018922190985, -2.500000000000001332 ) ) ;
#46492 = CARTESIAN_POINT ( 'NONE',  ( -2.121784821874999949, 16.18437500061451573, -33.67503911421598417 ) ) ;
#46493 = CARTESIAN_POINT ( 'NONE',  ( 6.525000001229033231, 2.886751345948129099, -4.999999999999998224 ) ) ;
#46494 = CARTESIAN_POINT ( 'NONE',  ( 6.862500000000002487, 2.886751345948129099, -4.999999999999998224 ) ) ;
#46495 =( BOUNDED_CURVE ( )  B_SPLINE_CURVE ( 2, ( #33780, #56673, #62222, #4989, #15688, #34135, #6071 ),
 .UNSPECIFIED., .F., .F. ) 
 B_SPLINE_CURVE_WITH_KNOTS ( ( 3, 2, 2, 3 ),
 ( 0.6999999999999999556, 0.7027777777777777235, 0.7055555555555557135, 0.7083333333333334814 ),
 .UNSPECIFIED. ) 
 CURVE ( )  GEOMETRIC_REPRESENTATION_ITEM ( )  RATIONAL_B_SPLINE_CURVE ( ( 1.000000000000000000, 0.8660254037844387076, 1.000000000000000000, 0.8660254037844387076, 1.000000000000000000, 0.8660254037844333785, 1.000000000000005329 ) ) 
 REPRESENTATION_ITEM ( '' )  );
#46496 = CARTESIAN_POINT ( 'NONE',  ( 4.162500001229033408, -4.330127018922190985, -2.500000000000001332 ) ) ;
#46497 = CARTESIAN_POINT ( 'NONE',  ( 10.54687500061451644, -3.027376345333614438, 5.243569643749998122 ) ) ;
#46498 = CARTESIAN_POINT ( 'NONE',  ( 28.90312500061451217, 0.000000000000000000, 5.243569643749999010 ) ) ;
#46499 = CYLINDRICAL_SURFACE ( 'NONE', #848, 4.000000000000000000 ) ;
#46500 = CARTESIAN_POINT ( 'NONE',  ( -5.959432963256016791, 8.030867404579453250, -29.19699834589561149 ) ) ;
#46501 = CARTESIAN_POINT ( 'NONE',  ( 9.525000000000002132, 6.123233995736764310E-16, -4.999999999999998224 ) ) ;
#46502 = CARTESIAN_POINT ( 'NONE',  ( 8.184375000614515727, 4.541064518000418104, 2.621784821874999949 ) ) ;
#46503 = CARTESIAN_POINT ( 'NONE',  ( 10.73437500061451644, 6.421520780324663323E-16, -5.243569643749999010 ) ) ;
#46504 = CARTESIAN_POINT ( 'NONE',  ( 6.637500000000001066, -2.886751345948129988, 4.999999999999997335 ) ) ;
#46505 = CARTESIAN_POINT ( 'NONE',  ( -4.243569643749999898, 14.36562500061459424, 27.54997392385601529 ) ) ;
#46506 = CARTESIAN_POINT ( 'NONE',  ( 7.320879633048903241E-15, 18.08749999999999858, 26.00000000000000355 ) ) ;
#46507 = CARTESIAN_POINT ( 'NONE',  ( 6.787500000000001421, -2.886751345948125991, -5.000000000000000000 ) ) ;
#46508 = CARTESIAN_POINT ( 'NONE',  ( 27.75000000122903288, 5.773502691896255534, 3.535250795749688894E-16 ) ) ;
#46509 = CARTESIAN_POINT ( 'NONE',  ( 17.55937500061451573, 2.746126346562643317, 4.756430356249998326 ) ) ;
#46510 = CARTESIAN_POINT ( 'NONE',  ( 23.39062500061451289, 6.054752690667223547, 3.707466751127219781E-16 ) ) ;
#46511 = CARTESIAN_POINT ( 'NONE',  ( 13.52812500061451750, 4.541064518000418104, 2.621784821874999949 ) ) ;
#46512 = CARTESIAN_POINT ( 'NONE',  ( 26.25937500061451502, -5.492252693125287522, -1.008910452111647106E-15 ) ) ;
#46513 = CARTESIAN_POINT ( 'NONE',  ( 8.934375000614517504, 6.421520780324663323E-16, -5.243569643749999010 ) ) ;
#46514 = CARTESIAN_POINT ( 'NONE',  ( 28.53749999999999787, 5.773502691896255534, 3.535250795749688894E-16 ) ) ;
#46515 = CARTESIAN_POINT ( 'NONE',  ( 22.27500000122903145, 2.886751345948129099, -4.999999999999998224 ) ) ;
#46516 = CARTESIAN_POINT ( 'NONE',  ( 11.40000000122903501, -2.886751345948126435, -5.000000000000000000 ) ) ;
#46517 = CARTESIAN_POINT ( 'NONE',  ( 11.85937500061451644, 0.000000000000000000, 5.243569643749999010 ) ) ;
#46518 = CARTESIAN_POINT ( 'NONE',  ( 25.92187500061451999, -6.054752690667223547, -1.112240025338166033E-15 ) ) ;
#46519 = CARTESIAN_POINT ( 'NONE',  ( 2.859375000614519546, 0.000000000000000000, 5.243569643749999010 ) ) ;
#46520 = FACE_OUTER_BOUND ( 'NONE', #13203, .T. ) ;
#46521 = CARTESIAN_POINT ( 'NONE',  ( 22.80937500061451573, -4.541064518000417216, -2.621784821875001281 ) ) ;
#46522 = CARTESIAN_POINT ( 'NONE',  ( 14.63437500061451679, -4.541064518000419881, 2.621784821874995952 ) ) ;
#46523 = CARTESIAN_POINT ( 'NONE',  ( 1.878215178124997609, 18.07812499938548356, 33.25316411605952993 ) ) ;
#46524 = CARTESIAN_POINT ( 'NONE',  ( 26.21249999999999858, 2.886751345948129099, -4.999999999999998224 ) ) ;
#46525 = CARTESIAN_POINT ( 'NONE',  ( 2.000000000000000444, 13.02500000000000036, 26.53589838486224650 ) ) ;
#46526 = CARTESIAN_POINT ( 'NONE',  ( -2.121784821874996840, 14.98437500061451644, -26.32496088578401583 ) ) ;
#46527 = CARTESIAN_POINT ( 'NONE',  ( 26.97187500061451360, 2.746126346562645981, -4.756430356249997438 ) ) ;
#46528 = CARTESIAN_POINT ( 'NONE',  ( 17.46562500061451217, 3.027376345333613106, -5.243569643749998122 ) ) ;
#46529 = CARTESIAN_POINT ( 'NONE',  ( 6.675000000000000711, -4.330127018922194537, 2.499999999999995559 ) ) ;
#46530 = CARTESIAN_POINT ( 'NONE',  ( -2.000000000000001776, 18.19999999999999929, 33.46410161513775705 ) ) ;
#46531 = CARTESIAN_POINT ( 'NONE',  ( 14.47499999999999964, 6.123233995736764310E-16, -4.999999999999998224 ) ) ;
#46532 = CARTESIAN_POINT ( 'NONE',  ( 1.999999999999998668, 19.51250000122903216, 26.53589838486224650 ) ) ;
#46533 = CARTESIAN_POINT ( 'NONE',  ( 14.36250000122903359, 0.000000000000000000, 4.999999999999998224 ) ) ;
#46534 = CARTESIAN_POINT ( 'NONE',  ( 24.38437500061451502, 4.541064518000418104, 2.621784821874999949 ) ) ;
#46535 = VERTEX_POINT ( 'NONE', #21657 ) ;
#46536 = CARTESIAN_POINT ( 'NONE',  ( 19.19062500061452070, -3.027376345333610441, -5.243569643749999898 ) ) ;
#46537 = CARTESIAN_POINT ( 'NONE',  ( 20.03437500061451715, -4.541064518000419881, 2.621784821874995952 ) ) ;
#46538 = CARTESIAN_POINT ( 'NONE',  ( 4.687500000000000000, 5.773502691896255534, 3.535250795749688894E-16 ) ) ;
#46539 = CARTESIAN_POINT ( 'NONE',  ( 8.128125000614515372, 4.541064518000418104, 2.621784821874999949 ) ) ;
#46540 = CARTESIAN_POINT ( 'NONE',  ( 21.66562500061451502, 3.027376345333611329, 5.243569643749999010 ) ) ;
#46541 = CARTESIAN_POINT ( 'NONE',  ( 12.19687500061451679, 6.054752690667223547, 3.707466751127219781E-16 ) ) ;
#46542 = EDGE_CURVE ( 'NONE', #49922, #19257, #10938, .T. ) ;
#46543 = CARTESIAN_POINT ( 'NONE',  ( 16.20937500061451786, 4.541064518000418104, -2.621784821874998173 ) ) ;
#46544 = CARTESIAN_POINT ( 'NONE',  ( 9.001249775931846008E-16, 15.41562500061451679, 34.90005215228797653 ) ) ;
#46545 = CARTESIAN_POINT ( 'NONE',  ( 19.95000000122903572, -2.886751345948125991, -5.000000000000000000 ) ) ;
#46546 = CARTESIAN_POINT ( 'NONE',  ( 13.95937500061451786, 4.119189519843966529, -2.378215178124998275 ) ) ;
#46547 = CARTESIAN_POINT ( 'NONE',  ( 10.45312500061451644, 0.000000000000000000, 5.243569643749999010 ) ) ;
#46548 = CARTESIAN_POINT ( 'NONE',  ( 13.64999999999999858, 4.330127018922192761, -2.499999999999997780 ) ) ;
#46549 = CARTESIAN_POINT ( 'NONE',  ( 29.24062500061451431, 6.054752690667223547, 3.707466751127219781E-16 ) ) ;
#46550 = CARTESIAN_POINT ( 'NONE',  ( 25.05937500061451573, -4.541064518000417216, -2.621784821875001281 ) ) ;
#46551 = CARTESIAN_POINT ( 'NONE',  ( 16.64062500061451289, 6.054752690667223547, 3.707466751127219781E-16 ) ) ;
#46552 = CARTESIAN_POINT ( 'NONE',  ( 27.15000000122902790, -2.886751345948125991, -5.000000000000000000 ) ) ;
#46553 = CARTESIAN_POINT ( 'NONE',  ( 25.37812500061451715, -4.541064518000419881, 2.621784821874995952 ) ) ;
#46554 = CARTESIAN_POINT ( 'NONE',  ( 22.02187500061452141, 3.027376345333613106, -5.243569643749998122 ) ) ;
#46555 = CARTESIAN_POINT ( 'NONE',  ( 16.75312500061451715, 0.000000000000000000, 5.243569643749999010 ) ) ;
#46556 = CARTESIAN_POINT ( 'NONE',  ( 2.121784821875001281, 16.85937500061451999, 33.67503911421598417 ) ) ;
#46557 = CARTESIAN_POINT ( 'NONE',  ( 23.39062500061451289, 6.054752690667223547, 3.707466751127219781E-16 ) ) ;
#46558 = CARTESIAN_POINT ( 'NONE',  ( 3.000000001229032875, 5.773502691896255534, 3.535250795749688894E-16 ) ) ;
#46559 = ORIENTED_EDGE ( 'NONE', *, *, #36894, .T. ) ;
#46560 = CARTESIAN_POINT ( 'NONE',  ( 25.27499999999999858, 6.123233995736764310E-16, -4.999999999999998224 ) ) ;
#46561 = CARTESIAN_POINT ( 'NONE',  ( -3.999999999999999556, 12.76250000000000284, -32.30940107675850470 ) ) ;
#46562 = CARTESIAN_POINT ( 'NONE',  ( 2.655984681222220721E-16, 20.51562499938548356, 25.66244784525396483 ) ) ;
#46563 = CARTESIAN_POINT ( 'NONE',  ( 29.65312500061451573, 4.541064518000418104, -2.621784821874998173 ) ) ;
#46564 = CARTESIAN_POINT ( 'NONE',  ( 9.440625000614517148, 6.054752690667223547, 3.707466751127219781E-16 ) ) ;
#46565 = CARTESIAN_POINT ( 'NONE',  ( 21.78750000122903074, 6.123233995736764310E-16, -4.999999999999998224 ) ) ;
#46566 = CARTESIAN_POINT ( 'NONE',  ( 27.81562500061452070, 3.027376345333613106, -5.243569643749998122 ) ) ;
#46567 = CARTESIAN_POINT ( 'NONE',  ( 25.72499999999999787, 6.123233995736764310E-16, -4.999999999999998224 ) ) ;
#46568 = CARTESIAN_POINT ( 'NONE',  ( -3.999999999999999556, 16.92500000122903359, -32.30940107675850470 ) ) ;
#46569 = CARTESIAN_POINT ( 'NONE',  ( 29.24062500061451431, 6.054752690667223547, 3.707466751127219781E-16 ) ) ;
#46570 = CARTESIAN_POINT ( 'NONE',  ( 9.403125000614517504, 4.541064518000418104, -2.621784821874998173 ) ) ;
#46571 = VERTEX_POINT ( 'NONE', #48289 ) ;
#46572 = CARTESIAN_POINT ( 'NONE',  ( 26.69062500061451715, -3.027376345333614438, 5.243569643749998122 ) ) ;
#46573 = CARTESIAN_POINT ( 'NONE',  ( 8.390625000614518214, -3.027376345333610441, -5.243569643749999898 ) ) ;
#46574 = AXIS2_PLACEMENT_3D ( 'NONE', #7591, #13126, #7958 ) ;
#46575 = CARTESIAN_POINT ( 'NONE',  ( 4.115625000614516082, 3.027376345333611329, 5.243569643749999010 ) ) ;
#46576 = CARTESIAN_POINT ( 'NONE',  ( 15.34687500061451537, 5.492252693125287522, 3.363034840372157021E-16 ) ) ;
#46577 = DIRECTION ( 'NONE',  ( -1.000000000000000000, -0.000000000000000000, -0.000000000000000000 ) ) ;
#46578 = AXIS2_PLACEMENT_3D ( 'NONE', #1533, #35494, #70205 ) ;
#46579 = CARTESIAN_POINT ( 'NONE',  ( 13.12500000000000178, 6.123233995736764310E-16, -4.999999999999998224 ) ) ;
#46580 = EDGE_CURVE ( 'NONE', #21751, #67801, #15384, .T. ) ;
#46581 = CARTESIAN_POINT ( 'NONE',  ( 13.69687500061451679, -3.027376345333614438, 5.243569643749998122 ) ) ;
#46582 = CARTESIAN_POINT ( 'NONE',  ( 10.50000000122903465, -2.886751345948125991, -5.000000000000000000 ) ) ;
#46583 = CARTESIAN_POINT ( 'NONE',  ( 16.58437500061451786, 6.421520780324663323E-16, -5.243569643749999010 ) ) ;
#46584 = CARTESIAN_POINT ( 'NONE',  ( 18.48750000000000071, -2.886751345948125991, -5.000000000000000000 ) ) ;
#46585 = B_SPLINE_CURVE_WITH_KNOTS ( 'NONE', 3,
 ( #3961, #26484, #4333, #30920, #65265, #15024, #20553, #9494, #53461, #3594 ),
 .UNSPECIFIED., .F., .F.,
 ( 4, 3, 3, 4 ),
 ( 1.332339343076284724E-16, 7.861290946297937144E-05, 0.0001572256709461994102, 0.0002973492893351208869 ),
 .UNSPECIFIED. ) ;
#46586 = CARTESIAN_POINT ( 'NONE',  ( 7.959375000614516971, -4.541064518000417216, -2.621784821875001281 ) ) ;
#46587 = CARTESIAN_POINT ( 'NONE',  ( -2.121784821874999949, 11.17812500061451786, -33.67503911421598417 ) ) ;
#46588 = CARTESIAN_POINT ( 'NONE',  ( 1.626862140677534273E-15, 16.51249999999999929, 34.00000000000000000 ) ) ;
#46589 = CARTESIAN_POINT ( 'NONE',  ( 23.33437500061451786, 5.492252693125287522, 3.363034840372157021E-16 ) ) ;
#46590 = CARTESIAN_POINT ( 'NONE',  ( 30.00000000000000000, 0.000000000000000000, 0.000000000000000000 ) ) ;
#46591 = CARTESIAN_POINT ( 'NONE',  ( 24.81562500061451715, 3.027376345333611329, 5.243569643749999010 ) ) ;
#46592 = CARTESIAN_POINT ( 'NONE',  ( 1.999999999999997335, 20.46874999877096712, 33.46410161513775705 ) ) ;
#46593 = CARTESIAN_POINT ( 'NONE',  ( 28.35937500061451289, 4.541064518000418104, -2.621784821874998173 ) ) ;
#46594 = CARTESIAN_POINT ( 'NONE',  ( 24.48749999999999716, 5.773502691896255534, 3.535250795749688894E-16 ) ) ;
#46595 = CARTESIAN_POINT ( 'NONE',  ( 7.790625000614518569, -3.027376345333614438, 5.243569643749998122 ) ) ;
#46596 = CARTESIAN_POINT ( 'NONE',  ( 24.12187500061451573, 5.824947211148865298E-16, -4.756430356249998326 ) ) ;
#46597 = CARTESIAN_POINT ( 'NONE',  ( 19.02187500061451786, 3.027376345333611329, 5.243569643749999010 ) ) ;
#46598 = CARTESIAN_POINT ( 'NONE',  ( 10.20937500061451431, 2.746126346562645981, -4.756430356249997438 ) ) ;
#46599 = CARTESIAN_POINT ( 'NONE',  ( 2.803125000614518747, 0.000000000000000000, 5.243569643749999010 ) ) ;
#46600 = CARTESIAN_POINT ( 'NONE',  ( 9.309375000614517504, -4.541064518000417216, -2.621784821875001281 ) ) ;
#46601 = ORIENTED_EDGE ( 'NONE', *, *, #27024, .F. ) ;
#46602 = CARTESIAN_POINT ( 'NONE',  ( 18.08437500061451431, 4.541064518000418104, 2.621784821874999949 ) ) ;
#46603 = CARTESIAN_POINT ( 'NONE',  ( 27.52500000000000213, 6.123233995736764310E-16, -4.999999999999998224 ) ) ;
#46604 = CARTESIAN_POINT ( 'NONE',  ( 29.48437500061451644, -4.541064518000419881, 2.621784821874995952 ) ) ;
#46605 = CARTESIAN_POINT ( 'NONE',  ( 34.99999999999999289, 9.426999614876460059E-14, 9.000000000000000000 ) ) ;
#46606 = CARTESIAN_POINT ( 'NONE',  ( 17.73750000000000071, 5.773502691896255534, 3.535250795749688401E-16 ) ) ;
#46607 = VERTEX_POINT ( 'NONE', #65634 ) ;
#46608 = CARTESIAN_POINT ( 'NONE',  ( 10.95000000000000107, 4.330127018922192761, -2.499999999999997780 ) ) ;
#46609 = CARTESIAN_POINT ( 'NONE',  ( 10.92187500061451644, -4.119189519843968306, 2.378215178124996054 ) ) ;
#46610 = CARTESIAN_POINT ( 'NONE',  ( 23.91562500061451502, 3.027376345333611329, 5.243569643749999010 ) ) ;
#46611 = CARTESIAN_POINT ( 'NONE',  ( 14.51250000000000107, 2.886751345948129099, -4.999999999999998224 ) ) ;
#46612 = CARTESIAN_POINT ( 'NONE',  ( 9.037500001229034297, -4.330127018922194537, 2.499999999999995559 ) ) ;
#46613 = CARTESIAN_POINT ( 'NONE',  ( 6.215625000614517504, 3.027376345333613106, -5.243569643749998122 ) ) ;
#46614 = CARTESIAN_POINT ( 'NONE',  ( 21.18749999999999645, -2.886751345948125991, -5.000000000000000000 ) ) ;
#46615 = CARTESIAN_POINT ( 'NONE',  ( 19.71562500061451928, 3.027376345333613106, -5.243569643749998122 ) ) ;
#46616 = CARTESIAN_POINT ( 'NONE',  ( 0.000000000000000000, -4.999999999999999112, 0.000000000000000000 ) ) ;
#46617 = CARTESIAN_POINT ( 'NONE',  ( 25.08750000122903145, 4.330127018922191873, 2.499999999999999556 ) ) ;
#46618 = CARTESIAN_POINT ( 'NONE',  ( -7.967954043666661671E-16, 17.92812499938548498, 34.33755215474603517 ) ) ;
#46619 = CARTESIAN_POINT ( 'NONE',  ( 5.512499999999999289, 2.886751345948129099, -4.999999999999998224 ) ) ;
#46620 = AXIS2_PLACEMENT_3D ( 'NONE', #45655, #39755, #57794 ) ;
#46621 = ORIENTED_EDGE ( 'NONE', *, *, #793, .T. ) ;
#46622 = CARTESIAN_POINT ( 'NONE',  ( 22.60312500061451857, 0.000000000000000000, 5.243569643749999010 ) ) ;
#46623 = CARTESIAN_POINT ( 'NONE',  ( 25.60312500061451502, 4.541064518000418104, -2.621784821874998173 ) ) ;
#46624 = CARTESIAN_POINT ( 'NONE',  ( 27.87187500061451573, 3.027376345333613106, -5.243569643749998122 ) ) ;
#46625 = CARTESIAN_POINT ( 'NONE',  ( 15.29062500061451679, 6.054752690667223547, 3.707466751127219781E-16 ) ) ;
#46626 = CARTESIAN_POINT ( 'NONE',  ( 12.05625000122903145, 0.000000000000000000, 4.999999999999998224 ) ) ;
#46627 = AXIS2_PLACEMENT_3D ( 'NONE', #65137, #14163, #2011 ) ;
#46628 = CARTESIAN_POINT ( 'NONE',  ( 26.73750000122903003, 6.123233995736764310E-16, -4.999999999999998224 ) ) ;
#46629 = CARTESIAN_POINT ( 'NONE',  ( 21.34687500061451715, -2.746126346562646425, 4.756430356249996549 ) ) ;
#46630 = CARTESIAN_POINT ( 'NONE',  ( 15.55312500061451608, -4.541064518000417216, -2.621784821875001281 ) ) ;
#46631 = CARTESIAN_POINT ( 'NONE',  ( -3.999999999999999112, 16.85000000000000142, -30.00000000000000000 ) ) ;
#46632 = CARTESIAN_POINT ( 'NONE',  ( 4.237500001229036251, 6.123233995736764310E-16, -4.999999999999998224 ) ) ;
#46633 = CARTESIAN_POINT ( 'NONE',  ( 9.234375000614518214, -4.541064518000419881, 2.621784821874995952 ) ) ;
#46634 = CARTESIAN_POINT ( 'NONE',  ( 10.99687500061451750, -3.027376345333614438, 5.243569643749998122 ) ) ;
#46635 = CARTESIAN_POINT ( 'NONE',  ( 20.89687500061452141, -3.027376345333614438, 5.243569643749998122 ) ) ;
#46636 = ORIENTED_EDGE ( 'NONE', *, *, #18362, .T. ) ;
#46637 = CARTESIAN_POINT ( 'NONE',  ( -0.4074127065224521504, 10.00000000000000178, 24.00000000000001066 ) ) ;
#46638 = CARTESIAN_POINT ( 'NONE',  ( 23.20312500061451644, -4.541064518000417216, -2.621784821875001281 ) ) ;
#46639 = VECTOR ( 'NONE', #16426, 1000.000000000000000 ) ;
#46640 = CARTESIAN_POINT ( 'NONE',  ( 18.27187500061451431, -6.054752690667223547, -1.112240025338166033E-15 ) ) ;
#46641 = CARTESIAN_POINT ( 'NONE',  ( 25.34062500061451217, -3.027376345333614438, 5.243569643749998122 ) ) ;
#46642 = CARTESIAN_POINT ( 'NONE',  ( 9.712500001229033231, 4.330127018922192761, -2.499999999999997780 ) ) ;
#46643 = CARTESIAN_POINT ( 'NONE',  ( -2.828200636599751609E-16, 14.48750000000000071, 25.38119784648299770 ) ) ;
#46644 = CARTESIAN_POINT ( 'NONE',  ( 29.20312500061451644, 4.541064518000418104, -2.621784821874998173 ) ) ;
#46645 = CARTESIAN_POINT ( 'NONE',  ( 8.887500001229033941, 4.330127018922191873, 2.499999999999999556 ) ) ;
#46646 = VECTOR ( 'NONE', #34297, 1000.000000000000000 ) ;
#46647 = CARTESIAN_POINT ( 'NONE',  ( 4.575000001229033941, -5.773502691896255534, -1.060575238724906372E-15 ) ) ;
#46648 = CARTESIAN_POINT ( 'NONE',  ( 1.999999999999998668, 19.84999999999999787, -33.46410161513775705 ) ) ;
#46649 = CARTESIAN_POINT ( 'NONE',  ( 27.71250000122903145, 4.330127018922192761, -2.499999999999997780 ) ) ;
#46650 = CARTESIAN_POINT ( 'NONE',  ( -3.756430356250000102, 13.87812499938548250, 30.00000000000000000 ) ) ;
#46651 = CARTESIAN_POINT ( 'NONE',  ( 9.496875000614517504, 6.054752690667223547, 3.707466751127219781E-16 ) ) ;
#46652 = CARTESIAN_POINT ( 'NONE',  ( 24.41250000000000142, 2.886751345948162850, -4.999999999999940492 ) ) ;
#46653 = CARTESIAN_POINT ( 'NONE',  ( 16.71562500061451573, 3.027376345333611329, 5.243569643749999010 ) ) ;
#46654 = CARTESIAN_POINT ( 'NONE',  ( 9.984375000614518214, 4.541064518000418104, 2.621784821874999949 ) ) ;
#46655 = CARTESIAN_POINT ( 'NONE',  ( 29.55000000122903003, 5.773502691896255534, 3.535250795749688894E-16 ) ) ;
#46656 = CARTESIAN_POINT ( 'NONE',  ( 18.79687500061451644, -3.027376345333610441, -5.243569643749999898 ) ) ;
#46657 = CARTESIAN_POINT ( 'NONE',  ( 7.284375000614518036, 4.541064518000418104, 2.621784821874999949 ) ) ;
#46658 = CARTESIAN_POINT ( 'NONE',  ( 3.033819321519781287, -3.974438763815245856, -3.388311280553572669 ) ) ;
#46659 = LINE ( 'NONE', #69199, #39210 ) ;
#46660 =( BOUNDED_CURVE ( )  B_SPLINE_CURVE ( 2, ( #40112, #29379, #51912, #1310, #40467, #67822, #23819 ),
 .UNSPECIFIED., .F., .F. ) 
 B_SPLINE_CURVE_WITH_KNOTS ( ( 3, 2, 2, 3 ),
 ( 0.1333333333333333037, 0.1361111111111110716, 0.1388888888888888673, 0.1416666666666666352 ),
 .UNSPECIFIED. ) 
 CURVE ( )  GEOMETRIC_REPRESENTATION_ITEM ( )  RATIONAL_B_SPLINE_CURVE ( ( 1.000000000000001332, 0.8660254037844373753, 1.000000000000000000, 0.8660254037844387076, 1.000000000000000000, 0.8660254037844400399, 0.9999999999999986677 ) ) 
 REPRESENTATION_ITEM ( '' )  );
#46661 = CARTESIAN_POINT ( 'NONE',  ( 8.503125000614515372, 4.541064518000418104, -2.621784821874998173 ) ) ;
#46662 = CARTESIAN_POINT ( 'NONE',  ( 17.20312500061451644, 0.000000000000000000, 5.243569643749999010 ) ) ;
#46663 = ORIENTED_EDGE ( 'NONE', *, *, #64920, .T. ) ;
#46664 = CARTESIAN_POINT ( 'NONE',  ( 5.025000001229035895, -5.773502691896255534, -1.060575238724906372E-15 ) ) ;
#46665 = CARTESIAN_POINT ( 'NONE',  ( 15.59062500061451573, -3.027376345333610441, -5.243569643749999898 ) ) ;
#46666 = CARTESIAN_POINT ( 'NONE',  ( 14.27812500061451573, 6.421520780324663323E-16, -5.243569643749999010 ) ) ;
#46667 = CARTESIAN_POINT ( 'NONE',  ( 22.95937500061451431, 4.119189519843966529, -2.378215178124998275 ) ) ;
#46668 = CARTESIAN_POINT ( 'NONE',  ( 12.56250000000000178, -5.773502691896255534, -1.060575238724906372E-15 ) ) ;
#46669 = CARTESIAN_POINT ( 'NONE',  ( 7.312500001229033764, -4.330127018922190985, -2.500000000000001332 ) ) ;
#46670 = CARTESIAN_POINT ( 'NONE',  ( 29.09999999999999787, 0.000000000000000000, 4.999999999999998224 ) ) ;
#46671 = EDGE_CURVE ( 'NONE', #29206, #52162, #51054, .T. ) ;
#46672 = CARTESIAN_POINT ( 'NONE',  ( 14.93437500061451750, 4.541064518000418104, 2.621784821874999949 ) ) ;
#46673 = CARTESIAN_POINT ( 'NONE',  ( 18.41250000122903430, 0.000000000000000000, 4.999999999999998224 ) ) ;
#46674 = CARTESIAN_POINT ( 'NONE',  ( 24.86250000000000071, 2.886751345948129099, -4.999999999999998224 ) ) ;
#46675 = CARTESIAN_POINT ( 'NONE',  ( -1.473776270879187500, 9.872922227264545825, -34.04916702557058983 ) ) ;
#46676 = CYLINDRICAL_SURFACE ( 'NONE', #22937, 4.000000000000000000 ) ;
#46677 = CARTESIAN_POINT ( 'NONE',  ( 4.267099419464107868, -3.843735374978448860, 3.829594327187515024 ) ) ;
#46678 = CARTESIAN_POINT ( 'NONE',  ( 6.375000000000001776, 6.123233995736764310E-16, -4.999999999999998224 ) ) ;
#46679 = CARTESIAN_POINT ( 'NONE',  ( 24.52499999999999858, 4.330127018922191873, 2.499999999999999556 ) ) ;
#46680 = CARTESIAN_POINT ( 'NONE',  ( 17.82187500061451502, -6.054752690667223547, -1.112240025338166033E-15 ) ) ;
#46681 = CARTESIAN_POINT ( 'NONE',  ( 21.41250000122903074, 4.330127018922192761, -2.499999999999997780 ) ) ;
#46682 = AXIS2_PLACEMENT_3D ( 'NONE', #52954, #30426, #13409 ) ;
#46683 = CARTESIAN_POINT ( 'NONE',  ( 15.25312500061451715, 4.541064518000418104, -2.621784821874998173 ) ) ;
#46684 = CARTESIAN_POINT ( 'NONE',  ( 9.393750001229035362, -2.886751345948129988, 4.999999999999997335 ) ) ;
#46685 = CARTESIAN_POINT ( 'NONE',  ( 22.53750000122903430, -4.330127018922194537, 2.499999999999995559 ) ) ;
#46686 = CARTESIAN_POINT ( 'NONE',  ( 25.69687500061451502, 6.054752690667223547, 3.707466751127219781E-16 ) ) ;
#46687 = CARTESIAN_POINT ( 'NONE',  ( 18.57187500061451857, -4.119189519843968306, 2.378215178124996054 ) ) ;
#46688 = CARTESIAN_POINT ( 'NONE',  ( 10.22812500061451679, 6.421520780324663323E-16, -5.243569643749999010 ) ) ;
#46689 = CIRCLE ( 'NONE', #63192, 5.999999999999998224 ) ;
#46690 = CARTESIAN_POINT ( 'NONE',  ( 16.54687500061451644, -3.027376345333610441, -5.243569643749999898 ) ) ;
#46691 = ORIENTED_EDGE ( 'NONE', *, *, #8082, .F. ) ;
#46692 = CARTESIAN_POINT ( 'NONE',  ( 26.72812500061451502, -4.541064518000419881, 2.621784821874995952 ) ) ;
#46693 = CARTESIAN_POINT ( 'NONE',  ( 20.95312500061451999, -4.541064518000417216, -2.621784821875001281 ) ) ;
#46694 = CARTESIAN_POINT ( 'NONE',  ( 29.57812500061451644, 6.421520780324663323E-16, -5.243569643749999010 ) ) ;
#46695 = CARTESIAN_POINT ( 'NONE',  ( 7.347880794884120722E-16, 20.00000000000000000, -24.00000000000000000 ) ) ;
#46696 =( BOUNDED_SURFACE ( )  B_SPLINE_SURFACE ( 1, 2, ( 
 ( #11625, #28255, #12334, #67425, #40423, #39345, #34141, #45967, #17510, #68500, #50786, #45613, #34869, #33422, #68146, #22694, #45245, #57397, #27528, #44534, #67066, #55963, #40071, #62585, #38981, #61497, #10894, #5358, #27896, #72956, #30051, #2349, #18948, #40793, #29337, #24865, #14151, #30423, #64395, #51867, #36327, #35954, #8252, #13785, #69942, #19312, #47774, #53313, #24140, #41507, #1269, #69586, #41865, #58842, #41155, #52229, #58112, #64027, #47412, #52951, #7163, #69229, #30782, #2712, #13054, #1633, #64761, #46328, #25228, #12697, #52591, #47052, #70310, #68863, #19683, #23776, #42236, #36686, #13406, #6803, #63306, #35234, #46692, #18219, #18590, #35593, #63664, #58475, #7520, #1998, #29692, #57755, #24508, #7887, #44352, #11074, #33602, #66133, #38053, #56146, #21786, #38801, #45064, #39160, #60578, #4091, #32521, #16966, #66877, #5540, #15881, #33246, #32882, #61317, #49157, #66499, #49518, #9986, #27348, #43611, #50606, #71688, #55784, #22517, #67601, #59207, #10714, #49879, #16245, #27711, #5175, #15511, #4815, #8615, #55058, #4459, #50251, #72774, #22158, #44710, #28078, #21060, #10, #38426, #55422, #26989, #60949, #72404, #72043, #21421, #43978, #67246, #10352, #16604, #61675, #32156, #54689, #26620, #18411, #29875, #52411, #18048, #29159, #62405, #62767, #67960, #57583, #22868, #29517, #12158, #33963, #46510, #11443, #45426, #11804, #52052, #69049, #45790, #1095, #69414, #46875, #34321, #730, #57217, #23239, #56853, #6259, #28787, #51328, #28428, #40977, #68325, #39522, #62048, #361, #17685, #24326, #63492, #12880, #35413, #17333, #39892, #57938, #23603, #40606, #56502, #7345, #40246, #5895, #34686, #50965, #46148, #1819, #6630, #12523, #51691, #63127, #68688, #35056, #6986, #1456, #23962, #2175, #9168, #7706, #14337, #54238, #3635, #26159, #70494, #59027, #47966, #59389, #2892, #24688, #36507, #48698, #13599, #19133, #19871, #42424, #64945, #25423, #14696, #52773, #31703, #25051, #13969, #36145, #19501, #8429, #47232, #69765, #41687, #36871, #2531, #30965, #53500, #64581, #3268, #53132, #70859, #18769, #41335, #8799, #31335, #64210, #42058, #58664, #53876, #8072, #25796, #48334, #13236, #20233, #63845, #30604, #47594, #42785, #65306, #70123, #37240, #35774, #58297, #59761, #30240, #15794, #54968, #20971, #43524, #37968, #66046, #60125, #72690, #4374, #27993, #71221, #32068, #60489, #56060, #50160, #21337, #38334, #5091, #37603, #33159, #20599, #10991, #16163, #55335, #22072, #54600, #26528, #15424, #44631, #9895, #26903, #32431, #60863, #49429, #71963, #43892, #65678, #39073, #55697, #4730, #66416, #9534, #67160, #10266, #43158, #15066, #4005, #32799, #5453, #16521, #27264, #49797, #27627, #49068, #61590, #71596, #33511, #38715, #72322, #21702, #44259, #66792, #61235, #10629, #17247, #56769, #39807, #17604, #62323, #34235, #280, #44980, #18320, #34970, #34600, #1368, #23878, #56423, #28343, #46425, #12079, #29073, #35329, #29432, #50880, #67517, #22788, #7261, #57129, #68963, #6173, #23515, #23153, #51608, #39436, #28703, #11719, #45341, #40164, #33878, #40893, #61956, #46065, #12793, #57852, #50522, #1008, #62683, #6539, #17961, #68600, #5812, #68241, #73050, #67875, #51242, #40522, #63038, #12437, #57499, #63407, #11360, #22432, #645, #45707, #6901, #51969, #16882, #63760, #7616, #13149, #8347, #13510, #41972, #70039, #2442, #14248, #64124, #8713, #20146, #42700, #30876, #19412, #52686, #53048, #58211, #47881, #35691, #19786, #24965, #24241, #36787, #1728, #30152, #2092, #42337, #59302, #36057, #64493, #59676, #37151, #24602, #58577, #47510, #7985, #47150, #69682, #19047, #46790, #31245, #41249, #13885, #25336, #36425, #41605, #52326, #70410, #29790, #53417, #53786, #69326, #3182, #58940, #25709, #48246, #64860, #70770, #65222, #14612, #30521, #2808, #18685, #71879, #44176, #66706, #43441, #54516, #60403, #21252, #27179, #55254, #9452, #71511, #61152, #32717, #15343, #3919, #67079, #48612, #10547, #14982, #4650, #31621, #71137, #43067, #26442, #3551, #31982, #48982, #65963, #33076, #72608, #21989, #60775, #43805, #20887, #32344, #37520, #49713, #65593, #72241, #54882, #26073, #16079, #54155, #60041, #37883, #21619, #38628, #9812, #66330, #38995, #16438, #4288, #26814, #49348, #15708, #38246, #10182, #55614, #5010, #20510, #27544, #50076, #9084, #44548, #22353, #50801, #46344, #40439, #11642, #28625, #68518, #27912, #23436, #10908, #1283, #6456, #45628, #62955, #44905, #16804, #56346, #34885, #28270, #67794, #204, #51163, #22710, #45262, #11282, #55979, #29352, #45982, #68162, #12350, #57413, #67443, #39360, #6818, #23073, #40087, #68878, #51885, #61875, #5373, #33434, #18235, #33802, #50446, #72971, #5736, #23793, #17168, #39727, #62245, #34157, #56694, #62601, #6094, #61510, #51528, #17525, #566, #11997, #34520, #57050, #28991, #928, #17879, #35608, #30438, #30798, #63323, #70684, #19327, #41523, #30068, #14165, #2363, #58128, #52967, #7901, #18963, #3093, #7535, #31158, #52606, #24881, #70322, #53330, #19698, #24523, #58857, #36699, #46709, #13803, #64042, #69602, #25622, #25243, #47792, #7179, #69244, #8267, #2728, #47426, #13421, #59221, #12713, #42251, #52245, #35971, #36342, #69957, #1648, #35248, #64775, #48159, #64410, #8629, #57769, #53700, #41882, #40808, #29707, #24156, #18605, #41171, #63679, #2012, #13069, #47067, #58491, #55169, #4565, #54435, #65510, #71424, #9728, #38162, #66242, #20430, #9366, #72154, #43719, #26355, #14897, #4925, #59589, #21533, #25989, #15620, #42615, #9001, #54073, #37438, #3469, #60685, #10100, #32629, #27095, #44088, #32991, #31533, #21166, #48528, #49627, #38540, #66615, #15991, #71055, #42979, #27460, #59959, #3834, #37798, #48894, #31899, #20801, #43356, #65879, #15260, #61064, #60318 ),
 ( #32262, #10461, #55531, #49991, #54794, #20059, #65139, #4201, #14530, #26729, #49264, #37064, #71797, #56962, #38908, #5282, #17440, #11909, #62157, #22624, #17791, #44460, #839, #10820, #45175, #68071, #11554, #33355, #21904, #39997, #6733, #22980, #6366, #66991, #28898, #28540, #23348, #51437, #62511, #34434, #40351, #45897, #16718, #34070, #16353, #56610, #68428, #62870, #33716, #44820, #50716, #6005, #12266, #45542, #72887, #61785, #34796, #57329, #5652, #67355, #29267, #61427, #72515, #27828, #55893, #50360, #22268, #39273, #11189, #56261, #28187, #119, #67706, #17078, #39639, #51075, #472, #52881, #63235, #36255, #70235, #19238, #13713, #12629, #35164, #36615, #1200, #59136, #29622, #40718, #68795, #23705, #14076, #57688, #7093, #52159, #46256, #69873, #8544, #2279, #58770, #18151, #8179, #7817, #53240, #30707, #41793, #64321, #19608, #25157, #69161, #63958, #1562, #41440, #2638, #47698, #12987, #24072, #29979, #13342, #42165, #24796, #46617, #41085, #64691, #47339, #58044, #18520, #51797, #63597, #35523, #7452, #52520, #1929, #24434, #46983, #69519, #18877, #35879, #58404, #30352, #49180, #32543, #44000, #70602, #32179, #42528, #15533, #49542, #71710, #66156, #65054, #14445, #15902, #53612, #38449, #8914, #19975, #48074, #3003, #66523, #36979, #59501, #31445, #25532, #37352, #54712, #3745, #55081, #21082, #15172, #53986, #3383, #25905, #48445, #70969, #20344, #59874, #42895, #20711, #43633, #65419, #60975, #9645, #31813, #14808, #4481, #65791, #9279, #43270, #71336, #54352, #31072, #26270, #21444, #48807, #37710, #60599, #38077, #10008, #60231, #27010, #72064, #4115, #26643, #33626, #39184, #69346, #67983, #17358, #49903, #16269, #28452, #22892, #34, #56170, #28812, #55444, #11827, #21811, #5564, #5918, #22540, #44375, #38825, #50987, #45450, #45088, #28101, #51350, #4837, #34345, #66901, #50629, #385, #67623, #61340, #32907, #39915, #18704, #33988, #62429, #27371, #56878, #39547, #6282, #1748, #24260, #46809, #41268, #10375, #27736, #16989, #72427, #62071, #10736, #33269, #44736, #55807, #61699, #11465, #5195, #56525, #50275, #72799, #22182, #67270, #16629, #11098, #48631, #30174, #65241, #69701, #59321, #13169, #52705, #24622, #58598, #47169, #14268, #8731, #31265, #53807, #14630, #3570, #2111, #64880, #19067, #48267, #9103, #3201, #25729, #41624, #64143, #71156, #35709, #20528, #13530, #36077, #7636, #58231, #26093, #8005, #30540, #53067, #2462, #70058, #36806, #36445, #37170, #70791, #47902, #24985, #47530, #19432, #41993, #64513, #13906, #58959, #8367, #53438, #20166, #30895, #63780, #42358, #2828, #25356, #59696, #70430, #19805, #42720, #31641, #54173, #72624, #43459, #50093, #65982, #66348, #38645, #72258, #61169, #9833, #49731, #5025, #3938, #27196, #49367, #54900, #22008, #66724, #16096, #60060, #10199, #60793, #55631, #54536, #27562, #4308, #71897, #15362, #26833, #21270, #26461, #49000, #71531, #32734, #32363, #21635, #43824, #10564, #15726, #38265, #33092, #44564, #67094, #55271, #4666, #20906, #44193, #37904, #43085, #60422, #65612, #15001, #9471, #37538, #32001, #41359, #57960, #64235, #13259, #62163, #11560, #17084, #125, #35436, #30265, #1844, #53158, #19157, #35797, #6011, #50722, #22630, #1480, #23986, #34076, #7368, #46533, #18795, #41711, #45181, #59052, #7731, #29899, #18434, #2556, #63869, #69075, #58320, #69438, #52437, #64607, #41001, #19526, #63516, #52798, #58687, #13626, #8097, #12903, #47257, #25074, #56616, #2199, #24351, #46899, #13993, #36169, #30626, #67712, #28546, #69791, #47617, #24714, #70148, #42085, #39645, #36532, #52074, #28193, #4030, #20626, #42450, #30992, #26555, #15818, #32093, #66071, #53525, #37994, #37627, #9921, #15449, #71624, #20997, #49454, #54994, #25823, #43185, #2919, #71247, #43549, #60515, #42811, #53903, #59788, #65704, #49095, #54624, #32459, #15091, #60150, #66442, #4400, #59418, #25450, #3295, #38361, #9560, #26929, #37266, #71988, #54267, #21362, #70522, #14723, #70885, #31362, #48724, #64972, #43916, #19897, #8457, #47993, #14363, #36898, #8825, #48360, #20259, #65334, #9194, #31729, #26184, #3661, #55723, #61260, #16906, #61982, #39461, #67543, #56794, #21727, #51268, #67186, #56089, #5117, #61616, #5481, #44286, #38740, #66816, #11384, #44656, #33903, #16547, #67900, #28020, #22098, #39833, #670, #23178, #56447, #50548, #10654, #11018, #16189, #5837, #33184, #50905, #33539, #55361, #17272, #32823, #39099, #27651, #50188, #27288, #73076, #22457, #17629, #68267, #72715, #45006, #28369, #304, #22814, #45365, #62348, #11744, #49822, #34261, #6199, #60888, #10293, #28727, #45732, #4755, #72346, #63435, #7290, #47178, #6567, #2121, #62710, #53077, #58241, #24270, #41634, #23542, #68628, #34998, #13540, #6928, #46453, #29458, #29819, #51995, #23905, #63065, #34625, #8015, #24633, #46819, #64153, #36088, #46092, #17990, #68991, #69711, #69357, #1035, #40549, #29099, #12104, #18348, #41279, #12822, #58608, #30184, #18714, #12468, #57156, #51634, #57527, #1396, #40923, #35356, #57880, #52354, #52715, #1757, #70069, #63790, #13180, #35719, #30550, #7646, #19077, #2472, #24996, #47540, #40189, #14278, #9843, #36816, #9113, #49010, #9482, #71541, #3211, #37548, #15373, #25367, #65623, #42730, #48277, #4318, #3948, #26471, #58969, #47911, #60070, #32011, #31651, #65251, #37915, #64523, #20916, #30906, #14640, #15011, #54184, #53448, #42003, #54546, #26843, #43095, #43468, #13916, #65992, #48641, #60432, #32372, #54910, #49377, #19442, #36455, #59331, #3580, #8377, #26103, #2838, #70440, #53818, #64890, #70801, #71166, #19815, #42368, #8742, #31275, #25740, #20176, #37181, #59706, #20539, #38275, #228, #4676, #67465, #21280, #60803, #32744, #66734, #55281, #22377, #16828, #39382, #61901, #22733 ) ),
 .UNSPECIFIED., .F., .F., .F. ) 
 B_SPLINE_SURFACE_WITH_KNOTS ( ( 2, 2 ),
 ( 3, 2, 2, 2, 2, 2, 2, 2, 2, 2, 2, 2, 2, 2, 2, 2, 2, 2, 2, 2, 2, 2, 2, 2, 2, 2, 2, 2, 2, 2, 2, 2, 2, 2, 2, 2, 2, 2, 2, 2, 2, 2, 2, 2, 2, 2, 2, 2, 2, 2, 2, 2, 2, 2, 2, 2, 2, 2, 2, 2, 2, 2, 2, 2, 2, 2, 2, 2, 2, 2, 2, 2, 2, 2, 2, 2, 2, 2, 2, 2, 2, 2, 2, 2, 2, 2, 2, 2, 2, 2, 2, 2, 2, 2, 2, 2, 2, 2, 2, 2, 2, 2, 2, 2, 2, 2, 2, 2, 2, 2, 2, 2, 2, 2, 2, 2, 2, 2, 2, 2, 2, 2, 2, 2, 2, 2, 2, 2, 2, 2, 2, 2, 2, 2, 2, 2, 2, 2, 2, 2, 2, 2, 2, 2, 2, 2, 2, 2, 2, 2, 2, 2, 2, 2, 2, 2, 2, 2, 2, 2, 2, 2, 2, 2, 2, 2, 2, 2, 2, 2, 2, 2, 2, 2, 2, 2, 2, 2, 2, 2, 2, 2, 2, 2, 2, 2, 2, 2, 2, 2, 2, 2, 2, 2, 2, 2, 2, 2, 2, 2, 2, 2, 2, 2, 2, 2, 2, 2, 2, 2, 2, 2, 2, 2, 2, 2, 2, 2, 2, 2, 2, 2, 2, 2, 2, 2, 2, 2, 2, 2, 2, 2, 2, 2, 2, 2, 2, 2, 2, 2, 2, 2, 2, 2, 2, 2, 2, 2, 2, 2, 2, 2, 2, 2, 2, 2, 2, 2, 2, 2, 2, 2, 2, 2, 2, 2, 2, 2, 2, 2, 2, 2, 2, 2, 2, 2, 2, 2, 2, 2, 2, 2, 2, 2, 2, 2, 2, 2, 2, 2, 2, 2, 2, 2, 2, 2, 2, 2, 2, 2, 2, 2, 2, 2, 2, 2, 2, 2, 2, 2, 2, 2, 2, 2, 2, 2, 2, 2, 2, 2, 2, 2, 2, 2, 2, 2, 2, 2, 2, 2, 2, 2, 2, 2, 2, 2, 2, 2, 2, 2, 2, 2, 2, 2, 2, 2, 2, 2, 2, 2, 2, 2, 2, 2, 2, 2, 2, 2, 2, 2, 3 ),
 ( 0.000000000000000000, 1.000000000000000000 ),
 ( 0.000000000000000000, 0.002777777777777777884, 0.005555555555555555768, 0.008333333333333333218, 0.01111111111111111154, 0.01388888888888888812, 0.01666666666666666644, 0.01944444444444444475, 0.02222222222222222307, 0.02500000000000000139, 0.02777777777777777624, 0.03055555555555555455, 0.03333333333333333287, 0.03611111111111110772, 0.03888888888888888951, 0.04166666666666666435, 0.04444444444444444614, 0.04722222222222222099, 0.05000000000000000278, 0.05277777777777777762, 0.05555555555555555247, 0.05833333333333333426, 0.06111111111111110911, 0.06388888888888888395, 0.06666666666666666574, 0.06944444444444444753, 0.07222222222222221544, 0.07499999999999999722, 0.07777777777777777901, 0.08055555555555556080, 0.08333333333333332871, 0.08611111111111111049, 0.08888888888888889228, 0.09166666666666666019, 0.09444444444444444198, 0.09722222222222222376, 0.1000000000000000056, 0.1027777777777777735, 0.1055555555555555552, 0.1083333333333333370, 0.1111111111111111049, 0.1138888888888888867, 0.1166666666666666685, 0.1194444444444444503, 0.1222222222222222182, 0.1250000000000000000, 0.1277777777777777679, 0.1305555555555555636, 0.1333333333333333315, 0.1361111111111110994, 0.1388888888888888951, 0.1416666666666666630, 0.1444444444444444309, 0.1472222222222222265, 0.1499999999999999944, 0.1527777777777777901, 0.1555555555555555580, 0.1583333333333333259, 0.1611111111111111216, 0.1638888888888888895, 0.1666666666666666574, 0.1694444444444444531, 0.1722222222222222210, 0.1749999999999999889, 0.1777777777777777846, 0.1805555555555555525, 0.1833333333333333204, 0.1861111111111111160, 0.1888888888888888840, 0.1916666666666666796, 0.1944444444444444475, 0.1972222222222222154, 0.2000000000000000111, 0.2027777777777777790, 0.2055555555555555469, 0.2083333333333333426, 0.2111111111111111105, 0.2138888888888888784, 0.2166666666666666741, 0.2194444444444444420, 0.2222222222222222099, 0.2250000000000000056, 0.2277777777777777735, 0.2305555555555555691, 0.2333333333333333370, 0.2361111111111111049, 0.2388888888888889006, 0.2416666666666666685, 0.2444444444444444364, 0.2472222222222222321, 0.2500000000000000000, 0.2527777777777777679, 0.2555555555555555358, 0.2583333333333333592, 0.2611111111111111271, 0.2638888888888888951, 0.2666666666666666630, 0.2694444444444444309, 0.2722222222222221988, 0.2750000000000000222, 0.2777777777777777901, 0.2805555555555555580, 0.2833333333333333259, 0.2861111111111110938, 0.2888888888888888618, 0.2916666666666666852, 0.2944444444444444531, 0.2972222222222222210, 0.2999999999999999889, 0.3027777777777777568, 0.3055555555555555802, 0.3083333333333333481, 0.3111111111111111160, 0.3138888888888888840, 0.3166666666666666519, 0.3194444444444444198, 0.3222222222222222432, 0.3250000000000000111, 0.3277777777777777790, 0.3305555555555555469, 0.3333333333333333148, 0.3361111111111111382, 0.3388888888888889062, 0.3416666666666666741, 0.3444444444444444420, 0.3472222222222222099, 0.3499999999999999778, 0.3527777777777778012, 0.3555555555555555691, 0.3583333333333333370, 0.3611111111111111049, 0.3638888888888888729, 0.3666666666666666408, 0.3694444444444444642, 0.3722222222222222321, 0.3750000000000000000, 0.3777777777777777679, 0.3805555555555555358, 0.3833333333333333592, 0.3861111111111111271, 0.3888888888888888951, 0.3916666666666666630, 0.3944444444444444309, 0.3972222222222221988, 0.4000000000000000222, 0.4027777777777777901, 0.4055555555555555580, 0.4083333333333333259, 0.4111111111111110938, 0.4138888888888888618, 0.4166666666666666852, 0.4194444444444444531, 0.4222222222222222210, 0.4249999999999999889, 0.4277777777777777568, 0.4305555555555555802, 0.4333333333333333481, 0.4361111111111111160, 0.4388888888888888840, 0.4416666666666666519, 0.4444444444444444198, 0.4472222222222222432, 0.4500000000000000111, 0.4527777777777777790, 0.4555555555555555469, 0.4583333333333333148, 0.4611111111111111382, 0.4638888888888889062, 0.4666666666666666741, 0.4694444444444444420, 0.4722222222222222099, 0.4749999999999999778, 0.4777777777777778012, 0.4805555555555555691, 0.4833333333333333370, 0.4861111111111111049, 0.4888888888888888729, 0.4916666666666666408, 0.4944444444444444642, 0.4972222222222222321, 0.5000000000000000000, 0.5027777777777777679, 0.5055555555555555358, 0.5083333333333333037, 0.5111111111111110716, 0.5138888888888888395, 0.5166666666666667185, 0.5194444444444444864, 0.5222222222222222543, 0.5250000000000000222, 0.5277777777777777901, 0.5305555555555555580, 0.5333333333333333259, 0.5361111111111110938, 0.5388888888888888618, 0.5416666666666666297, 0.5444444444444443976, 0.5472222222222222765, 0.5500000000000000444, 0.5527777777777778123, 0.5555555555555555802, 0.5583333333333333481, 0.5611111111111111160, 0.5638888888888888840, 0.5666666666666666519, 0.5694444444444444198, 0.5722222222222221877, 0.5749999999999999556, 0.5777777777777777235, 0.5805555555555556024, 0.5833333333333333703, 0.5861111111111111382, 0.5888888888888889062, 0.5916666666666666741, 0.5944444444444444420, 0.5972222222222222099, 0.5999999999999999778, 0.6027777777777777457, 0.6055555555555555136, 0.6083333333333332815, 0.6111111111111111605, 0.6138888888888889284, 0.6166666666666666963, 0.6194444444444444642, 0.6222222222222222321, 0.6250000000000000000, 0.6277777777777777679, 0.6305555555555555358, 0.6333333333333333037, 0.6361111111111110716, 0.6388888888888888395, 0.6416666666666667185, 0.6444444444444444864, 0.6472222222222222543, 0.6500000000000000222, 0.6527777777777777901, 0.6555555555555555580, 0.6583333333333333259, 0.6611111111111110938, 0.6638888888888888618, 0.6666666666666666297, 0.6694444444444443976, 0.6722222222222222765, 0.6750000000000000444, 0.6777777777777778123, 0.6805555555555555802, 0.6833333333333333481, 0.6861111111111111160, 0.6888888888888888840, 0.6916666666666666519, 0.6944444444444444198, 0.6972222222222221877, 0.6999999999999999556, 0.7027777777777777235, 0.7055555555555556024, 0.7083333333333333703, 0.7111111111111111382, 0.7138888888888889062, 0.7166666666666666741, 0.7194444444444444420, 0.7222222222222222099, 0.7249999999999999778, 0.7277777777777777457, 0.7305555555555555136, 0.7333333333333332815, 0.7361111111111111605, 0.7388888888888889284, 0.7416666666666666963, 0.7444444444444444642, 0.7472222222222222321, 0.7500000000000000000, 0.7527777777777777679, 0.7555555555555555358, 0.7583333333333333037, 0.7611111111111110716, 0.7638888888888888395, 0.7666666666666667185, 0.7694444444444444864, 0.7722222222222222543, 0.7750000000000000222, 0.7777777777777777901, 0.7805555555555555580, 0.7833333333333333259, 0.7861111111111110938, 0.7888888888888888618, 0.7916666666666666297, 0.7944444444444443976, 0.7972222222222222765, 0.8000000000000000444, 0.8027777777777778123, 0.8055555555555555802, 0.8083333333333333481, 0.8111111111111111160, 0.8138888888888888840, 0.8166666666666666519, 0.8194444444444444198, 0.8222222222222221877, 0.8249999999999999556, 0.8277777777777777235, 0.8305555555555556024, 0.8333333333333333703, 0.8361111111111111382, 0.8388888888888889062, 0.8416666666666666741, 0.8444444444444444420, 0.8472222222222222099, 0.8499999999999999778, 0.8527777777777777457, 0.8555555555555555136, 0.8583333333333332815, 0.8611111111111111605, 0.8638888888888889284, 0.8666666666666666963, 0.8694444444444444642, 0.8722222222222222321, 0.8750000000000000000, 0.8777777777777777679, 0.8805555555555555358, 0.8833333333333333037, 0.8861111111111110716, 0.8888888888888888395, 0.8916666666666667185, 0.8944444444444444864, 0.8972222222222222543, 0.9000000000000000222, 0.9027777777777777901, 0.9055555555555555580, 0.9083333333333333259, 0.9111111111111110938, 0.9138888888888888618, 0.9166666666666666297, 0.9194444444444443976, 0.9222222222222222765, 0.9250000000000000444, 0.9277777777777778123, 0.9305555555555555802, 0.9333333333333333481, 0.9361111111111111160, 0.9388888888888888840, 0.9416666666666666519, 0.9444444444444444198, 0.9472222222222221877, 0.9499999999999999556, 0.9527777777777777235, 0.9555555555555556024, 0.9583333333333333703, 0.9611111111111111382, 0.9638888888888889062, 0.9666666666666666741, 0.9694444444444444420, 0.9722222222222222099, 0.9749999999999999778, 0.9777777777777777457, 0.9805555555555555136, 0.9833333333333332815, 0.9861111111111111605, 0.9888888888888889284, 0.9916666666666666963, 0.9944444444444444642, 0.9972222222222222321, 1.000000000000000000 ),
 .UNSPECIFIED. ) 
 GEOMETRIC_REPRESENTATION_ITEM ( )  RATIONAL_B_SPLINE_SURFACE ( (
 ( 1.000000000000000000, 0.8660254037844387076, 1.000000000000000000, 0.8660254037844387076, 1.000000000000000000, 0.8660254037844387076, 1.000000000000000000, 0.8660254037844387076, 1.000000000000000000, 0.8660254037844387076, 1.000000000000000000, 0.8660254037844387076, 1.000000000000000000, 0.8660254037844387076, 1.000000000000000000, 0.8660254037844387076, 1.000000000000000000, 0.8660254037844387076, 1.000000000000000000, 0.8660254037844387076, 1.000000000000000000, 0.8660254037844387076, 1.000000000000000000, 0.8660254037844387076, 1.000000000000000000, 0.8660254037844387076, 1.000000000000000000, 0.8660254037844387076, 1.000000000000000000, 0.8660254037844387076, 1.000000000000000000, 0.8660254037844387076, 1.000000000000000000, 0.8660254037844387076, 1.000000000000000000, 0.8660254037844387076, 1.000000000000000000, 0.8660254037844387076, 1.000000000000000000, 0.8660254037844387076, 1.000000000000000000, 0.8660254037844387076, 1.000000000000000000, 0.8660254037844387076, 1.000000000000000000, 0.8660254037844387076, 1.000000000000000000, 0.8660254037844387076, 1.000000000000000000, 0.8660254037844387076, 1.000000000000000000, 0.8660254037844387076, 1.000000000000000000, 0.8660254037844387076, 1.000000000000000000, 0.8660254037844387076, 1.000000000000000000, 0.8660254037844387076, 1.000000000000000000, 0.8660254037844387076, 1.000000000000000000, 0.8660254037844387076, 1.000000000000000000, 0.8660254037844387076, 1.000000000000000000, 0.8660254037844387076, 1.000000000000000000, 0.8660254037844387076, 1.000000000000000000, 0.8660254037844387076, 1.000000000000000000, 0.8660254037844387076, 1.000000000000000000, 0.8660254037844387076, 1.000000000000000000, 0.8660254037844387076, 1.000000000000000000, 0.8660254037844387076, 1.000000000000000000, 0.8660254037844387076, 1.000000000000000000, 0.8660254037844387076, 1.000000000000000000, 0.8660254037844387076, 1.000000000000000000, 0.8660254037844387076, 1.000000000000000000, 0.8660254037844387076, 1.000000000000000000, 0.8660254037844387076, 1.000000000000000000, 0.8660254037844387076, 1.000000000000000000, 0.8660254037844387076, 1.000000000000000000, 0.8660254037844387076, 1.000000000000000000, 0.8660254037844387076, 1.000000000000000000, 0.8660254037844387076, 1.000000000000000000, 0.8660254037844387076, 1.000000000000000000, 0.8660254037844387076, 1.000000000000000000, 0.8660254037844387076, 1.000000000000000000, 0.8660254037844387076, 1.000000000000000000, 0.8660254037844387076, 1.000000000000000000, 0.8660254037844387076, 1.000000000000000000, 0.8660254037844387076, 1.000000000000000000, 0.8660254037844387076, 1.000000000000000000, 0.8660254037844387076, 1.000000000000000000, 0.8660254037844387076, 1.000000000000000000, 0.8660254037844387076, 1.000000000000000000, 0.8660254037844387076, 1.000000000000000000, 0.8660254037844387076, 1.000000000000000000, 0.8660254037844387076, 1.000000000000000000, 0.8660254037844387076, 1.000000000000000000, 0.8660254037844387076, 1.000000000000000000, 0.8660254037844387076, 1.000000000000000000, 0.8660254037844387076, 1.000000000000000000, 0.8660254037844387076, 1.000000000000000000, 0.8660254037844387076, 1.000000000000000000, 0.8660254037844387076, 1.000000000000000000, 0.8660254037844387076, 1.000000000000000000, 0.8660254037844387076, 1.000000000000000000, 0.8660254037844387076, 1.000000000000000000, 0.8660254037844387076, 1.000000000000000000, 0.8660254037844387076, 1.000000000000000000, 0.8660254037844387076, 1.000000000000000000, 0.8660254037844387076, 1.000000000000000000, 0.8660254037844387076, 1.000000000000000000, 0.8660254037844387076, 1.000000000000000000, 0.8660254037844387076, 1.000000000000000000, 0.8660254037844387076, 1.000000000000000000, 0.8660254037844387076, 1.000000000000000000, 0.8660254037844387076, 1.000000000000000000, 0.8660254037844387076, 1.000000000000000000, 0.8660254037844387076, 1.000000000000000000, 0.8660254037844387076, 1.000000000000000000, 0.8660254037844387076, 1.000000000000000000, 0.8660254037844387076, 1.000000000000000000, 0.8660254037844387076, 1.000000000000000000, 0.8660254037844387076, 1.000000000000000000, 0.8660254037844387076, 1.000000000000000000, 0.8660254037844387076, 1.000000000000000000, 0.8660254037844387076, 1.000000000000000000, 0.8660254037844387076, 1.000000000000000000, 0.8660254037844387076, 1.000000000000000000, 0.8660254037844387076, 1.000000000000000000, 0.8660254037844387076, 1.000000000000000000, 0.8660254037844387076, 1.000000000000000000, 0.8660254037844387076, 1.000000000000000000, 0.8660254037844387076, 1.000000000000000000, 0.8660254037844387076, 1.000000000000000000, 0.8660254037844387076, 1.000000000000000000, 0.8660254037844387076, 1.000000000000000000, 0.8660254037844387076, 1.000000000000000000, 0.8660254037844387076, 1.000000000000000000, 0.8660254037844387076, 1.000000000000000000, 0.8660254037844387076, 1.000000000000000000, 0.8660254037844387076, 1.000000000000000000, 0.8660254037844387076, 1.000000000000000000, 0.8660254037844387076, 1.000000000000000000, 0.8660254037844387076, 1.000000000000000000, 0.8660254037844387076, 1.000000000000000000, 0.8660254037844387076, 1.000000000000000000, 0.8660254037844387076, 1.000000000000000000, 0.8660254037844387076, 1.000000000000000000, 0.8660254037844387076, 1.000000000000000000, 0.8660254037844387076, 1.000000000000000000, 0.8660254037844387076, 1.000000000000000000, 0.8660254037844387076, 1.000000000000000000, 0.8660254037844387076, 1.000000000000000000, 0.8660254037844387076, 1.000000000000000000, 0.8660254037844387076, 1.000000000000000000, 0.8660254037844387076, 1.000000000000000000, 0.8660254037844387076, 1.000000000000000000, 0.8660254037844387076, 1.000000000000000000, 0.8660254037844387076, 1.000000000000000000, 0.8660254037844387076, 1.000000000000000000, 0.8660254037844387076, 1.000000000000000000, 0.8660254037844387076, 1.000000000000000000, 0.8660254037844387076, 1.000000000000000000, 0.8660254037844387076, 1.000000000000000000, 0.8660254037844387076, 1.000000000000000000, 0.8660254037844387076, 1.000000000000000000, 0.8660254037844387076, 1.000000000000000000, 0.8660254037844387076, 1.000000000000000000, 0.8660254037844387076, 1.000000000000000000, 0.8660254037844387076, 1.000000000000000000, 0.8660254037844387076, 1.000000000000000000, 0.8660254037844387076, 1.000000000000000000, 0.8660254037844387076, 1.000000000000000000, 0.8660254037844387076, 1.000000000000000000, 0.8660254037844387076, 1.000000000000000000, 0.8660254037844387076, 1.000000000000000000, 0.8660254037844387076, 1.000000000000000000, 0.8660254037844387076, 1.000000000000000000, 0.8660254037844387076, 1.000000000000000000, 0.8660254037844387076, 1.000000000000000000, 0.8660254037844387076, 1.000000000000000000, 0.8660254037844387076, 1.000000000000000000, 0.8660254037844387076, 1.000000000000000000, 0.8660254037844387076, 1.000000000000000000, 0.8660254037844387076, 1.000000000000000000, 0.8660254037844387076, 1.000000000000000000, 0.8660254037844387076, 1.000000000000000000, 0.8660254037844387076, 1.000000000000000000, 0.8660254037844387076, 1.000000000000000000, 0.8660254037844387076, 1.000000000000000000, 0.8660254037844387076, 1.000000000000000000, 0.8660254037844387076, 1.000000000000000000, 0.8660254037844387076, 1.000000000000000000, 0.8660254037844387076, 1.000000000000000000, 0.8660254037844387076, 1.000000000000000000, 0.8660254037844387076, 1.000000000000000000, 0.8660254037844387076, 1.000000000000000000, 0.8660254037844387076, 1.000000000000000000, 0.8660254037844387076, 1.000000000000000000, 0.8660254037844387076, 1.000000000000000000, 0.8660254037844387076, 1.000000000000000000, 0.8660254037844387076, 1.000000000000000000, 0.8660254037844387076, 1.000000000000000000, 0.8660254037844387076, 1.000000000000000000, 0.8660254037844387076, 1.000000000000000000, 0.8660254037844387076, 1.000000000000000000, 0.8660254037844387076, 1.000000000000000000, 0.8660254037844387076, 1.000000000000000000, 0.8660254037844387076, 1.000000000000000000, 0.8660254037844387076, 1.000000000000000000, 0.8660254037844387076, 1.000000000000000000, 0.8660254037844387076, 1.000000000000000000, 0.8660254037844387076, 1.000000000000000000, 0.8660254037844387076, 1.000000000000000000, 0.8660254037844387076, 1.000000000000000000, 0.8660254037844387076, 1.000000000000000000, 0.8660254037844387076, 1.000000000000000000, 0.8660254037844387076, 1.000000000000000000, 0.8660254037844387076, 1.000000000000000000, 0.8660254037844387076, 1.000000000000000000, 0.8660254037844387076, 1.000000000000000000, 0.8660254037844387076, 1.000000000000000000, 0.8660254037844387076, 1.000000000000000000, 0.8660254037844387076, 1.000000000000000000, 0.8660254037844387076, 1.000000000000000000, 0.8660254037844387076, 1.000000000000000000, 0.8660254037844387076, 1.000000000000000000, 0.8660254037844387076, 1.000000000000000000, 0.8660254037844387076, 1.000000000000000000, 0.8660254037844387076, 1.000000000000000000, 0.8660254037844387076, 1.000000000000000000, 0.8660254037844387076, 1.000000000000000000, 0.8660254037844387076, 1.000000000000000000, 0.8660254037844387076, 1.000000000000000000, 0.8660254037844387076, 1.000000000000000000, 0.8660254037844387076, 1.000000000000000000, 0.8660254037844387076, 1.000000000000000000, 0.8660254037844387076, 1.000000000000000000, 0.8660254037844387076, 1.000000000000000000, 0.8660254037844387076, 1.000000000000000000, 0.8660254037844387076, 1.000000000000000000, 0.8660254037844387076, 1.000000000000000000, 0.8660254037844387076, 1.000000000000000000, 0.8660254037844387076, 1.000000000000000000, 0.8660254037844387076, 1.000000000000000000, 0.8660254037844387076, 1.000000000000000000, 0.8660254037844387076, 1.000000000000000000, 0.8660254037844387076, 1.000000000000000000, 0.8660254037844387076, 1.000000000000000000, 0.8660254037844387076, 1.000000000000000000, 0.8660254037844387076, 1.000000000000000000, 0.8660254037844387076, 1.000000000000000000, 0.8660254037844387076, 1.000000000000000000, 0.8660254037844387076, 1.000000000000000000, 0.8660254037844387076, 1.000000000000000000, 0.8660254037844387076, 1.000000000000000000, 0.8660254037844387076, 1.000000000000000000, 0.8660254037844387076, 1.000000000000000000, 0.8660254037844387076, 1.000000000000000000, 0.8660254037844387076, 1.000000000000000000, 0.8660254037844387076, 1.000000000000000000, 0.8660254037844387076, 1.000000000000000000, 0.8660254037844387076, 1.000000000000000000, 0.8660254037844387076, 1.000000000000000000, 0.8660254037844387076, 1.000000000000000000, 0.8660254037844387076, 1.000000000000000000, 0.8660254037844387076, 1.000000000000000000, 0.8660254037844387076, 1.000000000000000000, 0.8660254037844387076, 1.000000000000000000, 0.8660254037844387076, 1.000000000000000000, 0.8660254037844387076, 1.000000000000000000, 0.8660254037844387076, 1.000000000000000000, 0.8660254037844387076, 1.000000000000000000, 0.8660254037844387076, 1.000000000000000000, 0.8660254037844387076, 1.000000000000000000, 0.8660254037844387076, 1.000000000000000000, 0.8660254037844387076, 1.000000000000000000, 0.8660254037844387076, 1.000000000000000000, 0.8660254037844387076, 1.000000000000000000, 0.8660254037844387076, 1.000000000000000000, 0.8660254037844387076, 1.000000000000000000, 0.8660254037844387076, 1.000000000000000000, 0.8660254037844387076, 1.000000000000000000, 0.8660254037844387076, 1.000000000000000000, 0.8660254037844387076, 1.000000000000000000, 0.8660254037844387076, 1.000000000000000000, 0.8660254037844387076, 1.000000000000000000, 0.8660254037844387076, 1.000000000000000000, 0.8660254037844387076, 1.000000000000000000, 0.8660254037844387076, 1.000000000000000000, 0.8660254037844387076, 1.000000000000000000, 0.8660254037844387076, 1.000000000000000000, 0.8660254037844387076, 1.000000000000000000, 0.8660254037844387076, 1.000000000000000000, 0.8660254037844387076, 1.000000000000000000, 0.8660254037844387076, 1.000000000000000000, 0.8660254037844387076, 1.000000000000000000, 0.8660254037844387076, 1.000000000000000000, 0.8660254037844387076, 1.000000000000000000, 0.8660254037844387076, 1.000000000000000000, 0.8660254037844387076, 1.000000000000000000, 0.8660254037844387076, 1.000000000000000000, 0.8660254037844387076, 1.000000000000000000, 0.8660254037844387076, 1.000000000000000000, 0.8660254037844387076, 1.000000000000000000, 0.8660254037844387076, 1.000000000000000000, 0.8660254037844387076, 1.000000000000000000, 0.8660254037844387076, 1.000000000000000000, 0.8660254037844387076, 1.000000000000000000, 0.8660254037844387076, 1.000000000000000000, 0.8660254037844387076, 1.000000000000000000, 0.8660254037844387076, 1.000000000000000000, 0.8660254037844387076, 1.000000000000000000, 0.8660254037844387076, 1.000000000000000000, 0.8660254037844387076, 1.000000000000000000, 0.8660254037844387076, 1.000000000000000000, 0.8660254037844387076, 1.000000000000000000, 0.8660254037844387076, 1.000000000000000000, 0.8660254037844387076, 1.000000000000000000, 0.8660254037844387076, 1.000000000000000000, 0.8660254037844387076, 1.000000000000000000, 0.8660254037844387076, 1.000000000000000000, 0.8660254037844387076, 1.000000000000000000, 0.8660254037844387076, 1.000000000000000000, 0.8660254037844387076, 1.000000000000000000, 0.8660254037844387076, 1.000000000000000000, 0.8660254037844387076, 1.000000000000000000, 0.8660254037844387076, 1.000000000000000000, 0.8660254037844387076, 1.000000000000000000, 0.8660254037844387076, 1.000000000000000000, 0.8660254037844387076, 1.000000000000000000, 0.8660254037844387076, 1.000000000000000000, 0.8660254037844387076, 1.000000000000000000, 0.8660254037844387076, 1.000000000000000000, 0.8660254037844387076, 1.000000000000000000, 0.8660254037844387076, 1.000000000000000000, 0.8660254037844387076, 1.000000000000000000, 0.8660254037844387076, 1.000000000000000000, 0.8660254037844387076, 1.000000000000000000, 0.8660254037844387076, 1.000000000000000000, 0.8660254037844387076, 1.000000000000000000, 0.8660254037844387076, 1.000000000000000000, 0.8660254037844387076, 1.000000000000000000, 0.8660254037844387076, 1.000000000000000000, 0.8660254037844387076, 1.000000000000000000, 0.8660254037844387076, 1.000000000000000000, 0.8660254037844387076, 1.000000000000000000, 0.8660254037844387076, 1.000000000000000000, 0.8660254037844387076, 1.000000000000000000, 0.8660254037844387076, 1.000000000000000000, 0.8660254037844387076, 1.000000000000000000, 0.8660254037844387076, 1.000000000000000000, 0.8660254037844387076, 1.000000000000000000, 0.8660254037844387076, 1.000000000000000000, 0.8660254037844387076, 1.000000000000000000, 0.8660254037844387076, 1.000000000000000000, 0.8660254037844387076, 1.000000000000000000, 0.8660254037844387076, 1.000000000000000000, 0.8660254037844387076, 1.000000000000000000, 0.8660254037844387076, 1.000000000000000000, 0.8660254037844387076, 1.000000000000000000, 0.8660254037844387076, 1.000000000000000000, 0.8660254037844387076, 1.000000000000000000, 0.8660254037844387076, 1.000000000000000000, 0.8660254037844387076, 1.000000000000000000, 0.8660254037844387076, 1.000000000000000000, 0.8660254037844387076, 1.000000000000000000, 0.8660254037844387076, 1.000000000000000000, 0.8660254037844387076, 1.000000000000000000, 0.8660254037844387076, 1.000000000000000000, 0.8660254037844387076, 1.000000000000000000, 0.8660254037844387076, 1.000000000000000000, 0.8660254037844387076, 1.000000000000000000, 0.8660254037844387076, 1.000000000000000000, 0.8660254037844387076, 1.000000000000000000, 0.8660254037844387076, 1.000000000000000000, 0.8660254037844387076, 1.000000000000000000, 0.8660254037844387076, 1.000000000000000000, 0.8660254037844387076, 1.000000000000000000, 0.8660254037844387076, 1.000000000000000000, 0.8660254037844387076, 1.000000000000000000, 0.8660254037844387076, 1.000000000000000000, 0.8660254037844387076, 1.000000000000000000, 0.8660254037844387076, 1.000000000000000000, 0.8660254037844387076, 1.000000000000000000, 0.8660254037844387076, 1.000000000000000000, 0.8660254037844387076, 1.000000000000000000, 0.8660254037844387076, 1.000000000000000000, 0.8660254037844387076, 1.000000000000000000, 0.8660254037844387076, 1.000000000000000000, 0.8660254037844387076, 1.000000000000000000, 0.8660254037844387076, 1.000000000000000000),
 ( 1.000000000000000000, 0.8660254037844387076, 1.000000000000000000, 0.8660254037844387076, 1.000000000000000000, 0.8660254037844387076, 1.000000000000000000, 0.8660254037844387076, 1.000000000000000000, 0.8660254037844387076, 1.000000000000000000, 0.8660254037844387076, 1.000000000000000000, 0.8660254037844387076, 1.000000000000000000, 0.8660254037844387076, 1.000000000000000000, 0.8660254037844387076, 1.000000000000000000, 0.8660254037844387076, 1.000000000000000000, 0.8660254037844387076, 1.000000000000000000, 0.8660254037844387076, 1.000000000000000000, 0.8660254037844387076, 1.000000000000000000, 0.8660254037844387076, 1.000000000000000000, 0.8660254037844387076, 1.000000000000000000, 0.8660254037844387076, 1.000000000000000000, 0.8660254037844387076, 1.000000000000000000, 0.8660254037844387076, 1.000000000000000000, 0.8660254037844387076, 1.000000000000000000, 0.8660254037844387076, 1.000000000000000000, 0.8660254037844387076, 1.000000000000000000, 0.8660254037844387076, 1.000000000000000000, 0.8660254037844387076, 1.000000000000000000, 0.8660254037844387076, 1.000000000000000000, 0.8660254037844387076, 1.000000000000000000, 0.8660254037844387076, 1.000000000000000000, 0.8660254037844387076, 1.000000000000000000, 0.8660254037844387076, 1.000000000000000000, 0.8660254037844387076, 1.000000000000000000, 0.8660254037844387076, 1.000000000000000000, 0.8660254037844387076, 1.000000000000000000, 0.8660254037844387076, 1.000000000000000000, 0.8660254037844387076, 1.000000000000000000, 0.8660254037844387076, 1.000000000000000000, 0.8660254037844387076, 1.000000000000000000, 0.8660254037844387076, 1.000000000000000000, 0.8660254037844387076, 1.000000000000000000, 0.8660254037844387076, 1.000000000000000000, 0.8660254037844387076, 1.000000000000000000, 0.8660254037844387076, 1.000000000000000000, 0.8660254037844387076, 1.000000000000000000, 0.8660254037844387076, 1.000000000000000000, 0.8660254037844387076, 1.000000000000000000, 0.8660254037844387076, 1.000000000000000000, 0.8660254037844387076, 1.000000000000000000, 0.8660254037844387076, 1.000000000000000000, 0.8660254037844387076, 1.000000000000000000, 0.8660254037844387076, 1.000000000000000000, 0.8660254037844387076, 1.000000000000000000, 0.8660254037844387076, 1.000000000000000000, 0.8660254037844387076, 1.000000000000000000, 0.8660254037844387076, 1.000000000000000000, 0.8660254037844387076, 1.000000000000000000, 0.8660254037844387076, 1.000000000000000000, 0.8660254037844387076, 1.000000000000000000, 0.8660254037844387076, 1.000000000000000000, 0.8660254037844387076, 1.000000000000000000, 0.8660254037844387076, 1.000000000000000000, 0.8660254037844387076, 1.000000000000000000, 0.8660254037844387076, 1.000000000000000000, 0.8660254037844387076, 1.000000000000000000, 0.8660254037844387076, 1.000000000000000000, 0.8660254037844387076, 1.000000000000000000, 0.8660254037844387076, 1.000000000000000000, 0.8660254037844387076, 1.000000000000000000, 0.8660254037844387076, 1.000000000000000000, 0.8660254037844387076, 1.000000000000000000, 0.8660254037844387076, 1.000000000000000000, 0.8660254037844387076, 1.000000000000000000, 0.8660254037844387076, 1.000000000000000000, 0.8660254037844387076, 1.000000000000000000, 0.8660254037844387076, 1.000000000000000000, 0.8660254037844387076, 1.000000000000000000, 0.8660254037844387076, 1.000000000000000000, 0.8660254037844387076, 1.000000000000000000, 0.8660254037844387076, 1.000000000000000000, 0.8660254037844387076, 1.000000000000000000, 0.8660254037844387076, 1.000000000000000000, 0.8660254037844387076, 1.000000000000000000, 0.8660254037844387076, 1.000000000000000000, 0.8660254037844387076, 1.000000000000000000, 0.8660254037844387076, 1.000000000000000000, 0.8660254037844387076, 1.000000000000000000, 0.8660254037844387076, 1.000000000000000000, 0.8660254037844387076, 1.000000000000000000, 0.8660254037844387076, 1.000000000000000000, 0.8660254037844387076, 1.000000000000000000, 0.8660254037844387076, 1.000000000000000000, 0.8660254037844387076, 1.000000000000000000, 0.8660254037844387076, 1.000000000000000000, 0.8660254037844387076, 1.000000000000000000, 0.8660254037844387076, 1.000000000000000000, 0.8660254037844387076, 1.000000000000000000, 0.8660254037844387076, 1.000000000000000000, 0.8660254037844387076, 1.000000000000000000, 0.8660254037844387076, 1.000000000000000000, 0.8660254037844387076, 1.000000000000000000, 0.8660254037844387076, 1.000000000000000000, 0.8660254037844387076, 1.000000000000000000, 0.8660254037844387076, 1.000000000000000000, 0.8660254037844387076, 1.000000000000000000, 0.8660254037844387076, 1.000000000000000000, 0.8660254037844387076, 1.000000000000000000, 0.8660254037844387076, 1.000000000000000000, 0.8660254037844387076, 1.000000000000000000, 0.8660254037844387076, 1.000000000000000000, 0.8660254037844387076, 1.000000000000000000, 0.8660254037844387076, 1.000000000000000000, 0.8660254037844387076, 1.000000000000000000, 0.8660254037844387076, 1.000000000000000000, 0.8660254037844387076, 1.000000000000000000, 0.8660254037844387076, 1.000000000000000000, 0.8660254037844387076, 1.000000000000000000, 0.8660254037844387076, 1.000000000000000000, 0.8660254037844387076, 1.000000000000000000, 0.8660254037844387076, 1.000000000000000000, 0.8660254037844387076, 1.000000000000000000, 0.8660254037844387076, 1.000000000000000000, 0.8660254037844387076, 1.000000000000000000, 0.8660254037844387076, 1.000000000000000000, 0.8660254037844387076, 1.000000000000000000, 0.8660254037844387076, 1.000000000000000000, 0.8660254037844387076, 1.000000000000000000, 0.8660254037844387076, 1.000000000000000000, 0.8660254037844387076, 1.000000000000000000, 0.8660254037844387076, 1.000000000000000000, 0.8660254037844387076, 1.000000000000000000, 0.8660254037844387076, 1.000000000000000000, 0.8660254037844387076, 1.000000000000000000, 0.8660254037844387076, 1.000000000000000000, 0.8660254037844387076, 1.000000000000000000, 0.8660254037844387076, 1.000000000000000000, 0.8660254037844387076, 1.000000000000000000, 0.8660254037844387076, 1.000000000000000000, 0.8660254037844387076, 1.000000000000000000, 0.8660254037844387076, 1.000000000000000000, 0.8660254037844387076, 1.000000000000000000, 0.8660254037844387076, 1.000000000000000000, 0.8660254037844387076, 1.000000000000000000, 0.8660254037844387076, 1.000000000000000000, 0.8660254037844387076, 1.000000000000000000, 0.8660254037844387076, 1.000000000000000000, 0.8660254037844387076, 1.000000000000000000, 0.8660254037844387076, 1.000000000000000000, 0.8660254037844387076, 1.000000000000000000, 0.8660254037844387076, 1.000000000000000000, 0.8660254037844387076, 1.000000000000000000, 0.8660254037844387076, 1.000000000000000000, 0.8660254037844387076, 1.000000000000000000, 0.8660254037844387076, 1.000000000000000000, 0.8660254037844387076, 1.000000000000000000, 0.8660254037844387076, 1.000000000000000000, 0.8660254037844387076, 1.000000000000000000, 0.8660254037844387076, 1.000000000000000000, 0.8660254037844387076, 1.000000000000000000, 0.8660254037844387076, 1.000000000000000000, 0.8660254037844387076, 1.000000000000000000, 0.8660254037844387076, 1.000000000000000000, 0.8660254037844387076, 1.000000000000000000, 0.8660254037844387076, 1.000000000000000000, 0.8660254037844387076, 1.000000000000000000, 0.8660254037844387076, 1.000000000000000000, 0.8660254037844387076, 1.000000000000000000, 0.8660254037844387076, 1.000000000000000000, 0.8660254037844387076, 1.000000000000000000, 0.8660254037844387076, 1.000000000000000000, 0.8660254037844387076, 1.000000000000000000, 0.8660254037844387076, 1.000000000000000000, 0.8660254037844387076, 1.000000000000000000, 0.8660254037844387076, 1.000000000000000000, 0.8660254037844387076, 1.000000000000000000, 0.8660254037844387076, 1.000000000000000000, 0.8660254037844387076, 1.000000000000000000, 0.8660254037844387076, 1.000000000000000000, 0.8660254037844387076, 1.000000000000000000, 0.8660254037844387076, 1.000000000000000000, 0.8660254037844387076, 1.000000000000000000, 0.8660254037844387076, 1.000000000000000000, 0.8660254037844387076, 1.000000000000000000, 0.8660254037844387076, 1.000000000000000000, 0.8660254037844387076, 1.000000000000000000, 0.8660254037844387076, 1.000000000000000000, 0.8660254037844387076, 1.000000000000000000, 0.8660254037844387076, 1.000000000000000000, 0.8660254037844387076, 1.000000000000000000, 0.8660254037844387076, 1.000000000000000000, 0.8660254037844387076, 1.000000000000000000, 0.8660254037844387076, 1.000000000000000000, 0.8660254037844387076, 1.000000000000000000, 0.8660254037844387076, 1.000000000000000000, 0.8660254037844387076, 1.000000000000000000, 0.8660254037844387076, 1.000000000000000000, 0.8660254037844387076, 1.000000000000000000, 0.8660254037844387076, 1.000000000000000000, 0.8660254037844387076, 1.000000000000000000, 0.8660254037844387076, 1.000000000000000000, 0.8660254037844387076, 1.000000000000000000, 0.8660254037844387076, 1.000000000000000000, 0.8660254037844387076, 1.000000000000000000, 0.8660254037844387076, 1.000000000000000000, 0.8660254037844387076, 1.000000000000000000, 0.8660254037844387076, 1.000000000000000000, 0.8660254037844387076, 1.000000000000000000, 0.8660254037844387076, 1.000000000000000000, 0.8660254037844387076, 1.000000000000000000, 0.8660254037844387076, 1.000000000000000000, 0.8660254037844387076, 1.000000000000000000, 0.8660254037844387076, 1.000000000000000000, 0.8660254037844387076, 1.000000000000000000, 0.8660254037844387076, 1.000000000000000000, 0.8660254037844387076, 1.000000000000000000, 0.8660254037844387076, 1.000000000000000000, 0.8660254037844387076, 1.000000000000000000, 0.8660254037844387076, 1.000000000000000000, 0.8660254037844387076, 1.000000000000000000, 0.8660254037844387076, 1.000000000000000000, 0.8660254037844387076, 1.000000000000000000, 0.8660254037844387076, 1.000000000000000000, 0.8660254037844387076, 1.000000000000000000, 0.8660254037844387076, 1.000000000000000000, 0.8660254037844387076, 1.000000000000000000, 0.8660254037844387076, 1.000000000000000000, 0.8660254037844387076, 1.000000000000000000, 0.8660254037844387076, 1.000000000000000000, 0.8660254037844387076, 1.000000000000000000, 0.8660254037844387076, 1.000000000000000000, 0.8660254037844387076, 1.000000000000000000, 0.8660254037844387076, 1.000000000000000000, 0.8660254037844387076, 1.000000000000000000, 0.8660254037844387076, 1.000000000000000000, 0.8660254037844387076, 1.000000000000000000, 0.8660254037844387076, 1.000000000000000000, 0.8660254037844387076, 1.000000000000000000, 0.8660254037844387076, 1.000000000000000000, 0.8660254037844387076, 1.000000000000000000, 0.8660254037844387076, 1.000000000000000000, 0.8660254037844387076, 1.000000000000000000, 0.8660254037844387076, 1.000000000000000000, 0.8660254037844387076, 1.000000000000000000, 0.8660254037844387076, 1.000000000000000000, 0.8660254037844387076, 1.000000000000000000, 0.8660254037844387076, 1.000000000000000000, 0.8660254037844387076, 1.000000000000000000, 0.8660254037844387076, 1.000000000000000000, 0.8660254037844387076, 1.000000000000000000, 0.8660254037844387076, 1.000000000000000000, 0.8660254037844387076, 1.000000000000000000, 0.8660254037844387076, 1.000000000000000000, 0.8660254037844387076, 1.000000000000000000, 0.8660254037844387076, 1.000000000000000000, 0.8660254037844387076, 1.000000000000000000, 0.8660254037844387076, 1.000000000000000000, 0.8660254037844387076, 1.000000000000000000, 0.8660254037844387076, 1.000000000000000000, 0.8660254037844387076, 1.000000000000000000, 0.8660254037844387076, 1.000000000000000000, 0.8660254037844387076, 1.000000000000000000, 0.8660254037844387076, 1.000000000000000000, 0.8660254037844387076, 1.000000000000000000, 0.8660254037844387076, 1.000000000000000000, 0.8660254037844387076, 1.000000000000000000, 0.8660254037844387076, 1.000000000000000000, 0.8660254037844387076, 1.000000000000000000, 0.8660254037844387076, 1.000000000000000000, 0.8660254037844387076, 1.000000000000000000, 0.8660254037844387076, 1.000000000000000000, 0.8660254037844387076, 1.000000000000000000, 0.8660254037844387076, 1.000000000000000000, 0.8660254037844387076, 1.000000000000000000, 0.8660254037844387076, 1.000000000000000000, 0.8660254037844387076, 1.000000000000000000, 0.8660254037844387076, 1.000000000000000000, 0.8660254037844387076, 1.000000000000000000, 0.8660254037844387076, 1.000000000000000000, 0.8660254037844387076, 1.000000000000000000, 0.8660254037844387076, 1.000000000000000000, 0.8660254037844387076, 1.000000000000000000, 0.8660254037844387076, 1.000000000000000000, 0.8660254037844387076, 1.000000000000000000, 0.8660254037844387076, 1.000000000000000000, 0.8660254037844387076, 1.000000000000000000, 0.8660254037844387076, 1.000000000000000000, 0.8660254037844387076, 1.000000000000000000, 0.8660254037844387076, 1.000000000000000000, 0.8660254037844387076, 1.000000000000000000, 0.8660254037844387076, 1.000000000000000000, 0.8660254037844387076, 1.000000000000000000, 0.8660254037844387076, 1.000000000000000000, 0.8660254037844387076, 1.000000000000000000, 0.8660254037844387076, 1.000000000000000000, 0.8660254037844387076, 1.000000000000000000, 0.8660254037844387076, 1.000000000000000000, 0.8660254037844387076, 1.000000000000000000, 0.8660254037844387076, 1.000000000000000000, 0.8660254037844387076, 1.000000000000000000, 0.8660254037844387076, 1.000000000000000000, 0.8660254037844387076, 1.000000000000000000, 0.8660254037844387076, 1.000000000000000000, 0.8660254037844387076, 1.000000000000000000, 0.8660254037844387076, 1.000000000000000000, 0.8660254037844387076, 1.000000000000000000, 0.8660254037844387076, 1.000000000000000000, 0.8660254037844387076, 1.000000000000000000, 0.8660254037844387076, 1.000000000000000000, 0.8660254037844387076, 1.000000000000000000, 0.8660254037844387076, 1.000000000000000000, 0.8660254037844387076, 1.000000000000000000, 0.8660254037844387076, 1.000000000000000000, 0.8660254037844387076, 1.000000000000000000, 0.8660254037844387076, 1.000000000000000000, 0.8660254037844387076, 1.000000000000000000, 0.8660254037844387076, 1.000000000000000000, 0.8660254037844387076, 1.000000000000000000, 0.8660254037844387076, 1.000000000000000000, 0.8660254037844387076, 1.000000000000000000, 0.8660254037844387076, 1.000000000000000000, 0.8660254037844387076, 1.000000000000000000, 0.8660254037844387076, 1.000000000000000000, 0.8660254037844387076, 1.000000000000000000, 0.8660254037844387076, 1.000000000000000000, 0.8660254037844387076, 1.000000000000000000, 0.8660254037844387076, 1.000000000000000000, 0.8660254037844387076, 1.000000000000000000, 0.8660254037844387076, 1.000000000000000000, 0.8660254037844387076, 1.000000000000000000, 0.8660254037844387076, 1.000000000000000000, 0.8660254037844387076, 1.000000000000000000, 0.8660254037844387076, 1.000000000000000000, 0.8660254037844387076, 1.000000000000000000, 0.8660254037844387076, 1.000000000000000000, 0.8660254037844387076, 1.000000000000000000, 0.8660254037844387076, 1.000000000000000000, 0.8660254037844387076, 1.000000000000000000, 0.8660254037844387076, 1.000000000000000000, 0.8660254037844387076, 1.000000000000000000, 0.8660254037844387076, 1.000000000000000000, 0.8660254037844387076, 1.000000000000000000, 0.8660254037844387076, 1.000000000000000000, 0.8660254037844387076, 1.000000000000000000, 0.8660254037844387076, 1.000000000000000000, 0.8660254037844387076, 1.000000000000000000, 0.8660254037844387076, 1.000000000000000000, 0.8660254037844387076, 1.000000000000000000, 0.8660254037844387076, 1.000000000000000000, 0.8660254037844387076, 1.000000000000000000, 0.8660254037844387076, 1.000000000000000000, 0.8660254037844387076, 1.000000000000000000, 0.8660254037844387076, 1.000000000000000000, 0.8660254037844387076, 1.000000000000000000, 0.8660254037844387076, 1.000000000000000000, 0.8660254037844387076, 1.000000000000000000, 0.8660254037844387076, 1.000000000000000000, 0.8660254037844387076, 1.000000000000000000, 0.8660254037844387076, 1.000000000000000000, 0.8660254037844387076, 1.000000000000000000, 0.8660254037844387076, 1.000000000000000000, 0.8660254037844387076, 1.000000000000000000, 0.8660254037844387076, 1.000000000000000000, 0.8660254037844387076, 1.000000000000000000, 0.8660254037844387076, 1.000000000000000000) ) ) 
 REPRESENTATION_ITEM ( '' )  SURFACE ( )  );
#46697 = CARTESIAN_POINT ( 'NONE',  ( 9.975000000000001421, 6.123233995736764310E-16, -4.999999999999998224 ) ) ;
#46698 = CARTESIAN_POINT ( 'NONE',  ( 19.12500000122903288, 2.886751345948129099, -4.999999999999998224 ) ) ;
#46699 = CARTESIAN_POINT ( 'NONE',  ( -3.999999999999999112, 18.76250000122903216, -30.00000000000000000 ) ) ;
#46700 = CARTESIAN_POINT ( 'NONE',  ( 10.09687500061451715, -4.119189519843965641, -2.378215178125001383 ) ) ;
#46701 = VERTEX_POINT ( 'NONE', #60081 ) ;
#46702 = CARTESIAN_POINT ( 'NONE',  ( 16.64999999999999858, -4.330127018922190985, -2.500000000000001332 ) ) ;
#46703 = CARTESIAN_POINT ( 'NONE',  ( 21.89999999999999858, 0.000000000000000000, 4.999999999999998224 ) ) ;
#46704 =( BOUNDED_CURVE ( )  B_SPLINE_CURVE ( 2, ( #17953, #35321, #12429, #34963, #68954, #29425, #51960 ),
 .UNSPECIFIED., .F., .F. ) 
 B_SPLINE_CURVE_WITH_KNOTS ( ( 3, 2, 2, 3 ),
 ( 0.2500000000000000000, 0.2527777777777777679, 0.2555555555555554803, 0.2583333333333333037 ),
 .UNSPECIFIED. ) 
 CURVE ( )  GEOMETRIC_REPRESENTATION_ITEM ( )  RATIONAL_B_SPLINE_CURVE ( ( 1.000000000000000000, 0.8660254037844387076, 1.000000000000000000, 0.8660254037844387076, 1.000000000000000000, 0.8660254037844413721, 0.9999999999999973355 ) ) 
 REPRESENTATION_ITEM ( '' )  );
#46705 = CARTESIAN_POINT ( 'NONE',  ( 18.15937500061451715, 0.000000000000000000, 5.243569643749999010 ) ) ;
#46706 = CARTESIAN_POINT ( 'NONE',  ( 25.04062500061451502, -3.027376345333610441, -5.243569643749999898 ) ) ;
#46707 = VERTEX_POINT ( 'NONE', #27217 ) ;
#46708 = CARTESIAN_POINT ( 'NONE',  ( 28.08750000122903145, 6.123233995736764310E-16, -4.999999999999998224 ) ) ;
#46709 = CARTESIAN_POINT ( 'NONE',  ( 6.140625000614516438, -3.027376345333610441, -5.243569643749999898 ) ) ;
#46710 = CARTESIAN_POINT ( 'NONE',  ( 3.999999999999999112, 15.38750000122903394, 30.00000000000000000 ) ) ;
#46711 = CARTESIAN_POINT ( 'NONE',  ( 13.42499999999999893, -4.330127018922194537, 2.499999999999995559 ) ) ;
#46712 = CARTESIAN_POINT ( 'NONE',  ( -4.243569643749999898, 16.61562500061451786, 27.54997392385601529 ) ) ;
#46713 = CARTESIAN_POINT ( 'NONE',  ( 28.82812500061451644, 4.541064518000418104, 2.621784821874999949 ) ) ;
#46714 = CARTESIAN_POINT ( 'NONE',  ( 9.975000000000001421, 6.123233995736764310E-16, -4.999999999999998224 ) ) ;
#46715 = CARTESIAN_POINT ( 'NONE',  ( -3.756430356250000102, 18.26562499938548356, 30.00000000000000000 ) ) ;
#46716 = CARTESIAN_POINT ( 'NONE',  ( 25.13437500061451502, 6.421520780324663323E-16, -5.243569643749999010 ) ) ;
#46717 = ORIENTED_EDGE ( 'NONE', *, *, #8966, .T. ) ;
#46718 = CARTESIAN_POINT ( 'NONE',  ( 21.44062500061452070, -3.027376345333610441, -5.243569643749999898 ) ) ;
#46719 = CARTESIAN_POINT ( 'NONE',  ( 22.35937500061451644, -4.541064518000417216, -2.621784821875001281 ) ) ;
#46720 = CARTESIAN_POINT ( 'NONE',  ( 9.001249775931846008E-16, 17.21562500061459744, -25.09994784771203058 ) ) ;
#46721 = CARTESIAN_POINT ( 'NONE',  ( 5.878125000614517148, 4.541064518000418104, 2.621784821874999949 ) ) ;
#46722 = CARTESIAN_POINT ( 'NONE',  ( 29.18437500061451573, 5.824947211148865298E-16, -4.756430356249998326 ) ) ;
#46723 = CARTESIAN_POINT ( 'NONE',  ( 24.44062500061451715, -3.027376345333614438, 5.243569643749998122 ) ) ;
#46724 = CARTESIAN_POINT ( 'NONE',  ( 27.75937500061451502, 2.746126346562645981, -4.756430356249997438 ) ) ;
#46725 = CARTESIAN_POINT ( 'NONE',  ( 12.49687500061451573, -2.746126346562642428, -4.756430356249999214 ) ) ;
#46726 = CARTESIAN_POINT ( 'NONE',  ( 16.77187500061451786, 3.027376345333611329, 5.243569643749999010 ) ) ;
#46727 = CARTESIAN_POINT ( 'NONE',  ( 19.02187500061451786, 3.027376345333611329, 5.243569643749999010 ) ) ;
#46728 = CARTESIAN_POINT ( 'NONE',  ( 28.20937500061451786, -4.541064518000417216, -2.621784821875001281 ) ) ;
#46729 = CARTESIAN_POINT ( 'NONE',  ( 4.243569643749999898, 15.54687500061451644, 32.45002607614398471 ) ) ;
#46730 = CARTESIAN_POINT ( 'NONE',  ( 6.890625000614516438, -3.027376345333614438, 5.243569643749998122 ) ) ;
#46731 = CARTESIAN_POINT ( 'NONE',  ( 1.071796769724497445, 16.26740381056766438, 26.00000000000000355 ) ) ;
#46732 =( BOUNDED_CURVE ( )  B_SPLINE_CURVE ( 2, ( #21138, #3806, #15232, #37770, #4172, #442, #28159 ),
 .UNSPECIFIED., .F., .F. ) 
 B_SPLINE_CURVE_WITH_KNOTS ( ( 3, 2, 2, 3 ),
 ( 0.4900000000000001021, 0.4933333333333334569, 0.4966666666666667562, 0.5000000000000001110 ),
 .UNSPECIFIED. ) 
 CURVE ( )  GEOMETRIC_REPRESENTATION_ITEM ( )  RATIONAL_B_SPLINE_CURVE ( ( 0.9999999999999955591, 0.8660254037844431485, 1.000000000000000000, 0.8660254037844387076, 1.000000000000000000, 0.8660254037844342667, 1.000000000000004441 ) ) 
 REPRESENTATION_ITEM ( '' )  );
#46733 = CARTESIAN_POINT ( 'NONE',  ( 5.034375000614519813, 4.541064518000418104, 2.621784821874999949 ) ) ;
#46734 = CARTESIAN_POINT ( 'NONE',  ( -1.071796769724491671, 13.53259618943233633, 26.00000000000000355 ) ) ;
#46735 = CARTESIAN_POINT ( 'NONE',  ( 4.115625000614516082, 3.027376345333611329, 5.243569643749999010 ) ) ;
#46736 = CARTESIAN_POINT ( 'NONE',  ( 9.721875000614517148, -6.054752690667223547, -1.112240025338166033E-15 ) ) ;
#46737 =( LENGTH_UNIT ( ) NAMED_UNIT ( * ) SI_UNIT ( .MILLI., .METRE. ) );
#46738 = CARTESIAN_POINT ( 'NONE',  ( 16.68750000122903288, -4.330127018922194537, 2.499999999999995559 ) ) ;
#46739 = CARTESIAN_POINT ( 'NONE',  ( 4.546875000614517326, 6.054752690667223547, 3.707466751127219781E-16 ) ) ;
#46740 = CARTESIAN_POINT ( 'NONE',  ( 8.503125000614515372, 4.541064518000418104, -2.621784821874998173 ) ) ;
#46741 = CARTESIAN_POINT ( 'NONE',  ( -4.000000000000000888, 13.60624999877096641, 32.30940107675850470 ) ) ;
#46742 = CARTESIAN_POINT ( 'NONE',  ( 24.54375000122903572, 5.773502691896255534, 3.535250795749688894E-16 ) ) ;
#46743 = CARTESIAN_POINT ( 'NONE',  ( 17.55937500061451573, 4.541064518000418104, -2.621784821874998173 ) ) ;
#46744 = CARTESIAN_POINT ( 'NONE',  ( 1.071796769724493892, 17.72990381179669583, 26.00000000000000711 ) ) ;
#46745 = ORIENTED_EDGE ( 'NONE', *, *, #73012, .T. ) ;
#46746 = CARTESIAN_POINT ( 'NONE',  ( 25.52812500061451573, 6.421520780324663323E-16, -5.243569643749999010 ) ) ;
#46747 = CARTESIAN_POINT ( 'NONE',  ( 10.07812500061451644, -4.541064518000419881, 2.621784821874995952 ) ) ;
#46748 = CARTESIAN_POINT ( 'NONE',  ( 26.70937500061451431, 0.000000000000000000, 5.243569643749999010 ) ) ;
#46749 = CARTESIAN_POINT ( 'NONE',  ( 10.97812500061451679, -4.541064518000419881, 2.621784821874995952 ) ) ;
#46750 = CARTESIAN_POINT ( 'NONE',  ( 28.91250000000000497, 2.886751345948104674, -5.000000000000039968 ) ) ;
#46751 = CARTESIAN_POINT ( 'NONE',  ( 11.36250000122903536, -4.330127018922190985, -2.500000000000001332 ) ) ;
#46752 = CARTESIAN_POINT ( 'NONE',  ( 24.96562500061451573, -6.054752690667223547, -1.112240025338166033E-15 ) ) ;
#46753 = CARTESIAN_POINT ( 'NONE',  ( 4.243569643749999898, 14.17812500061451608, -30.00000000000000000 ) ) ;
#46754 = CARTESIAN_POINT ( 'NONE',  ( 13.01250000122903394, 0.000000000000000000, 4.999999999999998224 ) ) ;
#46755 = CARTESIAN_POINT ( 'NONE',  ( 21.81562500061451004, -6.054752690667223547, -1.112240025338166033E-15 ) ) ;
#46756 = CARTESIAN_POINT ( 'NONE',  ( 10.35000000000000142, -4.330127018922190985, -2.500000000000001332 ) ) ;
#46757 = CARTESIAN_POINT ( 'NONE',  ( 19.19062500061452070, -3.027376345333610441, -5.243569643749999898 ) ) ;
#46758 = CARTESIAN_POINT ( 'NONE',  ( 5.409375000614516260, 4.541064518000418104, -2.621784821874998173 ) ) ;
#46759 = EDGE_CURVE ( 'NONE', #71649, #54715, #20714, .T. ) ;
#46760 = CARTESIAN_POINT ( 'NONE',  ( 20.99999999999999645, 0.000000000000000000, 4.999999999999998224 ) ) ;
#46761 = CARTESIAN_POINT ( 'NONE',  ( 14.66250000122903252, 4.330127018922192761, -2.499999999999997780 ) ) ;
#46762 = CARTESIAN_POINT ( 'NONE',  ( 10.52812500061451750, -4.541064518000419881, 2.621784821874995952 ) ) ;
#46763 = CARTESIAN_POINT ( 'NONE',  ( 15.66562500061451857, 3.027376345333613106, -5.243569643749998122 ) ) ;
#46764 = CARTESIAN_POINT ( 'NONE',  ( 24.82500000122902861, -5.773502691896255534, -1.060575238724906372E-15 ) ) ;
#46765 = CARTESIAN_POINT ( 'NONE',  ( 24.34687500061451715, 6.054752690667223547, 3.707466751127219781E-16 ) ) ;
#46766 = FACE_OUTER_BOUND ( 'NONE', #32860, .T. ) ;
#46767 = CARTESIAN_POINT ( 'NONE',  ( 8.250000001229034652, -2.886751345948125991, -5.000000000000000000 ) ) ;
#46768 = CARTESIAN_POINT ( 'NONE',  ( 10.02187500061451964, 3.027376345333611329, 5.243569643749999010 ) ) ;
#46769 = CARTESIAN_POINT ( 'NONE',  ( 24.94687500061451502, -3.027376345333614438, 5.243569643749998122 ) ) ;
#46770 = CARTESIAN_POINT ( 'NONE',  ( 3.646875000614520079, 6.054752690667223547, 3.707466751127219781E-16 ) ) ;
#46771 = CARTESIAN_POINT ( 'NONE',  ( 20.16562500061451146, 3.027376345333613106, -5.243569643749998122 ) ) ;
#46772 = CARTESIAN_POINT ( 'NONE',  ( 25.47187500061451715, -6.054752690667223547, -1.112240025338166033E-15 ) ) ;
#46773 = CARTESIAN_POINT ( 'NONE',  ( -3.756430356250000990, 16.61562499938548143, 32.16877607737301048 ) ) ;
#46774 = DIRECTION ( 'NONE',  ( 0.000000000000000000, 0.000000000000000000, -1.000000000000000000 ) ) ;
#46775 = VECTOR ( 'NONE', #46577, 1000.000000000000000 ) ;
#46776 = CARTESIAN_POINT ( 'NONE',  ( 8.259375000614518569, 0.000000000000000000, 5.243569643749999010 ) ) ;
#46777 = CARTESIAN_POINT ( 'NONE',  ( 17.69062500061451715, -3.027376345333614438, 5.243569643749998122 ) ) ;
#46778 = ORIENTED_EDGE ( 'NONE', *, *, #1971, .F. ) ;
#46779 = DIRECTION ( 'NONE',  ( -0.000000000000000000, -1.000000000000000000, -0.000000000000000000 ) ) ;
#46780 = CARTESIAN_POINT ( 'NONE',  ( 26.87812500061451360, 6.421520780324663323E-16, -5.243569643749999010 ) ) ;
#46781 = CARTESIAN_POINT ( 'NONE',  ( 5.146875000614517859, -3.027376345333614438, 5.243569643749998122 ) ) ;
#46782 = LINE ( 'NONE', #69317, #46639 ) ;
#46783 = DIRECTION ( 'NONE',  ( 0.000000000000000000, 0.000000000000000000, 1.000000000000000000 ) ) ;
#46784 = CARTESIAN_POINT ( 'NONE',  ( 17.25000000000000000, 4.330127018922192761, -2.499999999999997780 ) ) ;
#46785 = CARTESIAN_POINT ( 'NONE',  ( 20.76562500061451644, 3.027376345333611329, 5.243569643749999010 ) ) ;
#46786 = ORIENTED_EDGE ( 'NONE', *, *, #63206, .T. ) ;
#46787 = CARTESIAN_POINT ( 'NONE',  ( 25.01249999999999929, 2.886751345948126879, 4.999999999999999112 ) ) ;
#46788 = CARTESIAN_POINT ( 'NONE',  ( 27.30937500061451573, -4.541064518000417216, -2.621784821875001281 ) ) ;
#46789 = VERTEX_POINT ( 'NONE', #9854 ) ;
#46790 = CARTESIAN_POINT ( 'NONE',  ( 12.77812500061451750, -4.541064518000419881, 2.621784821874995952 ) ) ;
#46791 = CARTESIAN_POINT ( 'NONE',  ( 5.203125000614518214, -4.541064518000417216, -2.621784821875001281 ) ) ;
#46792 = CARTESIAN_POINT ( 'NONE',  ( 15.68437500061451750, 5.492252693125287522, 3.363034840372157021E-16 ) ) ;
#46793 = CARTESIAN_POINT ( 'NONE',  ( 28.75312500061451715, 4.541064518000418104, -2.621784821874998173 ) ) ;
#46794 = CARTESIAN_POINT ( 'NONE',  ( 15.90000000122903501, -2.886751345948125991, -5.000000000000000000 ) ) ;
#46795 = CARTESIAN_POINT ( 'NONE',  ( 22.53750000000000142, -2.886751345948125991, -5.000000000000000000 ) ) ;
#46796 = CARTESIAN_POINT ( 'NONE',  ( 29.69999999999999574, -4.330127018922190985, -2.500000000000001332 ) ) ;
#46797 = CARTESIAN_POINT ( 'NONE',  ( 4.209375000614516971, 0.000000000000000000, 5.243569643749999010 ) ) ;
#46798 = CARTESIAN_POINT ( 'NONE',  ( 9.571875000614518569, 3.027376345333611329, 5.243569643749999010 ) ) ;
#46799 = CARTESIAN_POINT ( 'NONE',  ( 20.52187500061451786, -6.054752690667223547, -1.112240025338166033E-15 ) ) ;
#46800 = CARTESIAN_POINT ( 'NONE',  ( 4.196151849995945149, -2.718880220196457476, -4.196151849995952254 ) ) ;
#46801 = ORIENTED_EDGE ( 'NONE', *, *, #47241, .F. ) ;
#46802 = CARTESIAN_POINT ( 'NONE',  ( 29.65312500061451573, 4.541064518000418104, -2.621784821874998173 ) ) ;
#46803 = CARTESIAN_POINT ( 'NONE',  ( 3.862500000000001155, 2.886751345948126879, 4.999999999999999112 ) ) ;
#46804 = CARTESIAN_POINT ( 'NONE',  ( 5.259375000614518569, -4.541064518000417216, -2.621784821875001281 ) ) ;
#46805 = CARTESIAN_POINT ( 'NONE',  ( 16.23750000000000071, -2.886751345948125991, -5.000000000000000000 ) ) ;
#46806 = CARTESIAN_POINT ( 'NONE',  ( 13.41562500061451502, 3.027376345333613106, -5.243569643749998122 ) ) ;
#46807 = CARTESIAN_POINT ( 'NONE',  ( -1.999999999999999112, 19.40000000000000213, 26.53589838486224650 ) ) ;
#46808 = DIRECTION ( 'NONE',  ( 0.000000000000000000, 0.000000000000000000, 1.000000000000000000 ) ) ;
#46809 = CARTESIAN_POINT ( 'NONE',  ( 20.36250000122903359, -4.330127018922190985, -2.500000000000001332 ) ) ;
#46810 = CARTESIAN_POINT ( 'NONE',  ( 0.8114860633430669434, 9.969066991719973458, 24.05167508342340454 ) ) ;
#46811 = CARTESIAN_POINT ( 'NONE',  ( 20.07187500061451857, -5.492252693125287522, -1.008910452111647106E-15 ) ) ;
#46812 = CARTESIAN_POINT ( 'NONE',  ( 6.778125000614518392, 4.541064518000418104, 2.621784821874999949 ) ) ;
#46813 = CARTESIAN_POINT ( 'NONE',  ( 23.93437500061451573, 4.541064518000418104, 2.621784821874999949 ) ) ;
#46814 = CARTESIAN_POINT ( 'NONE',  ( -4.243569643749997233, 19.44687500061451502, 32.45002607614398471 ) ) ;
#46815 = CARTESIAN_POINT ( 'NONE',  ( 26.74687500061451573, -3.027376345333614438, 5.243569643749998122 ) ) ;
#46816 = CARTESIAN_POINT ( 'NONE',  ( 6.487499999999999822, 5.773502691896255534, 3.535250795749688894E-16 ) ) ;
#46817 = CARTESIAN_POINT ( 'NONE',  ( -3.999999999999999112, 14.26250000122903572, 30.00000000000000000 ) ) ;
#46818 = CARTESIAN_POINT ( 'NONE',  ( 15.47812500061451679, -4.541064518000419881, 2.621784821874995952 ) ) ;
#46819 = CARTESIAN_POINT ( 'NONE',  ( 7.050000001229036251, 5.773502691896255534, 3.535250795749688894E-16 ) ) ;
#46820 = EDGE_CURVE ( 'NONE', #25475, #38626, #64902, .T. ) ;
#46821 = CARTESIAN_POINT ( 'NONE',  ( 18.08437500061451431, 4.541064518000418104, 2.621784821874999949 ) ) ;
#46822 = CARTESIAN_POINT ( 'NONE',  ( 11.14687500061451608, -3.027376345333610441, -5.243569643749999898 ) ) ;
#46823 = DIRECTION ( 'NONE',  ( 0.000000000000000000, 0.000000000000000000, 1.000000000000000000 ) ) ;
#46824 = VERTEX_POINT ( 'NONE', #4331 ) ;
#46825 = CARTESIAN_POINT ( 'NONE',  ( 11.87812500061451537, -4.541064518000419881, 2.621784821874995952 ) ) ;
#46826 = CARTESIAN_POINT ( 'NONE',  ( 10.65000000000000036, 0.000000000000000000, 4.999999999999998224 ) ) ;
#46827 = CARTESIAN_POINT ( 'NONE',  ( 24.48750000122903359, 6.123233995736764310E-16, -4.999999999999998224 ) ) ;
#46828 = CARTESIAN_POINT ( 'NONE',  ( 13.09687500061451892, 6.054752690667223547, 3.707466751127219781E-16 ) ) ;
#46829 = CARTESIAN_POINT ( 'NONE',  ( 13.82812500061451466, 6.421520780324663323E-16, -5.243569643749999010 ) ) ;
#46830 = CARTESIAN_POINT ( 'NONE',  ( 1.071796769724491893, 18.78259618943233278, -26.00000000000000355 ) ) ;
#46831 = CARTESIAN_POINT ( 'NONE',  ( 24.57187500061451502, -6.054752690667223547, -1.112240025338166033E-15 ) ) ;
#46832 = CARTESIAN_POINT ( 'NONE',  ( 0.000000000000000000, 20.00000000000000000, 30.00000000000000000 ) ) ;
#46833 = CARTESIAN_POINT ( 'NONE',  ( 0.6522905807966048464, 20.75364847883808395, 33.69936292076899065 ) ) ;
#46834 = CARTESIAN_POINT ( 'NONE',  ( 14.77500000000000036, -4.330127018922194537, 2.499999999999995559 ) ) ;
#46835 = CARTESIAN_POINT ( 'NONE',  ( 9.001249775931846008E-16, 16.37187500061451573, -25.09994784771203058 ) ) ;
#46836 = CARTESIAN_POINT ( 'NONE',  ( 15.49687500061451750, -3.027376345333614438, 5.243569643749998122 ) ) ;
#46837 = CARTESIAN_POINT ( 'NONE',  ( 18.33750000122903501, 4.330127018922191873, 2.499999999999999556 ) ) ;
#46838 = CARTESIAN_POINT ( 'NONE',  ( 13.20937500061451786, 0.000000000000000000, 5.243569643749999010 ) ) ;
#46839 = CARTESIAN_POINT ( 'NONE',  ( -0.7368805616696193495, 9.859898480082234684, 25.82089837893477480 ) ) ;
#46840 = CARTESIAN_POINT ( 'NONE',  ( 19.76250000122903216, 0.000000000000000000, 4.999999999999998224 ) ) ;
#46841 = CARTESIAN_POINT ( 'NONE',  ( 15.44062500061451537, -3.027376345333614438, 5.243569643749998122 ) ) ;
#46842 = ORIENTED_EDGE ( 'NONE', *, *, #22509, .F. ) ;
#46843 = VERTEX_POINT ( 'NONE', #66372 ) ;
#46844 = CARTESIAN_POINT ( 'NONE',  ( 18.18750000000000000, 5.773502691896255534, 3.535250795749688894E-16 ) ) ;
#46845 = CARTESIAN_POINT ( 'NONE',  ( -4.243569643749999898, 19.83125000061451715, 30.00000000000000000 ) ) ;
#46846 = CARTESIAN_POINT ( 'NONE',  ( 13.09687500061451537, 6.054752690667223547, 3.707466751127219781E-16 ) ) ;
#46847 = CARTESIAN_POINT ( 'NONE',  ( 3.022718161895720623, 3.982892879517589968, -3.221804244138950502 ) ) ;
#46848 = CARTESIAN_POINT ( 'NONE',  ( 13.76250000122903394, 4.330127018922192761, -2.499999999999997780 ) ) ;
#46849 = CARTESIAN_POINT ( 'NONE',  ( 19.80000000122903359, -2.886751345948129988, 4.999999999999997335 ) ) ;
#46850 = CARTESIAN_POINT ( 'NONE',  ( 19.04062500061451146, -3.027376345333614438, 5.243569643749998122 ) ) ;
#46851 = CARTESIAN_POINT ( 'NONE',  ( 23.61562500061451431, -6.054752690667223547, -1.112240025338166033E-15 ) ) ;
#46852 = CARTESIAN_POINT ( 'NONE',  ( 3.740625000614516527, -3.027376345333614438, 5.243569643749998122 ) ) ;
#46853 = CARTESIAN_POINT ( 'NONE',  ( 27.75000000000000000, 0.000000000000000000, 4.999999999999998224 ) ) ;
#46854 = CARTESIAN_POINT ( 'NONE',  ( 27.80625000122903145, 0.000000000000000000, 4.999999999999998224 ) ) ;
#46855 = CARTESIAN_POINT ( 'NONE',  ( 9.721875000614517148, -5.492252693125287522, -1.008910452111647106E-15 ) ) ;
#46856 = DIRECTION ( 'NONE',  ( 0.000000000000000000, 0.000000000000000000, -1.000000000000000000 ) ) ;
#46857 = LINE ( 'NONE', #47215, #13425 ) ;
#46858 = CARTESIAN_POINT ( 'NONE',  ( -3.000416591977282496E-16, 16.59687500061452070, -34.90005215228797653 ) ) ;
#46859 = EDGE_CURVE ( 'NONE', #27013, #47688, #21293, .T. ) ;
#46860 = CARTESIAN_POINT ( 'NONE',  ( 2.775000001229033675, -5.773502691896255534, -1.060575238724906372E-15 ) ) ;
#46861 = CARTESIAN_POINT ( 'NONE',  ( 4.912499999999999645, -5.773502691896255534, -1.060575238724906372E-15 ) ) ;
#46862 = CARTESIAN_POINT ( 'NONE',  ( 3.709174336338540989, 3.352913023424228811, 4.031500572517469294 ) ) ;
#46863 = CARTESIAN_POINT ( 'NONE',  ( 8.896875000614517859, -3.027376345333610441, -5.243569643749999898 ) ) ;
#46864 = CARTESIAN_POINT ( 'NONE',  ( 28.19062500061451715, -3.027376345333610441, -5.243569643749999898 ) ) ;
#46865 = FACE_OUTER_BOUND ( 'NONE', #54779, .T. ) ;
#46866 = CARTESIAN_POINT ( 'NONE',  ( -5.678847837524354070, 8.233079231341507764, -31.97529239793390232 ) ) ;
#46867 = CARTESIAN_POINT ( 'NONE',  ( 7.359375000614516438, 0.000000000000000000, 5.243569643749999010 ) ) ;
#46868 = CARTESIAN_POINT ( 'NONE',  ( 10.80937500061451928, 4.541064518000418104, -2.621784821874998173 ) ) ;
#46869 = CARTESIAN_POINT ( 'NONE',  ( 7.124999999999999112, -4.330127018922194537, 2.499999999999995559 ) ) ;
#46870 = VECTOR ( 'NONE', #47042, 1000.000000000000000 ) ;
#46871 = CARTESIAN_POINT ( 'NONE',  ( 4.243569643749999010, 15.56562500061459353, 27.54997392385601174 ) ) ;
#46872 = CARTESIAN_POINT ( 'NONE',  ( 4.818692141996692158, -1.334243621178544226, 4.818692141997074074 ) ) ;
#46873 = CARTESIAN_POINT ( 'NONE',  ( 6.187500000000002665, -2.886751345948129988, 4.999999999999997335 ) ) ;
#46874 = CARTESIAN_POINT ( 'NONE',  ( 14.37187500061451573, 4.119189519843966529, 2.378215178124999607 ) ) ;
#46875 = CARTESIAN_POINT ( 'NONE',  ( 23.05312500061451431, 0.000000000000000000, 5.243569643749999010 ) ) ;
#46876 = CARTESIAN_POINT ( 'NONE',  ( 13.94062500061451892, 6.054752690667223547, 3.707466751127219781E-16 ) ) ;
#46877 = CARTESIAN_POINT ( 'NONE',  ( 25.13437500061451857, 5.492252693125287522, 3.363034840372157021E-16 ) ) ;
#46878 = CARTESIAN_POINT ( 'NONE',  ( 8.559375000614515727, 4.541064518000418104, -2.621784821874998173 ) ) ;
#46879 = CARTESIAN_POINT ( 'NONE',  ( 26.66250000000000142, 2.886751345948129099, -4.999999999999998224 ) ) ;
#46880 = CARTESIAN_POINT ( 'NONE',  ( 22.80000000122903359, 5.773502691896255534, 3.535250795749688894E-16 ) ) ;
#46881 = CARTESIAN_POINT ( 'NONE',  ( 11.36250000122903536, -4.330127018922190985, -2.500000000000001332 ) ) ;
#46882 = CARTESIAN_POINT ( 'NONE',  ( 12.15937500061451892, 4.541064518000418104, -2.621784821874998173 ) ) ;
#46883 = CARTESIAN_POINT ( 'NONE',  ( 27.08437500061451786, 4.541064518000418104, 2.621784821874999949 ) ) ;
#46884 = CARTESIAN_POINT ( 'NONE',  ( 3.684375000614518836, 4.541064518000418104, 2.621784821874999949 ) ) ;
#46885 = DIRECTION ( 'NONE',  ( -1.000000000000000000, -0.000000000000000000, -0.000000000000000000 ) ) ;
#46886 = CARTESIAN_POINT ( 'NONE',  ( 18.94687500061451502, 6.054752690667223547, 3.707466751127219781E-16 ) ) ;
#46887 = CARTESIAN_POINT ( 'NONE',  ( 11.55937500061451928, -4.541064518000417216, -2.621784821875001281 ) ) ;
#46888 = CARTESIAN_POINT ( 'NONE',  ( 1.878215178124997609, 19.42812499938548143, 33.25316411605952993 ) ) ;
#46889 = CARTESIAN_POINT ( 'NONE',  ( 24.63749999999999574, -2.886751345948129988, 4.999999999999997335 ) ) ;
#46890 = CARTESIAN_POINT ( 'NONE',  ( 3.999999999999998668, 13.81249999999999822, 32.30940107675850470 ) ) ;
#46891 = CARTESIAN_POINT ( 'NONE',  ( 2.121784821875001281, 12.35937500061451821, -26.32496088578401938 ) ) ;
#46892 = CARTESIAN_POINT ( 'NONE',  ( 28.32187500061451502, 2.746126346562645981, -4.756430356249997438 ) ) ;
#46893 = CARTESIAN_POINT ( 'NONE',  ( 15.51562500061451644, -6.054752690667223547, -1.112240025338166033E-15 ) ) ;
#46894 = CARTESIAN_POINT ( 'NONE',  ( 4.875000000000000888, -4.330127018922194537, 2.499999999999995559 ) ) ;
#46895 = DIRECTION ( 'NONE',  ( 0.000000000000000000, 0.000000000000000000, -1.000000000000000000 ) ) ;
#46896 = CYLINDRICAL_SURFACE ( 'NONE', #20808, 4.999999999999998224 ) ;
#46897 = CARTESIAN_POINT ( 'NONE',  ( 13.83749999999999858, -2.886751345948129988, 4.999999999999997335 ) ) ;
#46898 = CARTESIAN_POINT ( 'NONE',  ( 4.243569643749999898, 10.09062500061451928, 32.45002607614398471 ) ) ;
#46899 = CARTESIAN_POINT ( 'NONE',  ( 13.31250000122903288, 4.330127018922192761, -2.499999999999997780 ) ) ;
#46900 = CARTESIAN_POINT ( 'NONE',  ( 24.23437500061451644, 6.421520780324663323E-16, -5.243569643749999010 ) ) ;
#46901 = ORIENTED_EDGE ( 'NONE', *, *, #40917, .F. ) ;
#46902 = CARTESIAN_POINT ( 'NONE',  ( 18.89062500061451644, 6.054752690667223547, 3.707466751127219781E-16 ) ) ;
#46903 = CARTESIAN_POINT ( 'NONE',  ( 4.453125000614517326, 4.541064518000418104, -2.621784821874998173 ) ) ;
#46904 = CARTESIAN_POINT ( 'NONE',  ( 19.50937500061451857, 0.000000000000000000, 5.243569643749999010 ) ) ;
#46905 = CARTESIAN_POINT ( 'NONE',  ( 5.325000000000000178, -4.330127018922194537, 2.499999999999995559 ) ) ;
#46906 = CARTESIAN_POINT ( 'NONE',  ( 8.090625000614515727, 6.054752690667223547, 3.707466751127219781E-16 ) ) ;
#46907 = CARTESIAN_POINT ( 'NONE',  ( 23.05312500061451431, 0.000000000000000000, 5.243569643749999010 ) ) ;
#46908 = CARTESIAN_POINT ( 'NONE',  ( 4.243569643749999898, 15.97812500061451857, 30.00000000000000000 ) ) ;
#46909 = CARTESIAN_POINT ( 'NONE',  ( 19.05000000122903359, -2.886751345948125991, -5.000000000000000000 ) ) ;
#46910 = CARTESIAN_POINT ( 'NONE',  ( 11.22187500061451892, 2.746126346562645981, -4.756430356249997438 ) ) ;
#46911 = CARTESIAN_POINT ( 'NONE',  ( 10.04062500061451679, -3.027376345333614438, 5.243569643749998122 ) ) ;
#46912 = CARTESIAN_POINT ( 'NONE',  ( 3.121875000614518836, 3.027376345333613106, -5.243569643749998122 ) ) ;
#46913 = CARTESIAN_POINT ( 'NONE',  ( 28.26562500061451289, 3.027376345333613106, -5.243569643749998122 ) ) ;
#46914 = ADVANCED_FACE ( 'NONE', ( #38286, #60814, #55293 ), #4687, .F. ) ;
#46915 = CARTESIAN_POINT ( 'NONE',  ( 24.42187500061451999, 3.027376345333611329, 5.243569643749999010 ) ) ;
#46916 = CARTESIAN_POINT ( 'NONE',  ( 15.29062500061451679, 6.054752690667223547, 3.707466751127219781E-16 ) ) ;
#46917 = CARTESIAN_POINT ( 'NONE',  ( 25.76250000122903216, -4.330127018922190985, -2.500000000000001332 ) ) ;
#46918 = CARTESIAN_POINT ( 'NONE',  ( 25.07812500061451644, 6.421520780324663323E-16, -5.243569643749999010 ) ) ;
#46919 = CARTESIAN_POINT ( 'NONE',  ( 18.38437500061451857, 6.421520780324663323E-16, -5.243569643749999010 ) ) ;
#46920 = CARTESIAN_POINT ( 'NONE',  ( 14.72812500061451679, 6.421520780324663323E-16, -5.243569643749999010 ) ) ;
#46921 = CARTESIAN_POINT ( 'NONE',  ( -2.121784821874996840, 17.68437500061451928, 33.67503911421598417 ) ) ;
#46922 = CARTESIAN_POINT ( 'NONE',  ( 23.16562500061451502, -6.054752690667223547, -1.112240025338166033E-15 ) ) ;
#46923 = CARTESIAN_POINT ( 'NONE',  ( 2.662500001229036073, 0.000000000000000000, 4.999999999999998224 ) ) ;
#46924 = VERTEX_POINT ( 'NONE', #12031 ) ;
#46925 = CARTESIAN_POINT ( 'NONE',  ( 24.60000000000000142, 0.000000000000000000, 4.999999999999998224 ) ) ;
#46926 = CARTESIAN_POINT ( 'NONE',  ( -3.999999999999999556, 10.96250000000000213, -32.30940107675850470 ) ) ;
#46927 = CARTESIAN_POINT ( 'NONE',  ( -3.756430356249999214, 20.14062499938548356, 27.83122392262697531 ) ) ;
#46928 = CARTESIAN_POINT ( 'NONE',  ( 28.67812500061451431, 6.421520780324663323E-16, -5.243569643749999010 ) ) ;
#46929 = CARTESIAN_POINT ( 'NONE',  ( 7.490625000614516082, -3.027376345333610441, -5.243569643749999898 ) ) ;
#46930 = CARTESIAN_POINT ( 'NONE',  ( 22.50000000122903288, -2.886751345948129988, 4.999999999999997335 ) ) ;
#46931 = VECTOR ( 'NONE', #6191, 1000.000000000000000 ) ;
#46932 = CARTESIAN_POINT ( 'NONE',  ( 27.21562500061451928, -6.054752690667223547, -1.112240025338166033E-15 ) ) ;
#46933 = CARTESIAN_POINT ( 'NONE',  ( 26.02499999999999858, -4.330127018922194537, 2.499999999999995559 ) ) ;
#46934 = APPLICATION_CONTEXT ( 'automotive_design' ) ;
#46935 = CARTESIAN_POINT ( 'NONE',  ( -2.828200636599751609E-16, 16.40000000122903501, -34.61880215351700230 ) ) ;
#46936 = CARTESIAN_POINT ( 'NONE',  ( -1.071796769724491005, 12.37009619066136956, 26.00000000000000355 ) ) ;
#46937 = CARTESIAN_POINT ( 'NONE',  ( 10.52812500061451750, -4.541064518000419881, 2.621784821874995952 ) ) ;
#46938 =( BOUNDED_CURVE ( )  B_SPLINE_CURVE ( 3, ( #31359, #55358, #10651, #45003 ),
 .UNSPECIFIED., .F., .F. ) 
 B_SPLINE_CURVE_WITH_KNOTS ( ( 4, 4 ),
 ( 0.5446367559021773053, 0.5855140179436351122 ),
 .UNSPECIFIED. ) 
 CURVE ( )  GEOMETRIC_REPRESENTATION_ITEM ( )  RATIONAL_B_SPLINE_CURVE ( ( 1.000000000000000000, 0.9998607589679524565, 0.9998607589679524565, 1.000000000000000000 ) ) 
 REPRESENTATION_ITEM ( '' )  );
#46939 = ORIENTED_EDGE ( 'NONE', *, *, #22648, .T. ) ;
#46940 = CARTESIAN_POINT ( 'NONE',  ( 24.96562500061451573, -6.054752690667223547, -1.112240025338166033E-15 ) ) ;
#46941 = CARTESIAN_POINT ( 'NONE',  ( 7.265625000614516438, 3.027376345333611329, 5.243569643749999010 ) ) ;
#46942 = CARTESIAN_POINT ( 'NONE',  ( 3.103125000614517237, 4.541064518000418104, -2.621784821874998173 ) ) ;
#46943 = CARTESIAN_POINT ( 'NONE',  ( 15.94687500061451502, -2.746126346562646425, 4.756430356249996549 ) ) ;
#46944 = CARTESIAN_POINT ( 'NONE',  ( 12.97499999999999964, -4.330127018922194537, 2.499999999999995559 ) ) ;
#46945 = CARTESIAN_POINT ( 'NONE',  ( 14.02499999999999858, 6.123233995736764310E-16, -4.999999999999998224 ) ) ;
#46946 = CARTESIAN_POINT ( 'NONE',  ( 12.75937500061451857, 0.000000000000000000, 5.243569643749999010 ) ) ;
#46947 = CARTESIAN_POINT ( 'NONE',  ( 9.637500001229033941, 6.123233995736764310E-16, -4.999999999999998224 ) ) ;
#46948 = CARTESIAN_POINT ( 'NONE',  ( 17.67187500061451644, 3.027376345333611329, 5.243569643749999010 ) ) ;
#46949 = CARTESIAN_POINT ( 'NONE',  ( 18.14999999999999858, 4.330127018922192761, -2.499999999999997780 ) ) ;
#46950 = CARTESIAN_POINT ( 'NONE',  ( 8.821875000614518569, -6.054752690667223547, -1.112240025338166033E-15 ) ) ;
#46951 = CARTESIAN_POINT ( 'NONE',  ( 4.243569643749999898, 10.54062500061451679, -27.54997392385601529 ) ) ;
#46952 = DIRECTION ( 'NONE',  ( -1.000000000000000000, -0.000000000000000000, -0.000000000000000000 ) ) ;
#46953 = CARTESIAN_POINT ( 'NONE',  ( 22.65937500061451004, -5.492252693125287522, -1.008910452111647106E-15 ) ) ;
#46954 = VERTEX_POINT ( 'NONE', #50480 ) ;
#46955 = EDGE_CURVE ( 'NONE', #41820, #68271, #62187, .T. ) ;
#46956 = CARTESIAN_POINT ( 'NONE',  ( 23.57812500061451289, -4.541064518000419881, 2.621784821874995952 ) ) ;
#46957 = LINE ( 'NONE', #1535, #52842 ) ;
#46958 = CARTESIAN_POINT ( 'NONE',  ( 27.34687500061451360, -3.027376345333610441, -5.243569643749999898 ) ) ;
#46959 = CARTESIAN_POINT ( 'NONE',  ( 20.96250000000000213, 2.886751345948126879, 4.999999999999999112 ) ) ;
#46960 = CARTESIAN_POINT ( 'NONE',  ( 6.590625000614518392, -3.027376345333610441, -5.243569643749999898 ) ) ;
#46961 = CARTESIAN_POINT ( 'NONE',  ( 25.09687500061451360, 4.119189519843966529, -2.378215178124998275 ) ) ;
#46962 = CARTESIAN_POINT ( 'NONE',  ( 16.39687500061451786, -3.027376345333614438, 5.243569643749998122 ) ) ;
#46963 = CARTESIAN_POINT ( 'NONE',  ( 9.684375000614517504, -2.746126346562641984, -4.756430356249999214 ) ) ;
#46964 = CARTESIAN_POINT ( 'NONE',  ( 29.02500000122903145, 2.886751345948129099, -4.999999999999998224 ) ) ;
#46965 = CARTESIAN_POINT ( 'NONE',  ( 7.509375000614517681, -4.541064518000417216, -2.621784821875001281 ) ) ;
#46966 = ORIENTED_EDGE ( 'NONE', *, *, #7459, .F. ) ;
#46967 = CARTESIAN_POINT ( 'NONE',  ( 19.50937500061451857, 0.000000000000000000, 5.243569643749999010 ) ) ;
#46968 = CARTESIAN_POINT ( 'NONE',  ( -2.443018120338280585, 25.33977806483805040, 26.82191794298074328 ) ) ;
#46969 = CARTESIAN_POINT ( 'NONE',  ( 26.21249999999999858, 2.886751345948129099, -4.999999999999998224 ) ) ;
#46970 = CARTESIAN_POINT ( 'NONE',  ( 29.07187500061451502, -6.054752690667223547, -1.112240025338166033E-15 ) ) ;
#46971 = CARTESIAN_POINT ( 'NONE',  ( 19.34999999999999787, -4.330127018922190985, -2.500000000000001332 ) ) ;
#46972 = DIRECTION ( 'NONE',  ( -1.000000000000000000, 0.000000000000000000, 0.000000000000000000 ) ) ;
#46973 = EDGE_LOOP ( 'NONE', ( #27443, #56593, #33299, #39589 ) ) ;
#46974 = CARTESIAN_POINT ( 'NONE',  ( 10.98750000000000071, 5.773502691896255534, 3.535250795749688894E-16 ) ) ;
#46975 = CARTESIAN_POINT ( 'NONE',  ( 12.30937500061451750, -5.492252693125287522, -1.008910452111647106E-15 ) ) ;
#46976 = CARTESIAN_POINT ( 'NONE',  ( 21.47812500061451502, 6.421520780324663323E-16, -5.243569643749999010 ) ) ;
#46977 = CARTESIAN_POINT ( 'NONE',  ( 14.28750000000000142, -2.886751345948129988, 4.999999999999997335 ) ) ;
#46978 = CARTESIAN_POINT ( 'NONE',  ( 8.550000001229031810, -2.886751345948129988, 4.999999999999997335 ) ) ;
#46979 = CARTESIAN_POINT ( 'NONE',  ( 6.328125000614515550, 4.541064518000418104, 2.621784821874999949 ) ) ;
#46980 = CARTESIAN_POINT ( 'NONE',  ( 20.77500000000000213, 6.123233995736764310E-16, -4.999999999999998224 ) ) ;
#46981 = CARTESIAN_POINT ( 'NONE',  ( 21.81562500061451004, -6.054752690667223547, -1.112240025338166033E-15 ) ) ;
#46982 = CARTESIAN_POINT ( 'NONE',  ( 12.11250000000000249, -5.773502691896255534, -1.060575238724906372E-15 ) ) ;
#46983 = CARTESIAN_POINT ( 'NONE',  ( 24.60000000122903430, 5.773502691896255534, 3.535250795749688894E-16 ) ) ;
#46984 = CARTESIAN_POINT ( 'NONE',  ( -1.878215178125001827, 18.34062499938548285, 33.25316411605952283 ) ) ;
#46985 = CARTESIAN_POINT ( 'NONE',  ( 5.962500000000002132, 2.886751345948129099, -4.999999999999998224 ) ) ;
#46986 = ORIENTED_EDGE ( 'NONE', *, *, #60362, .F. ) ;
#46987 = CARTESIAN_POINT ( 'NONE',  ( 22.45312500061451644, 4.541064518000418104, -2.621784821874998173 ) ) ;
#46988 = CARTESIAN_POINT ( 'NONE',  ( 26.76562500061451644, -6.054752690667223547, -1.112240025338166033E-15 ) ) ;
#46989 = CARTESIAN_POINT ( 'NONE',  ( 27.45937500061451786, 4.541064518000418104, -2.621784821874998173 ) ) ;
#46990 = CARTESIAN_POINT ( 'NONE',  ( 14.80312500061451608, 4.541064518000418104, -2.621784821874998173 ) ) ;
#46991 = CARTESIAN_POINT ( 'NONE',  ( 29.81249999999999645, 2.886751345948139313, -4.999999999999980460 ) ) ;
#46992 = CARTESIAN_POINT ( 'NONE',  ( 26.25000000122903288, -2.886751345948125991, -5.000000000000000000 ) ) ;
#46993 = CARTESIAN_POINT ( 'NONE',  ( 19.13437500061451857, -4.119189519843968306, 2.378215178124996054 ) ) ;
#46994 = CARTESIAN_POINT ( 'NONE',  ( 16.07812500061451289, 6.421520780324663323E-16, -5.243569643749999010 ) ) ;
#46995 = CARTESIAN_POINT ( 'NONE',  ( 4.000000000000000000, 14.45000000122903572, -27.69059892324149885 ) ) ;
#46996 = EDGE_CURVE ( 'NONE', #48258, #39103, #30764, .T. ) ;
#46997 = CARTESIAN_POINT ( 'NONE',  ( 3.900000001229034563, 5.773502691896255534, 3.535250795749688894E-16 ) ) ;
#46998 = CARTESIAN_POINT ( 'NONE',  ( 10.88437500061451679, 4.541064518000418104, 2.621784821874999949 ) ) ;
#46999 = CARTESIAN_POINT ( 'NONE',  ( 8.821875000614518569, -6.054752690667223547, -1.112240025338166033E-15 ) ) ;
#47000 = CARTESIAN_POINT ( 'NONE',  ( 18.53437500061451715, 4.541064518000418104, 2.621784821874999949 ) ) ;
#47001 = VERTEX_POINT ( 'NONE', #16840 ) ;
#47002 = CARTESIAN_POINT ( 'NONE',  ( -4.872631645816655421, 8.733424155075979911, 26.49367970277769047 ) ) ;
#47003 = CARTESIAN_POINT ( 'NONE',  ( 23.95312500061451289, 0.000000000000000000, 5.243569643749999010 ) ) ;
#47004 = CARTESIAN_POINT ( 'NONE',  ( 18.12187500061451573, 3.027376345333611329, 5.243569643749999010 ) ) ;
#47005 = CARTESIAN_POINT ( 'NONE',  ( 21.51562500061451644, 3.027376345333613106, -5.243569643749998122 ) ) ;
#47006 = CARTESIAN_POINT ( 'NONE',  ( 30.00000000000000000, 6.123233995736764310E-16, -4.999999999999998224 ) ) ;
#47007 = CARTESIAN_POINT ( 'NONE',  ( 3.999999999999999112, 13.92500000000000071, 30.00000000000000000 ) ) ;
#47008 = CARTESIAN_POINT ( 'NONE',  ( 29.12812500061451715, 6.421520780324663323E-16, -5.243569643749999010 ) ) ;
#47009 = CARTESIAN_POINT ( 'NONE',  ( 9.600000001229034297, -2.886751345948125991, -5.000000000000000000 ) ) ;
#47010 = VERTEX_POINT ( 'NONE', #39765 ) ;
#47011 = CARTESIAN_POINT ( 'NONE',  ( 5.512500001229033941, -4.330127018922190985, -2.500000000000001332 ) ) ;
#47012 = CARTESIAN_POINT ( 'NONE',  ( -2.828200636599751609E-16, 19.43750000000000000, -34.61880215351700230 ) ) ;
#47013 = CARTESIAN_POINT ( 'NONE',  ( 27.48750000122903359, -4.330127018922194537, 2.499999999999995559 ) ) ;
#47014 = CARTESIAN_POINT ( 'NONE',  ( 2.655984681222220721E-16, 13.31562499938548783, 25.66244784525396483 ) ) ;
#47015 = CARTESIAN_POINT ( 'NONE',  ( 9.946875000614516793, 6.054752690667223547, 3.707466751127219781E-16 ) ) ;
#47016 = CARTESIAN_POINT ( 'NONE',  ( 1.626862140677534273E-15, 9.875000001229034652, 34.00000000000000000 ) ) ;
#47017 = CARTESIAN_POINT ( 'NONE',  ( 14.05312500061451431, 0.000000000000000000, 5.243569643749999010 ) ) ;
#47018 = CARTESIAN_POINT ( 'NONE',  ( 10.35937500061451644, 4.541064518000418104, -2.621784821874998173 ) ) ;
#47019 = CARTESIAN_POINT ( 'NONE',  ( 29.25000000122903288, -2.886751345948129988, 4.999999999999997335 ) ) ;
#47020 = CARTESIAN_POINT ( 'NONE',  ( 18.75937500061451857, -4.541064518000417216, -2.621784821875001281 ) ) ;
#47021 = CARTESIAN_POINT ( 'NONE',  ( 7.546875000614517326, -3.027376345333610441, -5.243569643749999898 ) ) ;
#47022 = DIRECTION ( 'NONE',  ( -1.000000000000000000, -0.000000000000000000, -0.000000000000000000 ) ) ;
#47023 = CARTESIAN_POINT ( 'NONE',  ( 8.878125000614515372, 6.421520780324663323E-16, -5.243569643749999010 ) ) ;
#47024 = CARTESIAN_POINT ( 'NONE',  ( 16.52812500061451573, 6.421520780324663323E-16, -5.243569643749999010 ) ) ;
#47025 = ORIENTED_EDGE ( 'NONE', *, *, #561, .F. ) ;
#47026 = CARTESIAN_POINT ( 'NONE',  ( 15.74062500061451608, 6.054752690667223547, 3.707466751127219781E-16 ) ) ;
#47027 = CARTESIAN_POINT ( 'NONE',  ( 11.46562500061451573, -6.054752690667223547, -1.112240025338166033E-15 ) ) ;
#47028 = CARTESIAN_POINT ( 'NONE',  ( 23.59687500061451715, -2.746126346562646425, 4.756430356249996549 ) ) ;
#47029 = CARTESIAN_POINT ( 'NONE',  ( 11.55000000000000071, 0.000000000000000000, 4.999999999999998224 ) ) ;
#47030 = CARTESIAN_POINT ( 'NONE',  ( 7.275000001229035007, -5.773502691896255534, -1.060575238724906372E-15 ) ) ;
#47031 = B_SPLINE_CURVE_WITH_KNOTS ( 'NONE', 3,
 ( #9657, #14086, #32191, #65066, #8927, #4127, #36626, #66169, #42907, #14821 ),
 .UNSPECIFIED., .F., .F.,
 ( 4, 3, 3, 4 ),
 ( 8.949075925690993792E-17, 7.861233265730306976E-05, 0.0001572246084809364789, 0.0003125746657383838330 ),
 .UNSPECIFIED. ) ;
#47032 = CARTESIAN_POINT ( 'NONE',  ( 14.22187500061451537, -6.054752690667223547, -1.112240025338166033E-15 ) ) ;
#47033 = CARTESIAN_POINT ( 'NONE',  ( 17.28750000122903430, 6.123233995736764310E-16, -4.999999999999998224 ) ) ;
#47034 = CARTESIAN_POINT ( 'NONE',  ( 24.03750000000000142, 5.773502691896255534, 3.535250795749688894E-16 ) ) ;
#47035 = CARTESIAN_POINT ( 'NONE',  ( 9.001249775931846008E-16, 19.01562500061451644, -25.09994784771203058 ) ) ;
#47036 = CARTESIAN_POINT ( 'NONE',  ( 4.648177544792955741E-15, 14.58124999877096606, 33.99999999999999289 ) ) ;
#47037 = FACE_OUTER_BOUND ( 'NONE', #9810, .T. ) ;
#47038 = CARTESIAN_POINT ( 'NONE',  ( 1.999999999999998668, 10.96250000122903501, -33.46410161513775705 ) ) ;
#47039 = CARTESIAN_POINT ( 'NONE',  ( 3.927649849665248105, 3.094731086393085917, 3.927649849665248105 ) ) ;
#47040 = CARTESIAN_POINT ( 'NONE',  ( 18.08437500061451431, 4.541064518000418104, 2.621784821874999949 ) ) ;
#47041 = EDGE_CURVE ( 'NONE', #45611, #66904, #55809, .T. ) ;
#47042 = DIRECTION ( 'NONE',  ( -1.000000000000000000, -0.000000000000000000, -0.000000000000000000 ) ) ;
#47043 = CARTESIAN_POINT ( 'NONE',  ( 15.17812500061451608, 6.421520780324663323E-16, -5.243569643749999010 ) ) ;
#47044 = CARTESIAN_POINT ( 'NONE',  ( 8.306250001229031454, 4.330127018922192761, -2.499999999999997780 ) ) ;
#47045 = LINE ( 'NONE', #34498, #37744 ) ;
#47046 = CARTESIAN_POINT ( 'NONE',  ( 24.90937500061451715, 0.000000000000000000, 5.243569643749999010 ) ) ;
#47047 = CARTESIAN_POINT ( 'NONE',  ( 19.35937500061451289, 2.746126346562643317, 4.756430356249998326 ) ) ;
#47048 = CARTESIAN_POINT ( 'NONE',  ( 10.19062500061451892, -3.027376345333610441, -5.243569643749999898 ) ) ;
#47049 = CARTESIAN_POINT ( 'NONE',  ( 14.59687500061452070, -3.027376345333614438, 5.243569643749998122 ) ) ;
#47050 = ORIENTED_EDGE ( 'NONE', *, *, #69367, .T. ) ;
#47051 = CARTESIAN_POINT ( 'NONE',  ( 27.27187500061451431, -6.054752690667223547, -1.112240025338166033E-15 ) ) ;
#47052 = CARTESIAN_POINT ( 'NONE',  ( 27.14062500061451644, -3.027376345333614438, 5.243569643749998122 ) ) ;
#47053 = CARTESIAN_POINT ( 'NONE',  ( 20.42812500061451431, -4.541064518000419881, 2.621784821874995952 ) ) ;
#47054 = CARTESIAN_POINT ( 'NONE',  ( 18.86249999999999716, -5.773502691896255534, -1.060575238724906372E-15 ) ) ;
#47055 = CARTESIAN_POINT ( 'NONE',  ( 65.00000000000000000, 9.426999614876460059E-14, 9.000000000000000000 ) ) ;
#47056 = CARTESIAN_POINT ( 'NONE',  ( 10.68750000000000000, -2.886751345948129988, 4.999999999999997335 ) ) ;
#47057 = CARTESIAN_POINT ( 'NONE',  ( 19.53750000122903430, 6.123233995736764310E-16, -4.999999999999998224 ) ) ;
#47058 = CARTESIAN_POINT ( 'NONE',  ( -3.999999999999999112, 10.10000000000000142, 30.00000000000000000 ) ) ;
#47059 = CARTESIAN_POINT ( 'NONE',  ( 9.496875000614517504, 0.000000000000000000, 4.756430356249998326 ) ) ;
#47060 = ORIENTED_EDGE ( 'NONE', *, *, #42578, .F. ) ;
#47061 = CARTESIAN_POINT ( 'NONE',  ( 18.67500000000000071, 4.330127018922191873, 2.499999999999999556 ) ) ;
#47062 = CARTESIAN_POINT ( 'NONE',  ( 22.27499999999999858, 4.330127018922191873, 2.499999999999999556 ) ) ;
#47063 = CARTESIAN_POINT ( 'NONE',  ( 18.30937500061451928, -4.541064518000417216, -2.621784821875001281 ) ) ;
#47064 = CARTESIAN_POINT ( 'NONE',  ( 13.30312500061451786, -4.541064518000417216, -2.621784821875001281 ) ) ;
#47065 = ORIENTED_EDGE ( 'NONE', *, *, #28761, .F. ) ;
#47066 = CARTESIAN_POINT ( 'NONE',  ( 10.20000000000000107, 0.000000000000000000, 4.999999999999998224 ) ) ;
#47067 = CARTESIAN_POINT ( 'NONE',  ( 4.753125000614515372, -4.541064518000417216, -2.621784821875001281 ) ) ;
#47068 = CARTESIAN_POINT ( 'NONE',  ( 3.242103111326755549, 4.229119190475764789, 3.162089978331414031 ) ) ;
#47069 = CARTESIAN_POINT ( 'NONE',  ( 13.35000000000000142, 0.000000000000000000, 4.999999999999998224 ) ) ;
#47070 = CARTESIAN_POINT ( 'NONE',  ( 28.13437500061451502, -2.746126346562642428, -4.756430356249999214 ) ) ;
#47071 = CARTESIAN_POINT ( 'NONE',  ( 9.001249775931846008E-16, 15.86562500061451608, 34.90005215228797653 ) ) ;
#47072 = CARTESIAN_POINT ( 'NONE',  ( 28.11562500061451431, -6.054752690667223547, -1.112240025338166033E-15 ) ) ;
#47073 = CARTESIAN_POINT ( 'NONE',  ( 8.699999999999999289, 4.330127018922192761, -2.499999999999997780 ) ) ;
#47074 = CARTESIAN_POINT ( 'NONE',  ( -3.756430356250000102, 16.46562499938548285, 30.00000000000000000 ) ) ;
#47075 = CARTESIAN_POINT ( 'NONE',  ( 24.12187500061451217, -6.054752690667223547, -1.112240025338166033E-15 ) ) ;
#47076 = VERTEX_POINT ( 'NONE', #28660 ) ;
#47077 = CARTESIAN_POINT ( 'NONE',  ( 22.37812500061451360, 6.421520780324663323E-16, -5.243569643749999010 ) ) ;
#47078 = CARTESIAN_POINT ( 'NONE',  ( 22.95937500061451431, 4.541064518000418104, -2.621784821874998173 ) ) ;
#47079 = CARTESIAN_POINT ( 'NONE',  ( -4.243569643749999898, 15.75312500061459531, -30.00000000000000000 ) ) ;
#47080 = CARTESIAN_POINT ( 'NONE',  ( 7.415625000614516793, -6.054752690667223547, -1.112240025338166033E-15 ) ) ;
#47081 = CARTESIAN_POINT ( 'NONE',  ( 3.825000000000001954, 4.330127018922191873, 2.499999999999999556 ) ) ;
#47082 = CARTESIAN_POINT ( 'NONE',  ( 24.81562500061451715, 3.027376345333611329, 5.243569643749999010 ) ) ;
#47083 = CARTESIAN_POINT ( 'NONE',  ( 27.34687500061451360, 4.119189519843966529, -2.378215178124998275 ) ) ;
#47084 = CARTESIAN_POINT ( 'NONE',  ( 10.39687500061451786, 5.492252693125287522, 3.363034840372157021E-16 ) ) ;
#47085 =( BOUNDED_CURVE ( )  B_SPLINE_CURVE ( 2, ( #57351, #11934, #51462, #34459, #51102, #18174, #40743 ),
 .UNSPECIFIED., .F., .F. ) 
 B_SPLINE_CURVE_WITH_KNOTS ( ( 3, 2, 2, 3 ),
 ( 0.1000000000000000611, 0.1027777777777778151, 0.1055555555555555969, 0.1083333333333333648 ),
 .UNSPECIFIED. ) 
 CURVE ( )  GEOMETRIC_REPRESENTATION_ITEM ( )  RATIONAL_B_SPLINE_CURVE ( ( 0.9999999999999973355, 0.8660254037844413721, 1.000000000000000000, 0.8660254037844387076, 1.000000000000000000, 0.8660254037844373753, 1.000000000000001332 ) ) 
 REPRESENTATION_ITEM ( '' )  );
#47086 = CARTESIAN_POINT ( 'NONE',  ( 17.97187500061451715, 3.027376345333613106, -5.243569643749998122 ) ) ;
#47087 = CARTESIAN_POINT ( 'NONE',  ( 26.03437500061451715, 6.421520780324663323E-16, -5.243569643749999010 ) ) ;
#47088 = CARTESIAN_POINT ( 'NONE',  ( -2.121784821874996840, 17.68437500061451928, 33.67503911421598417 ) ) ;
#47089 = CARTESIAN_POINT ( 'NONE',  ( 6.440625000614517148, -3.027376345333614438, 5.243569643749998122 ) ) ;
#47090 = EDGE_CURVE ( 'NONE', #38159, #47076, #15670, .T. ) ;
#47091 = CARTESIAN_POINT ( 'NONE',  ( 4.246875000614519280, -3.027376345333614438, 5.243569643749998122 ) ) ;
#47092 = CARTESIAN_POINT ( 'NONE',  ( 4.184734259358962483, 3.742548387690015854, -3.517716042735904658 ) ) ;
#47093 = CARTESIAN_POINT ( 'NONE',  ( 5.353125000614515905, 4.541064518000418104, -2.621784821874998173 ) ) ;
#47094 = CARTESIAN_POINT ( 'NONE',  ( 9.571875000614518569, 3.027376345333611329, 5.243569643749999010 ) ) ;
#47095 =( NAMED_UNIT ( * ) PLANE_ANGLE_UNIT ( ) SI_UNIT ( $, .RADIAN. ) );
#47096 = CARTESIAN_POINT ( 'NONE',  ( 16.20000000122903216, -2.886751345948129988, 4.999999999999997335 ) ) ;
#47097 = CARTESIAN_POINT ( 'NONE',  ( 3.421875000614516882, -6.054752690667223547, -1.112240025338166033E-15 ) ) ;
#47098 = CARTESIAN_POINT ( 'NONE',  ( 7.940625000614518036, -3.027376345333610441, -5.243569643749999898 ) ) ;
#47099 = CARTESIAN_POINT ( 'NONE',  ( -1.999999999999999112, 14.84374999877096712, 26.53589838486224650 ) ) ;
#47100 = CARTESIAN_POINT ( 'NONE',  ( 20.90625000122903288, 4.330127018922192761, -2.499999999999997780 ) ) ;
#47101 = CARTESIAN_POINT ( 'NONE',  ( 16.99687500061451573, -3.027376345333610441, -5.243569643749999898 ) ) ;
#47102 = CARTESIAN_POINT ( 'NONE',  ( 1.999999999999998668, 17.71250000122903501, 26.53589838486224650 ) ) ;
#47103 = ORIENTED_EDGE ( 'NONE', *, *, #798, .T. ) ;
#47104 = CARTESIAN_POINT ( 'NONE',  ( 25.26562500061451289, 3.027376345333611329, 5.243569643749999010 ) ) ;
#47105 = CARTESIAN_POINT ( 'NONE',  ( 9.965625000614517504, 3.027376345333611329, 5.243569643749999010 ) ) ;
#47106 = CARTESIAN_POINT ( 'NONE',  ( 28.02187500061451431, 3.027376345333611329, 5.243569643749999010 ) ) ;
#47107 = CARTESIAN_POINT ( 'NONE',  ( 11.09062500061451573, -3.027376345333610441, -5.243569643749999898 ) ) ;
#47108 = CARTESIAN_POINT ( 'NONE',  ( 3.450000001229035718, 5.773502691896255534, 3.535250795749688401E-16 ) ) ;
#47109 = CARTESIAN_POINT ( 'NONE',  ( 9.750000001229032875, 5.773502691896255534, 3.535250795749688894E-16 ) ) ;
#47110 = CARTESIAN_POINT ( 'NONE',  ( 23.99062500061451786, -3.027376345333614438, 5.243569643749998122 ) ) ;
#47111 = CARTESIAN_POINT ( 'NONE',  ( -2.121784821874996840, 13.12812500061451715, -26.32496088578401583 ) ) ;
#47112 = CARTESIAN_POINT ( 'NONE',  ( 13.23750000122903359, 6.123233995736764310E-16, -4.999999999999998224 ) ) ;
#47113 = CARTESIAN_POINT ( 'NONE',  ( 21.74062500061451431, -3.027376345333614438, 5.243569643749998122 ) ) ;
#47114 = CARTESIAN_POINT ( 'NONE',  ( 17.95312500061451644, 4.541064518000418104, -2.621784821874998173 ) ) ;
#47115 = CARTESIAN_POINT ( 'NONE',  ( 29.70937500061451431, 4.119189519843966529, -2.378215178124998275 ) ) ;
#47116 = CARTESIAN_POINT ( 'NONE',  ( 18.75000000000000000, 0.000000000000000000, 4.999999999999998224 ) ) ;
#47117 = CARTESIAN_POINT ( 'NONE',  ( 14.10000000122903252, -2.886751345948125991, -5.000000000000000000 ) ) ;
#47118 = CARTESIAN_POINT ( 'NONE',  ( 10.60312500061451679, -4.541064518000417216, -2.621784821875001281 ) ) ;
#47119 = CARTESIAN_POINT ( 'NONE',  ( 14.39062500061451821, 6.054752690667223547, 3.707466751127219781E-16 ) ) ;
#47120 = CARTESIAN_POINT ( 'NONE',  ( 25.38750000122903216, 6.123233995736764310E-16, -4.999999999999998224 ) ) ;
#47121 = CARTESIAN_POINT ( 'NONE',  ( 21.94687500061451857, -3.027376345333610441, -5.243569643749999898 ) ) ;
#47122 = CARTESIAN_POINT ( 'NONE',  ( 20.97187500061451715, -6.054752690667223547, -1.112240025338166033E-15 ) ) ;
#47123 = CYLINDRICAL_SURFACE ( 'NONE', #46574, 4.999999999999998224 ) ;
#47124 = CARTESIAN_POINT ( 'NONE',  ( 6.862500001229034474, -4.330127018922190985, -2.500000000000001332 ) ) ;
#47125 =( BOUNDED_CURVE ( )  B_SPLINE_CURVE ( 2, ( #12700, #57758, #7166, #18594, #29695, #52233, #1637, #69232, #63667 ),
 .UNSPECIFIED., .F., .F. ) 
 B_SPLINE_CURVE_WITH_KNOTS ( ( 3, 2, 2, 2, 3 ),
 ( 0.5108695652173913526, 0.5144927536231883591, 0.5217391304347825942, 0.5289855072463768293, 0.5326086956521739468 ),
 .UNSPECIFIED. ) 
 CURVE ( )  GEOMETRIC_REPRESENTATION_ITEM ( )  RATIONAL_B_SPLINE_CURVE ( ( 0.9330127018922192983, 0.9330127018922202975, 1.000000000000000000, 0.8660254037844387076, 1.000000000000000000, 0.8660254037844387076, 1.000000000000000000, 0.9330127018922194093, 0.9330127018922194093 ) ) 
 REPRESENTATION_ITEM ( '' )  );
#47126 = CARTESIAN_POINT ( 'NONE',  ( 6.309375000614517504, 4.541064518000418104, -2.621784821874998173 ) ) ;
#47127 = CARTESIAN_POINT ( 'NONE',  ( 26.10937500061451644, 4.541064518000418104, -2.621784821874998173 ) ) ;
#47128 =( BOUNDED_CURVE ( )  B_SPLINE_CURVE ( 2, ( #58588, #54525, #14621, #30531, #31630, #20156, #42347, #59312, #43077 ),
 .UNSPECIFIED., .F., .F. ) 
 B_SPLINE_CURVE_WITH_KNOTS ( ( 3, 2, 2, 2, 3 ),
 ( 0.5543478260869565410, 0.5579710144927536586, 0.5652173913043477826, 0.5724637681159420177, 0.5760869565217391353 ),
 .UNSPECIFIED. ) 
 CURVE ( )  GEOMETRIC_REPRESENTATION_ITEM ( )  RATIONAL_B_SPLINE_CURVE ( ( 0.9330127018922194093, 0.9330127018922194093, 1.000000000000000000, 0.8660254037844387076, 1.000000000000000000, 0.8660254037844387076, 1.000000000000000000, 0.9330127018922194093, 0.9330127018922194093 ) ) 
 REPRESENTATION_ITEM ( '' )  );
#47129 = CARTESIAN_POINT ( 'NONE',  ( 15.33750000122903323, -4.330127018922194537, 2.499999999999995559 ) ) ;
#47130 = CARTESIAN_POINT ( 'NONE',  ( 21.32812500061451644, -4.541064518000419881, 2.621784821874995952 ) ) ;
#47131 = CARTESIAN_POINT ( 'NONE',  ( 25.84687500061451360, -3.027376345333614438, 5.243569643749998122 ) ) ;
#47132 = CARTESIAN_POINT ( 'NONE',  ( 1.878215178125000495, 16.42812499938548143, 26.74683588394047007 ) ) ;
#47133 = CARTESIAN_POINT ( 'NONE',  ( 7.724999999999999645, 6.123233995736764310E-16, -4.999999999999998224 ) ) ;
#47134 = DIRECTION ( 'NONE',  ( -0.000000000000000000, -1.000000000000000000, -0.000000000000000000 ) ) ;
#47135 = CARTESIAN_POINT ( 'NONE',  ( 8.484375000614518214, 6.421520780324663323E-16, -5.243569643749999010 ) ) ;
#47136 = CARTESIAN_POINT ( 'NONE',  ( 18.02812500061451573, 4.541064518000418104, 2.621784821874999949 ) ) ;
#47137 = ORIENTED_EDGE ( 'NONE', *, *, #1197, .T. ) ;
#47138 = CYLINDRICAL_SURFACE ( 'NONE', #41889, 4.999999999999998224 ) ;
#47139 = CARTESIAN_POINT ( 'NONE',  ( 26.65312500061451573, 0.000000000000000000, 5.243569643749999010 ) ) ;
#47140 = CARTESIAN_POINT ( 'NONE',  ( 4.321875000614517681, -6.054752690667223547, -1.112240025338166033E-15 ) ) ;
#47141 = DIRECTION ( 'NONE',  ( -1.000000000000000000, -0.000000000000000000, -0.000000000000000000 ) ) ;
#47142 = CARTESIAN_POINT ( 'NONE',  ( 3.988952146040426694, 3.968976988887717994, -3.612669488674732587 ) ) ;
#47143 = CARTESIAN_POINT ( 'NONE',  ( 17.92500000000000071, -4.330127018922194537, 2.499999999999995559 ) ) ;
#47144 = CARTESIAN_POINT ( 'NONE',  ( 20.50312500061451715, -4.541064518000417216, -2.621784821875001281 ) ) ;
#47145 = VERTEX_POINT ( 'NONE', #10948 ) ;
#47146 = CARTESIAN_POINT ( 'NONE',  ( 25.87500000000000000, 4.330127018922191873, 2.499999999999999556 ) ) ;
#47147 = CARTESIAN_POINT ( 'NONE',  ( 25.69687500061451502, 6.054752690667223547, 3.707466751127219781E-16 ) ) ;
#47148 =( BOUNDED_CURVE ( )  B_SPLINE_CURVE ( 2, ( #72513, #61062, #60316, #21164, #66240, #37796, #27826 ),
 .UNSPECIFIED., .F., .F. ) 
 B_SPLINE_CURVE_WITH_KNOTS ( ( 3, 2, 2, 3 ),
 ( 0.1333333333333333037, 0.1361111111111110716, 0.1388888888888888673, 0.1416666666666666352 ),
 .UNSPECIFIED. ) 
 CURVE ( )  GEOMETRIC_REPRESENTATION_ITEM ( )  RATIONAL_B_SPLINE_CURVE ( ( 1.000000000000001332, 0.8660254037844373753, 1.000000000000000000, 0.8660254037844387076, 1.000000000000000000, 0.8660254037844400399, 0.9999999999999986677 ) ) 
 REPRESENTATION_ITEM ( '' )  );
#47149 = EDGE_LOOP ( 'NONE', ( #47644, #35617, #5656, #4384 ) ) ;
#47150 = CARTESIAN_POINT ( 'NONE',  ( 12.89062500061451821, -3.027376345333610441, -5.243569643749999898 ) ) ;
#47151 = CARTESIAN_POINT ( 'NONE',  ( 4.828125000614518214, 6.421520780324663323E-16, -5.243569643749999010 ) ) ;
#47152 = CARTESIAN_POINT ( 'NONE',  ( 15.38437500061451679, -2.746126346562646425, 4.756430356249996549 ) ) ;
#47153 = CARTESIAN_POINT ( 'NONE',  ( 29.80312500061451431, 0.000000000000000000, 5.243569643749999010 ) ) ;
#47154 = CARTESIAN_POINT ( 'NONE',  ( 14.62500000122903288, 2.886751345948129099, -4.999999999999998224 ) ) ;
#47155 = CARTESIAN_POINT ( 'NONE',  ( 19.27500000000000213, -4.330127018922194537, 2.499999999999995559 ) ) ;
#47156 = CARTESIAN_POINT ( 'NONE',  ( 28.80000000000000071, -4.330127018922190985, -2.500000000000001332 ) ) ;
#47157 = CARTESIAN_POINT ( 'NONE',  ( 4.284375000614518925, -4.541064518000419881, 2.621784821874995952 ) ) ;
#47158 = CARTESIAN_POINT ( 'NONE',  ( 8.746875000614515727, -3.027376345333614438, 5.243569643749998122 ) ) ;
#47159 = CARTESIAN_POINT ( 'NONE',  ( 19.84687500061451360, 6.054752690667223547, 3.707466751127219781E-16 ) ) ;
#47160 = CARTESIAN_POINT ( 'NONE',  ( -3.999999999999999112, 17.30000000000000071, -30.00000000000000000 ) ) ;
#47161 = ORIENTED_EDGE ( 'NONE', *, *, #65919, .T. ) ;
#47162 = CARTESIAN_POINT ( 'NONE',  ( 28.34062500061451928, 6.054752690667223547, 3.707466751127219781E-16 ) ) ;
#47163 = CARTESIAN_POINT ( 'NONE',  ( 29.14687500061451075, -3.027376345333610441, -5.243569643749999898 ) ) ;
#47164 = CARTESIAN_POINT ( 'NONE',  ( 4.771875000614516971, -6.054752690667223547, -1.112240025338166033E-15 ) ) ;
#47165 = CARTESIAN_POINT ( 'NONE',  ( 16.76249999999999929, 2.886751345948129099, -4.999999999999998224 ) ) ;
#47166 = CARTESIAN_POINT ( 'NONE',  ( 12.81562500061451537, -6.054752690667223547, -1.112240025338166033E-15 ) ) ;
#47167 = CARTESIAN_POINT ( 'NONE',  ( -4.000000000000000888, 19.06249999999999645, 32.30940107675850470 ) ) ;
#47168 = CARTESIAN_POINT ( 'NONE',  ( 3.975000000000002753, -4.330127018922194537, 2.499999999999995559 ) ) ;
#47169 = CARTESIAN_POINT ( 'NONE',  ( 19.23750000122903714, 4.330127018922191873, 2.499999999999999556 ) ) ;
#47170 = CARTESIAN_POINT ( 'NONE',  ( 27.75000000000000000, 0.000000000000000000, 4.999999999999998224 ) ) ;
#47171 = CARTESIAN_POINT ( 'NONE',  ( 17.52187500061451431, 2.746126346562645981, -4.756430356249997438 ) ) ;
#47172 = CARTESIAN_POINT ( 'NONE',  ( 6.965625000614518392, -6.054752690667223547, -1.112240025338166033E-15 ) ) ;
#47173 = CARTESIAN_POINT ( 'NONE',  ( 24.00937500061451502, 0.000000000000000000, 5.243569643749999010 ) ) ;
#47174 = CARTESIAN_POINT ( 'NONE',  ( 26.70937500061451431, 0.000000000000000000, 5.243569643749999010 ) ) ;
#47175 = CARTESIAN_POINT ( 'NONE',  ( 7.350000000000002309, 4.330127018922192761, -2.499999999999997780 ) ) ;
#47176 = CARTESIAN_POINT ( 'NONE',  ( -3.999999999999999112, 12.91250000122903430, 30.00000000000000000 ) ) ;
#47177 = CARTESIAN_POINT ( 'NONE',  ( 15.55312500061451608, -4.541064518000417216, -2.621784821875001281 ) ) ;
#47178 = CARTESIAN_POINT ( 'NONE',  ( 7.875000001229034652, 2.886751345948129099, -4.999999999999998224 ) ) ;
#47179 = EDGE_CURVE ( 'NONE', #8722, #69635, #66158, .T. ) ;
#47180 = CARTESIAN_POINT ( 'NONE',  ( 11.44687500061451857, -3.027376345333614438, 5.243569643749998122 ) ) ;
#47181 = DIRECTION ( 'NONE',  ( -1.000000000000000000, -0.000000000000000000, -0.000000000000000000 ) ) ;
#47182 = ORIENTED_EDGE ( 'NONE', *, *, #48691, .F. ) ;
#47183 = CARTESIAN_POINT ( 'NONE',  ( 11.24062500061451608, 6.054752690667223547, 3.707466751127219781E-16 ) ) ;
#47184 = CARTESIAN_POINT ( 'NONE',  ( 1.999999999999997335, 19.56874999877096499, 33.46410161513775705 ) ) ;
#47185 = CARTESIAN_POINT ( 'NONE',  ( 24.45000000122903572, -2.886751345948125991, -5.000000000000000000 ) ) ;
#47186 = CARTESIAN_POINT ( 'NONE',  ( 11.85937500061451644, 0.000000000000000000, 5.243569643749999010 ) ) ;
#47187 = CARTESIAN_POINT ( 'NONE',  ( 15.29062500061451679, 6.054752690667223547, 3.707466751127219781E-16 ) ) ;
#47188 = FACE_OUTER_BOUND ( 'NONE', #3969, .T. ) ;
#47189 = CARTESIAN_POINT ( 'NONE',  ( 23.85937500061451644, 4.541064518000418104, -2.621784821874998173 ) ) ;
#47190 = CARTESIAN_POINT ( 'NONE',  ( 4.898587196589411843E-16, 20.00000000000000000, 33.99999999999999289 ) ) ;
#47191 = CARTESIAN_POINT ( 'NONE',  ( 5.287500000000000533, -2.886751345948130876, 4.999999999999996447 ) ) ;
#47192 = DIRECTION ( 'NONE',  ( -0.000000000000000000, -1.000000000000000000, -0.000000000000000000 ) ) ;
#47193 = CARTESIAN_POINT ( 'NONE',  ( -4.243569643749999898, 13.97187500061451715, -32.45002607614398471 ) ) ;
#47194 = CARTESIAN_POINT ( 'NONE',  ( 16.24687500061451573, 6.054752690667223547, 3.707466751127219781E-16 ) ) ;
#47195 = CARTESIAN_POINT ( 'NONE',  ( 17.06250000122903288, 0.000000000000000000, 4.999999999999998224 ) ) ;
#47196 = CARTESIAN_POINT ( 'NONE',  ( 11.97187500061451892, -6.054752690667223547, -1.112240025338166033E-15 ) ) ;
#47197 = CARTESIAN_POINT ( 'NONE',  ( -3.000416591977282496E-16, 19.69062500061451360, -34.90005215228797653 ) ) ;
#47198 = CARTESIAN_POINT ( 'NONE',  ( 19.68750000122903288, 4.330127018922191873, 2.499999999999999556 ) ) ;
#47199 = CARTESIAN_POINT ( 'NONE',  ( 11.91562500061451857, -6.054752690667223547, -1.112240025338166033E-15 ) ) ;
#47200 = ORIENTED_EDGE ( 'NONE', *, *, #14213, .T. ) ;
#47201 = ORIENTED_EDGE ( 'NONE', *, *, #11270, .T. ) ;
#47202 = CARTESIAN_POINT ( 'NONE',  ( 18.63749999999999929, 5.773502691896255534, 3.535250795749688894E-16 ) ) ;
#47203 = CARTESIAN_POINT ( 'NONE',  ( 3.999999999999998668, 15.55624999877096748, 32.30940107675850470 ) ) ;
#47204 = CARTESIAN_POINT ( 'NONE',  ( 13.65937500061451715, 0.000000000000000000, 5.243569643749999010 ) ) ;
#47205 = DIRECTION ( 'NONE',  ( 0.000000000000000000, 0.000000000000000000, 1.000000000000000000 ) ) ;
#47206 = CARTESIAN_POINT ( 'NONE',  ( 11.62500000122903465, 2.886751345948126879, 4.999999999999999112 ) ) ;
#47207 = CARTESIAN_POINT ( 'NONE',  ( 21.07500000122903572, 2.886751345948126879, 4.999999999999999112 ) ) ;
#47208 = CARTESIAN_POINT ( 'NONE',  ( 17.50312500061451715, 4.541064518000418104, -2.621784821874998173 ) ) ;
#47209 = CARTESIAN_POINT ( 'NONE',  ( 20.87812500061451715, -4.541064518000419881, 2.621784821874995952 ) ) ;
#47210 = CARTESIAN_POINT ( 'NONE',  ( 2.953125000614516438, -4.541064518000417216, -2.621784821875001281 ) ) ;
#47211 = CARTESIAN_POINT ( 'NONE',  ( 27.11249999999999716, 2.886751345948129099, -4.999999999999998224 ) ) ;
#47212 = DIRECTION ( 'NONE',  ( -1.000000000000000000, -0.000000000000000000, -0.000000000000000000 ) ) ;
#47213 = CARTESIAN_POINT ( 'NONE',  ( 28.35000000000000142, -4.330127018922190985, -2.500000000000001332 ) ) ;
#47214 = CARTESIAN_POINT ( 'NONE',  ( 28.47187500061451715, 3.027376345333611329, 5.243569643749999010 ) ) ;
#47215 = CARTESIAN_POINT ( 'NONE',  ( 30.00000000000000000, 0.000000000000000000, 4.999999999999998224 ) ) ;
#47216 = CARTESIAN_POINT ( 'NONE',  ( -2.121784821874999949, 14.83437500061451786, -33.67503911421598417 ) ) ;
#47217 = CARTESIAN_POINT ( 'NONE',  ( 4.650000001229035895, -2.886751345948125991, -5.000000000000000000 ) ) ;
#47218 = CARTESIAN_POINT ( 'NONE',  ( 5.362500000000003375, -5.773502691896255534, -1.060575238724906372E-15 ) ) ;
#47219 = EDGE_CURVE ( 'NONE', #15128, #41505, #53865, .T. ) ;
#47220 = CARTESIAN_POINT ( 'NONE',  ( 28.74375000122903501, -2.886751345948095349, 5.000000000000058620 ) ) ;
#47221 = CARTESIAN_POINT ( 'NONE',  ( 9.871875000614517504, 3.027376345333613106, -5.243569643749998122 ) ) ;
#47222 = CARTESIAN_POINT ( 'NONE',  ( 28.45312500061451289, 0.000000000000000000, 5.243569643749999010 ) ) ;
#47223 = CARTESIAN_POINT ( 'NONE',  ( 15.61875000122903323, 2.886751345948126879, 4.999999999999998224 ) ) ;
#47224 = CARTESIAN_POINT ( 'NONE',  ( 3.658875532774302997, -3.408200617373282171, -3.658875532774302997 ) ) ;
#47225 = CARTESIAN_POINT ( 'NONE',  ( 8.324999999999999289, 4.330127018922191873, 2.499999999999999556 ) ) ;
#47226 = CARTESIAN_POINT ( 'NONE',  ( 8.409375000614518925, -4.541064518000417216, -2.621784821875001281 ) ) ;
#47227 = CARTESIAN_POINT ( 'NONE',  ( 11.18437500061451928, 6.421520780324663323E-16, -5.243569643749999010 ) ) ;
#47228 = CARTESIAN_POINT ( 'NONE',  ( 4.687500000000000000, 5.773502691896255534, 3.535250795749688894E-16 ) ) ;
#47229 = CARTESIAN_POINT ( 'NONE',  ( -4.243569643749999898, 15.26562500061459460, 27.54997392385601529 ) ) ;
#47230 = CARTESIAN_POINT ( 'NONE',  ( 6.112499999999999822, 2.886751345948126879, 4.999999999999999112 ) ) ;
#47231 = CARTESIAN_POINT ( 'NONE',  ( 15.45937500061451608, -5.492252693125287522, -1.008910452111647106E-15 ) ) ;
#47232 = CARTESIAN_POINT ( 'NONE',  ( 20.39062500061451644, -3.027376345333614438, 5.243569643749998122 ) ) ;
#47233 = CARTESIAN_POINT ( 'NONE',  ( 12.17812500061451608, 4.541064518000418104, 2.621784821874999949 ) ) ;
#47234 = CARTESIAN_POINT ( 'NONE',  ( 22.92187500061451644, 4.119189519843966529, 2.378215178124999607 ) ) ;
#47235 = CARTESIAN_POINT ( 'NONE',  ( 9.796875000614519990, -3.027376345333610441, -5.243569643749999898 ) ) ;
#47236 = CARTESIAN_POINT ( 'NONE',  ( 26.13749999999999929, -2.886751345948125991, -5.000000000000000000 ) ) ;
#47237 = CARTESIAN_POINT ( 'NONE',  ( 23.55000000122903359, -2.886751345948125991, -5.000000000000000000 ) ) ;
#47238 = CARTESIAN_POINT ( 'NONE',  ( 17.06250000000000000, -5.773502691896255534, -1.060575238724906372E-15 ) ) ;
#47239 = CARTESIAN_POINT ( 'NONE',  ( 11.25937500061451679, 4.541064518000418104, -2.621784821874998173 ) ) ;
#47240 = CARTESIAN_POINT ( 'NONE',  ( 27.34687500061451360, -3.027376345333610441, -5.243569643749999898 ) ) ;
#47241 = EDGE_CURVE ( 'NONE', #39465, #40447, #44325, .T. ) ;
#47242 = CARTESIAN_POINT ( 'NONE',  ( 3.571875000614517237, 3.027376345333613106, -5.243569643749998122 ) ) ;
#47243 = CARTESIAN_POINT ( 'NONE',  ( 24.33750000122903145, -4.330127018922194537, 2.499999999999995559 ) ) ;
#47244 = CARTESIAN_POINT ( 'NONE',  ( 20.33437500061451786, 4.541064518000418104, 2.621784821874999949 ) ) ;
#47245 = CARTESIAN_POINT ( 'NONE',  ( 11.70937500061451608, 4.541064518000418104, -2.621784821874998173 ) ) ;
#47246 = CARTESIAN_POINT ( 'NONE',  ( -3.756430356250000102, 19.27812499938548640, 30.00000000000000000 ) ) ;
#47247 = CARTESIAN_POINT ( 'NONE',  ( 23.77499999999999858, -4.330127018922194537, 2.499999999999995559 ) ) ;
#47248 = CARTESIAN_POINT ( 'NONE',  ( -3.999999999999999556, 12.68750000000000000, 27.69059892324149175 ) ) ;
#47249 = CARTESIAN_POINT ( 'NONE',  ( 9.001249775931846008E-16, 11.42187500061451999, -25.09994784771203058 ) ) ;
#47250 = CARTESIAN_POINT ( 'NONE',  ( 28.13437500061451502, -4.119189519843968306, 2.378215178124996054 ) ) ;
#47251 = CARTESIAN_POINT ( 'NONE',  ( 14.09062500061451750, -3.027376345333614438, 5.243569643749998122 ) ) ;
#47252 = CARTESIAN_POINT ( 'NONE',  ( 4.762499999999999289, 2.886751345948126879, 4.999999999999999112 ) ) ;
#47253 = CARTESIAN_POINT ( 'NONE',  ( 45.00000000000000000, 0.000000000000000000, 0.000000000000000000 ) ) ;
#47254 = CARTESIAN_POINT ( 'NONE',  ( -3.137519842735245283E-14, 12.91250000000000142, 34.00000000000000000 ) ) ;
#47255 = CARTESIAN_POINT ( 'NONE',  ( 14.36249999999999893, -5.773502691896255534, -1.060575238724906372E-15 ) ) ;
#47256 = CARTESIAN_POINT ( 'NONE',  ( 4.243569643749999898, 10.99062500061451786, 32.45002607614398471 ) ) ;
#47257 = CARTESIAN_POINT ( 'NONE',  ( 13.50000000122903288, -2.886751345948129988, 4.999999999999997335 ) ) ;
#47258 = CARTESIAN_POINT ( 'NONE',  ( 23.63437500061451502, -4.541064518000419881, 2.621784821874995952 ) ) ;
#47259 = CARTESIAN_POINT ( 'NONE',  ( 4.022770794281430362, 2.969407772832715953, -4.321770970117402300 ) ) ;
#47260 = ORIENTED_EDGE ( 'NONE', *, *, #30226, .F. ) ;
#47261 = CARTESIAN_POINT ( 'NONE',  ( 20.35312500061451502, 0.000000000000000000, 5.243569643749999010 ) ) ;
#47262 = CARTESIAN_POINT ( 'NONE',  ( 4.340625000614515727, -3.027376345333610441, -5.243569643749999898 ) ) ;
#47263 = CARTESIAN_POINT ( 'NONE',  ( 20.40937500061451715, 0.000000000000000000, 5.243569643749999010 ) ) ;
#47264 = CARTESIAN_POINT ( 'NONE',  ( 3.300000000000000711, 4.330127018922192761, -2.499999999999997780 ) ) ;
#47265 = CARTESIAN_POINT ( 'NONE',  ( 6.028125000614517504, -4.541064518000419881, 2.621784821874995952 ) ) ;
#47266 = CARTESIAN_POINT ( 'NONE',  ( 22.22812500061451502, -4.541064518000419881, 2.621784821874995952 ) ) ;
#47267 = CARTESIAN_POINT ( 'NONE',  ( 2.121784821875001281, 14.10312500061451679, 33.67503911421598417 ) ) ;
#47268 = CARTESIAN_POINT ( 'NONE',  ( 18.00000000122903288, -2.886751345948129988, 4.999999999999997335 ) ) ;
#47269 = CARTESIAN_POINT ( 'NONE',  ( 13.05937500061451750, 4.119189519843966529, -2.378215178124998275 ) ) ;
#47270 = CARTESIAN_POINT ( 'NONE',  ( 9.703125000614514661, -4.541064518000417216, -2.621784821875001281 ) ) ;
#47271 = CARTESIAN_POINT ( 'NONE',  ( 4.134375000614517681, 4.541064518000418104, 2.621784821874999949 ) ) ;
#47272 = CARTESIAN_POINT ( 'NONE',  ( 3.384375000614517237, -4.541064518000419881, 2.621784821874995952 ) ) ;
#47273 = CARTESIAN_POINT ( 'NONE',  ( 23.03437500061451715, 4.541064518000418104, 2.621784821874999949 ) ) ;
#47274 = CARTESIAN_POINT ( 'NONE',  ( 15.21562500061451750, 3.027376345333613106, -5.243569643749998122 ) ) ;
#47275 = EDGE_CURVE ( 'NONE', #53798, #39431, #56017, .T. ) ;
#47276 = CARTESIAN_POINT ( 'NONE',  ( 25.16250000122903074, 0.000000000000000000, 4.999999999999998224 ) ) ;
#47277 = CARTESIAN_POINT ( 'NONE',  ( 24.70312500061451644, 4.541064518000418104, -2.621784821874998173 ) ) ;
#47278 = CARTESIAN_POINT ( 'NONE',  ( 18.27187500061451431, -6.054752690667223547, -1.112240025338166033E-15 ) ) ;
#47279 = CARTESIAN_POINT ( 'NONE',  ( 14.12812500061451715, -4.541064518000419881, 2.621784821874995952 ) ) ;
#47280 = CARTESIAN_POINT ( 'NONE',  ( -3.000416591977282496E-16, 16.14687500061451431, 25.09994784771203058 ) ) ;
#47281 = CARTESIAN_POINT ( 'NONE',  ( 20.54062500061451502, -3.027376345333610441, -5.243569643749999898 ) ) ;
#47282 = CARTESIAN_POINT ( 'NONE',  ( 45.00000000000000000, -6.363961030678871644, 4.863961030678981778 ) ) ;
#47283 = ORIENTED_EDGE ( 'NONE', *, *, #42578, .T. ) ;
#47284 = CARTESIAN_POINT ( 'NONE',  ( 24.26249999999999929, -5.773502691896255534, -1.060575238724906372E-15 ) ) ;
#47285 = CARTESIAN_POINT ( 'NONE',  ( 2.000000000000001332, 10.70000000000000107, -26.53589838486224650 ) ) ;
#47286 = CARTESIAN_POINT ( 'NONE',  ( 2.655984681222220721E-16, 19.16562499938548214, 25.66244784525396483 ) ) ;
#47287 = CARTESIAN_POINT ( 'NONE',  ( 27.85312500061451502, 4.541064518000418104, -2.621784821874998173 ) ) ;
#47288 = CARTESIAN_POINT ( 'NONE',  ( 7.828125000614517326, -4.541064518000419881, 2.621784821874995952 ) ) ;
#47289 = CARTESIAN_POINT ( 'NONE',  ( 20.55000000122903359, 5.773502691896255534, 3.535250795749688894E-16 ) ) ;
#47290 = CARTESIAN_POINT ( 'NONE',  ( 23.76562500061451644, 3.027376345333613106, -5.243569643749998122 ) ) ;
#47291 = CARTESIAN_POINT ( 'NONE',  ( 26.39999999999999858, 0.000000000000000000, 4.999999999999998224 ) ) ;
#47292 = CARTESIAN_POINT ( 'NONE',  ( 4.000000000000000000, 15.80000000122903359, -27.69059892324149530 ) ) ;
#47293 = CARTESIAN_POINT ( 'NONE',  ( -5.810221930991193690E-16, 15.50000000122903465, -34.00000000000000000 ) ) ;
#47294 = CARTESIAN_POINT ( 'NONE',  ( 11.24062500061451608, 6.054752690667223547, 3.707466751127219781E-16 ) ) ;
#47295 = VERTEX_POINT ( 'NONE', #67117 ) ;
#47296 = CARTESIAN_POINT ( 'NONE',  ( 25.49062500061451786, -3.027376345333610441, -5.243569643749999898 ) ) ;
#47297 = CARTESIAN_POINT ( 'NONE',  ( 6.328125000614515550, 4.541064518000418104, 2.621784821874999949 ) ) ;
#47298 = CARTESIAN_POINT ( 'NONE',  ( 13.84687500061451537, -2.746126346562642428, -4.756430356249999214 ) ) ;
#47299 = CARTESIAN_POINT ( 'NONE',  ( 4.646859583631838042, -1.845723709011792613, 4.907986002307686668 ) ) ;
#47300 = CARTESIAN_POINT ( 'NONE',  ( 13.61250000000000071, 2.886751345948129099, -4.999999999999998224 ) ) ;
#47301 = VECTOR ( 'NONE', #67523, 1000.000000000000000 ) ;
#47302 = CARTESIAN_POINT ( 'NONE',  ( 14.48437500061451821, 4.541064518000418104, 2.621784821874999949 ) ) ;
#47303 = CARTESIAN_POINT ( 'NONE',  ( 8.325000001229033941, 2.886751345948129099, -4.999999999999998224 ) ) ;
#47304 = CARTESIAN_POINT ( 'NONE',  ( 16.69687500061451502, 6.054752690667223547, 3.707466751127219781E-16 ) ) ;
#47305 = CARTESIAN_POINT ( 'NONE',  ( 16.64999999999999858, -4.330127018922190985, -2.500000000000001332 ) ) ;
#47306 = CARTESIAN_POINT ( 'NONE',  ( 8.184375000614515727, 4.541064518000418104, 2.621784821874999949 ) ) ;
#47307 = CARTESIAN_POINT ( 'NONE',  ( -2.121784821874996840, 12.67812500061451786, -26.32496088578401583 ) ) ;
#47308 = CARTESIAN_POINT ( 'NONE',  ( 20.88750000122903572, 6.123233995736764310E-16, -4.999999999999998224 ) ) ;
#47309 = CARTESIAN_POINT ( 'NONE',  ( 22.32187500061451502, 5.824947211148865298E-16, -4.756430356249998326 ) ) ;
#47310 = VERTEX_POINT ( 'NONE', #29388 ) ;
#47311 = CARTESIAN_POINT ( 'NONE',  ( 23.31562500061451715, 3.027376345333613106, -5.243569643749998122 ) ) ;
#47312 = CARTESIAN_POINT ( 'NONE',  ( -1.071796769724488563, 17.50490381179670152, 34.00000000000000000 ) ) ;
#47313 = CARTESIAN_POINT ( 'NONE',  ( 26.07187500061451857, 3.027376345333613106, -5.243569643749998122 ) ) ;
#47314 = EDGE_CURVE ( 'NONE', #61022, #68363, #53421, .T. ) ;
#47315 = CARTESIAN_POINT ( 'NONE',  ( 29.03437500061451715, -4.541064518000419881, 2.621784821874995952 ) ) ;
#47316 = CARTESIAN_POINT ( 'NONE',  ( 20.92500000000000071, 4.330127018922191873, 2.499999999999999556 ) ) ;
#47317 = CARTESIAN_POINT ( 'NONE',  ( 6.103125000614515905, -4.541064518000417216, -2.621784821875001281 ) ) ;
#47318 = CARTESIAN_POINT ( 'NONE',  ( 22.28437500061451360, -2.746126346562642428, -4.756430356249999214 ) ) ;
#47319 = CARTESIAN_POINT ( 'NONE',  ( 17.55937500061451573, 4.541064518000418104, -2.621784821874998173 ) ) ;
#47320 = CARTESIAN_POINT ( 'NONE',  ( 7.809375000614515727, -5.492252693125287522, -1.008910452111647106E-15 ) ) ;
#47321 = CARTESIAN_POINT ( 'NONE',  ( 3.703125000614516882, 0.000000000000000000, 5.243569643749999010 ) ) ;
#47322 = CARTESIAN_POINT ( 'NONE',  ( 9.121875000614517504, 3.027376345333611329, 5.243569643749999010 ) ) ;
#47323 = CARTESIAN_POINT ( 'NONE',  ( 19.05937500061451928, 0.000000000000000000, 5.243569643749999010 ) ) ;
#47324 = CARTESIAN_POINT ( 'NONE',  ( -3.011742865011199921, 25.23389687710447760, 32.64526797158287508 ) ) ;
#47325 = CARTESIAN_POINT ( 'NONE',  ( 26.88749999999999574, -2.886751345948129988, 4.999999999999997335 ) ) ;
#47326 = CARTESIAN_POINT ( 'NONE',  ( 26.97187500061451360, 3.027376345333613106, -5.243569643749998122 ) ) ;
#47327 = CARTESIAN_POINT ( 'NONE',  ( 26.30625000122903145, 4.330127018922192761, -2.499999999999997780 ) ) ;
#47328 = CARTESIAN_POINT ( 'NONE',  ( 21.71249999999999858, 2.886751345948129099, -4.999999999999997335 ) ) ;
#47329 = ORIENTED_EDGE ( 'NONE', *, *, #40621, .F. ) ;
#47330 = CARTESIAN_POINT ( 'NONE',  ( 11.55000000000000071, 0.000000000000000000, 4.999999999999998224 ) ) ;
#47331 = CARTESIAN_POINT ( 'NONE',  ( 12.12187500061451573, 4.119189519843966529, 2.378215178124999607 ) ) ;
#47332 = CARTESIAN_POINT ( 'NONE',  ( 21.32812500061451644, -4.541064518000419881, 2.621784821874995952 ) ) ;
#47333 = CARTESIAN_POINT ( 'NONE',  ( 12.18750000000000000, -2.886751345948125991, -5.000000000000000000 ) ) ;
#47334 = CARTESIAN_POINT ( 'NONE',  ( 8.062500001229034652, 0.000000000000000000, 4.999999999999998224 ) ) ;
#47335 = CARTESIAN_POINT ( 'NONE',  ( 6.178125000614518747, 6.421520780324663323E-16, -5.243569643749999010 ) ) ;
#47336 = CARTESIAN_POINT ( 'NONE',  ( 21.93750000000000000, -2.886751345948129988, 4.999999999999997335 ) ) ;
#47337 = CARTESIAN_POINT ( 'NONE',  ( 20.05312500061451431, -4.541064518000417216, -2.621784821875001281 ) ) ;
#47338 = CARTESIAN_POINT ( 'NONE',  ( 14.69999999999999929, 0.000000000000000000, 4.999999999999998224 ) ) ;
#47339 = CARTESIAN_POINT ( 'NONE',  ( 24.97500000122903430, 2.886751345948129099, -4.999999999999998224 ) ) ;
#47340 = CARTESIAN_POINT ( 'NONE',  ( 3.756430356250000102, 18.49062499938548143, 30.00000000000000000 ) ) ;
#47341 = CARTESIAN_POINT ( 'NONE',  ( 6.112499999999999822, 2.886751345948126879, 4.999999999999999112 ) ) ;
#47342 = ORIENTED_EDGE ( 'NONE', *, *, #72661, .F. ) ;
#47343 = CARTESIAN_POINT ( 'NONE',  ( 18.51562500061451289, 3.027376345333611329, 5.243569643749999010 ) ) ;
#47344 = CARTESIAN_POINT ( 'NONE',  ( 27.06562500061451004, 3.027376345333611329, 5.243569643749999010 ) ) ;
#47345 = CARTESIAN_POINT ( 'NONE',  ( 26.29687500061451644, -3.027376345333614438, 5.243569643749998122 ) ) ;
#47346 = CARTESIAN_POINT ( 'NONE',  ( 15.06562500061451537, -6.054752690667223547, -1.112240025338166033E-15 ) ) ;
#47347 = CARTESIAN_POINT ( 'NONE',  ( 28.60312500061451502, -4.541064518000417216, -2.621784821875001281 ) ) ;
#47348 = CARTESIAN_POINT ( 'NONE',  ( 8.353125000614518569, -4.541064518000417216, -2.621784821875001281 ) ) ;
#47349 = CARTESIAN_POINT ( 'NONE',  ( 11.43750000000000000, 5.773502691896255534, 3.535250795749688401E-16 ) ) ;
#47350 = ADVANCED_FACE ( 'NONE', ( #68913 ), #2045, .F. ) ;
#47351 = CARTESIAN_POINT ( 'NONE',  ( 26.21250000122903501, -4.330127018922190985, -2.500000000000001332 ) ) ;
#47352 = CARTESIAN_POINT ( 'NONE',  ( 18.87187500061452283, 2.746126346562645981, -4.756430356249997438 ) ) ;
#47353 = CARTESIAN_POINT ( 'NONE',  ( 16.34062500061451573, -3.027376345333614438, 5.243569643749998122 ) ) ;
#47354 = CARTESIAN_POINT ( 'NONE',  ( 7.320879633048903241E-15, 18.53750000000000142, -34.00000000000000000 ) ) ;
#47355 = CIRCLE ( 'NONE', #36754, 10.00000000000000000 ) ;
#47356 = CARTESIAN_POINT ( 'NONE',  ( 29.03437500061451715, -4.541064518000419881, 2.621784821874995952 ) ) ;
#47357 = CARTESIAN_POINT ( 'NONE',  ( 9.496875000614517504, 6.054752690667223547, 3.707466751127219781E-16 ) ) ;
#47358 = CARTESIAN_POINT ( 'NONE',  ( 9.909375000614517148, 4.541064518000418104, -2.621784821874998173 ) ) ;
#47359 = CARTESIAN_POINT ( 'NONE',  ( 17.82187500061451502, -6.054752690667223547, -1.112240025338166033E-15 ) ) ;
#47360 = VERTEX_POINT ( 'NONE', #1681 ) ;
#47361 = CARTESIAN_POINT ( 'NONE',  ( 29.07187500061451502, -6.054752690667223547, -1.112240025338166033E-15 ) ) ;
#47362 = CARTESIAN_POINT ( 'NONE',  ( 22.86562500061451431, 3.027376345333613106, -5.243569643749998122 ) ) ;
#47363 =( BOUNDED_SURFACE ( )  B_SPLINE_SURFACE ( 1, 2, ( 
 ( #42519, #3374, #8168, #25147, #42153, #9635, #64680, #65409, #43260, #14799, #37342, #48798, #14065, #54702, #59865, #65781, #24784, #16618, #71702, #49532, #72056, #10000, #4472, #32535, #33616, #21074, #43625, #55798, #72789, #56160, #60966, #11456, #66147, #39537, #60591, #66892, #25, #55071, #5188, #27002, #43992, #22172, #5555, #67260, #28092, #10365, #50620, #22531, #39173, #11088, #44725, #50264, #10728, #21435, #61689, #15525, #66513, #45078, #67614, #15894, #32896, #33260, #38067, #4828, #38440, #49893, #55436, #27362, #72418, #21801, #44365, #16260, #16980, #62062, #49171, #33977, #27726, #4107, #38815, #61330, #26634, #41349, #51342, #18784, #1470, #40260, #29531, #50978, #46162, #63859, #23253, #57951, #45441, #23976, #56516, #1109, #62781, #11818, #13249, #62419, #28801, #46524, #12894, #12537, #6273, #34335, #35071, #5909, #12173, #56869, #744, #68702, #28443, #375, #45803, #67974, #7359, #34701, #22883, #69066, #23616, #57230, #1833, #6645, #57597, #29172, #51706, #17347, #7000, #18062, #29888, #68339, #52066, #39906, #17699, #40623, #63142, #18425, #40991, #63507, #35427, #52427, #24341, #46889, #69427, #42074, #53893, #31352, #52788, #25812, #36888, #41701, #13614, #59778, #70511, #48350, #70138, #59042, #64596, #54255, #3651, #25440, #35787, #9184, #59407, #30255, #47247, #25065, #58310, #26174, #48715, #58677, #2909, #19147, #71237, #47983, #19516, #69780, #8815, #7721, #42440, #20617, #14353, #13983, #43175, #19887, #20249, #36522, #3284, #70875, #31719, #64225, #36159, #42801, #65323, #65694, #8087, #64962, #30617, #14714, #37256, #53515, #2189, #24703, #8446, #53147, #2546, #47608, #30982, #60878, #72704, #37983, #54614, #39089, #38730, #61606, #71978, #44645, #72337, #60505, #50537, #11007, #56078, #67175, #33528, #5469, #33174, #10283, #27279, #21351, #20987, #22087, #32813, #32449, #16536, #28009, #15809, #9911, #66431, #49812, #16179, #55712, #43908, #21717, #4020, #32083, #60140, #73065, #43540, #5106, #22446, #38351, #61250, #44995, #37618, #15081, #55351, #66807, #15439, #27640, #9549, #54984, #4390, #66061, #26919, #49444, #26545, #49086, #71614, #10644, #50176, #4745, #44276, #1744, #61971, #29806, #50894, #57144, #63422, #22803, #68615, #294, #34250, #12455, #23893, #57515, #46441, #51257, #68979, #12809, #6916, #1383, #34986, #40537, #1024, #45355, #51984, #33892, #67889, #29446, #63053, #6188, #659, #23530, #5827, #68256, #39823, #40178, #17261, #23167, #62337, #56436, #11733, #11373, #18336, #40909, #39450, #35344, #46080, #57867, #28358, #62698, #56782, #52341, #28717, #24257, #7276, #45721, #67532, #17618, #6556, #16895, #12093, #34614, #29088, #51624, #17978, #64508, #30536, #2107, #3565, #58594, #48262, #36440, #19062, #20161, #59317, #54168, #24618, #13901, #58227, #64139, #41264, #47165, #69697, #47897, #52701, #41620, #70786, #8362, #36802, #8001, #70054, #2457, #65236, #14626, #58954, #46805, #42715, #70425, #63776, #7632, #36073, #69342, #37165, #59691, #13526, #30891, #30170, #9098, #53433, #53063, #24980, #19800, #18700, #2823, #31636, #25351, #47525, #13164, #42353, #31260, #19427, #64875, #14263, #35705, #41988, #8726, #53802, #3197, #25725, #48996, #38260, #54531, #38640, #10559, #43819, #72253, #61521, #71892, #14996, #65608, #60788, #66343, #21265, #33087, #71526, #37533, #50088, #49726, #72619, #9828, #55626, #10194, #20901, #10919, #22003, #67090, #5022, #44559, #16449, #44188, #31996, #43455, #16092, #27557, #55266, #65977, #3933, #4661, #26088, #32358, #26456, #15357, #15721, #48626, #33446, #37899, #60055, #39006, #54896, #55990, #61164, #32729, #4303, #71151, #26828, #27191, #49362, #21630, #20523, #66719, #43082, #9466, #60417, #6467, #50455, #44915, #72981, #28635, #36262, #6104, #11652, #45272, #45640, #67805, #56356, #67452, #34167, #23447, #940, #22363, #68530, #17179, #16814, #6830, #62255, #5383, #17891, #23082, #56703, #23805, #51173, #29002, #577, #68172, #39370, #34530, #17535, #29365, #22719, #51539, #61887, #11292, #33813, #40097, #27921, #62611, #12007, #39738, #57060, #45993, #5746, #28280, #40451, #62967, #12363, #50812, #34897, #57426, #214, #51897, #1295, #46356, #68890, #18247, #40820, #63336, #13721, #4122, #48452, #58777, #9652, #9287, #53247, #70244, #48082, #8186, #26651, #71717, #8552, #25912, #42172, #49187, #70976, #42535, #19615, #31820, #30714, #65426, #21089, #37359, #19982, #66164, #20351, #43277, #14452, #59881, #3753, #32186, #64698, #59143, #48814, #54359, #43640, #31079, #42902, #14082, #71344, #65798, #3391, #26277, #15540, #31452, #47705, #25164, #14816, #20719, #53994, #15179, #53619, #36622, #54719, #37718, #2645, #65061, #60238, #3010, #25540, #70609, #36986, #59508, #8922, #33994, #28458, #56178, #44007, #10382, #28108, #67629, #67277, #60983, #15909, #16636, #38084, #44383, #38457, #32914, #27743, #60606, #22898, #72806, #39191, #5571, #66908, #44743, #27017, #55088, #10015, #391, #66529, #50637, #11471, #61347, #61706, #45094, #32551, #45457, #16276, #11105, #55451, #41, #4488, #4844, #27378, #49910, #72434, #21818, #16996, #49549, #72071, #33634, #22546, #39553, #38832, #67989, #21452, #10743, #33276, #50282, #56531, #55815, #62078, #5202, #22189, #5924, #50993, #7373, #46905, #1121, #18801, #13266, #29904, #24357, #35441, #63521, #23991, #23266, #1849, #56883, #45816, #57965, #12908, #29186, #23630, #46538, #28817, #18075, #62794, #63155, #40273, #46176, #17713, #6288, #12187, #11832, #52444, #69444, #62434, #41365, #69080, #63875, #51355, #12550, #34714, #2206, #57244, #52805, #35804, #68715, #58326, #34350, #7013, #24721, #6657, #7737, #758, #30272, #17363, #35084, #40636, #68352, #47264, #51720, #39920, #29544, #57610, #52080, #1485, #18441, #41006 ),
 ( #19905, #69798, #9202, #53911, #13633, #8105, #14001, #19164, #26192, #71255, #19535, #42457, #53165, #48732, #64980, #8465, #30633, #3304, #64245, #59426, #20635, #31370, #59060, #41718, #8834, #59796, #48002, #48368, #42819, #3669, #25082, #64615, #14732, #70894, #20267, #25458, #36540, #54275, #31000, #36177, #37274, #58694, #53533, #25831, #42093, #70530, #47625, #2929, #14371, #65342, #31737, #36906, #2562, #70158, #35312, #6885, #69662, #30501, #63391, #57481, #40874, #24223, #63743, #30136, #68945, #69308, #51594, #6525, #34585, #24946, #17945, #7597, #36037, #12776, #13132, #19027, #12062, #70020, #18303, #41231, #63022, #2074, #57113, #34953, #29418, #68584, #12421, #40507, #41586, #29057, #994, #35671, #58194, #64104, #46408, #19391, #23501, #47490, #46049, #52308, #58557, #51951, #52667, #1351, #23860, #24583, #13489, #47131, #7965, #57834, #53029, #2423, #62667, #7243, #29772, #1710, #18669, #46772, #26420, #8328, #47860, #60020, #37500, #53767, #25691, #48593, #71118, #70389, #48961, #30858, #19765, #9432, #31960, #3162, #48226, #20490, #53396, #42680, #14229, #14592, #64842, #70750, #42316, #2789, #36767, #36407, #54498, #3899, #13866, #71491, #43046, #43421, #25314, #37127, #59284, #26793, #8693, #4269, #20868, #20125, #14962, #58920, #31599, #49327, #31225, #65943, #65203, #15323, #41952, #59656, #9065, #54136, #65572, #3531, #26053, #37864, #60383, #9791, #32324, #71859, #54861, #64472, #30850, #59276, #14221, #19757, #31590, #70013, #13479, #71111, #70739, #20483, #53385, #3524, #31216, #19382, #9424, #43038, #14954, #26045, #65565, #37493, #65195, #53021, #41941, #37119, #48585, #3153, #64464, #24937, #25682, #47121, #2780, #47480, #13856, #36757, #69653, #31953, #36398, #36029, #60013, #25305, #3891, #59648, #64833, #47852, #54491, #70379, #48217, #42306, #8684, #41578, #20117, #53759, #19017, #58911, #42672, #64095, #58545, #7956, #14585, #30493, #9058, #54128, #8321, #2415, #66303, #4262, #65936, #32688, #45506, #22945, #43411, #49685, #57294, #27151, #55227, #15680, #66674, #38218, #26785, #15316, #4622, #68036, #17406, #37855, #39963, #28502, #32317, #49320, #51401, #62122, #62477, #60745, #72214, #21592, #45860, #68394, #17043, #26411, #804, #51040, #20859, #60376, #10156, #48954, #17755, #40315, #71851, #39601, #9784, #62838, #11514, #44146, #54853, #436, #71484, #34036, #12230, #5971, #56575, #34759, #11875, #34399, #56927, #6331, #28862, #23311, #21224, #43776, #69839, #7780, #46220, #29232, #30317, #63199, #19204, #64287, #24399, #52847, #57653, #12595, #58369, #63563, #18844, #46948, #52484, #13675, #29587, #68759, #30673, #2245, #53205, #12951, #36219, #63921, #52125, #42130, #2601, #47664, #58735, #25122, #70198, #24761, #35128, #1527, #41758, #8146, #35844, #24034, #7059, #47304, #6699, #35488, #46583, #69126, #69485, #51765, #64656, #18484, #18117, #19574, #58008, #36581, #14041, #41405, #7416, #1164, #29944, #23673, #1895, #13306, #40681, #41050, #65383, #9971, #3349, #60198, #31037, #25499, #53573, #48044, #2971, #70569, #21408, #14410, #4077, #32508, #9245, #9610, #66119, #8508, #66486, #14774, #37676, #59467, #71672, #19945, #31412, #53952, #65021, #8877, #36947, #15498, #42498, #25871, #32141, #54674, #38040, #42861, #15865, #48411, #43965, #70937, #48774, #55043, #20308, #26605, #37316, #59840, #49143, #60564, #21046, #4446, #31780, #26974, #49503, #43598, #72032, #59101, #54319, #65754, #3710, #26237, #71298, #20677, #43234, #15138, #50236, #22144, #45052, #49867, #39143, #10699, #11060, #61304, #67231, #38787, #27335, #33231, #32870, #50952, #5883, #10338, #67946, #67588, #39879, #4802, #33586, #55769, #23223, #5161, #716, #56489, #44697, #11429, #55407, #28063, #45776, #27696, #62391, #72391, #28414, #38413, #56132, #16590, #66863, #62033, #61660, #72758, #17319, #5525, #11789, #349, #68311, #60934, #21771, #44335, #50593, #16234, #48581, #22503, #16954, #39507, #33948, #22856, #45410, #34306, #56838, #6245, #28772, #51312, #12512, #69035, #52398, #18758, #58284, #23947, #24314, #8058, #69402, #52038, #25038, #7331, #2163, #46497, #41322, #35762, #41675, #51678, #18036, #7690, #63832, #57200, #40231, #13223, #1082, #30228, #24674, #35399, #52760, #68673, #23589, #47221, #1442, #29862, #57925, #63480, #69752, #40592, #6616, #64198, #19121, #13585, #18397, #36132, #1806, #63113, #53119, #58651, #30592, #2517, #47582, #17671, #62753, #46135, #35041, #12146, #34672, #46863, #57568, #6972, #29143, #29503, #40964, #12867, #47955, #59747, #19487, #54954, #59375, #59014, #71582, #53863, #26887, #9521, #14681, #3254, #15412, #25783, #71207, #20218, #42773, #64568, #26143, #48320, #20955, #14323, #20584, #42045, #36494, #13957, #65292, #70111, #70845, #37223, #36858, #9154, #8785, #70482, #8417, #31689, #15052, #65662, #30949, #60111, #43139, #2880, #19859, #43509, #54224, #32054, #31320, #3621, #48683, #37954, #60473, #37590, #53488, #66033, #54586, #25410, #42412, #3989, #64932, #9882, #32417, #26515, #49054, #4359, #39790, #16505, #33142, #60845, #73033, #71946, #56045, #49782, #55320, #5796, #43875, #66400, #27976, #44963, #28326, #55680, #56752, #15777, #11703, #32783, #39058, #45323, #4714, #50507, #27248, #16147, #67501, #50864, #39420, #262, #5077, #22771, #67859, #61941, #56405, #16865, #22416, #5437, #72306, #33862, #38319, #21688, #11345, #17230, #61218, #27610, #62307, #10252, #50146, #44244, #22057, #66775, #72674, #38699, #10613, #44615, #67145, #34219, #6157, #21322, #49414, #61572, #10975, #33496, #23858, #29055, #13486, #23499, #64102, #46770, #12419, #1707, #23136, #18301, #36035, #68582, #30134, #17588, #69306, #28686, #46406, #34951, #57111, #52306, #57479, #51592, #7595, #992, #2072, #41228, #58555 ) ),
 .UNSPECIFIED., .F., .F., .F. ) 
 B_SPLINE_SURFACE_WITH_KNOTS ( ( 2, 2 ),
 ( 3, 2, 2, 2, 2, 2, 2, 2, 2, 2, 2, 2, 2, 2, 2, 2, 2, 2, 2, 2, 2, 2, 2, 2, 2, 2, 2, 2, 2, 2, 2, 2, 2, 2, 2, 2, 2, 2, 2, 2, 2, 2, 2, 2, 2, 2, 2, 2, 2, 2, 2, 2, 2, 2, 2, 2, 2, 2, 2, 2, 2, 2, 2, 2, 2, 2, 2, 2, 2, 2, 2, 2, 2, 2, 2, 2, 2, 2, 2, 2, 2, 2, 2, 2, 2, 2, 2, 2, 2, 2, 2, 2, 2, 2, 2, 2, 2, 2, 2, 2, 2, 2, 2, 2, 2, 2, 2, 2, 2, 2, 2, 2, 2, 2, 2, 2, 2, 2, 2, 2, 2, 2, 2, 2, 2, 2, 2, 2, 2, 2, 2, 2, 2, 2, 2, 2, 2, 2, 2, 2, 2, 2, 2, 2, 2, 2, 2, 2, 2, 2, 2, 2, 2, 2, 2, 2, 2, 2, 2, 2, 2, 2, 2, 2, 2, 2, 2, 2, 2, 2, 2, 2, 2, 2, 2, 2, 2, 2, 2, 2, 2, 2, 2, 2, 2, 2, 2, 2, 2, 2, 2, 2, 2, 2, 2, 2, 2, 2, 2, 2, 2, 2, 2, 2, 2, 2, 2, 2, 2, 2, 2, 2, 2, 2, 2, 2, 2, 2, 2, 2, 2, 2, 2, 2, 2, 2, 2, 2, 2, 2, 2, 2, 2, 2, 2, 2, 2, 2, 2, 2, 2, 2, 2, 2, 2, 2, 2, 2, 2, 2, 2, 2, 2, 2, 2, 2, 2, 2, 2, 2, 2, 2, 2, 2, 2, 2, 2, 2, 2, 2, 2, 2, 2, 2, 2, 2, 2, 2, 2, 2, 2, 2, 2, 2, 2, 2, 2, 2, 2, 2, 2, 2, 2, 2, 2, 2, 2, 2, 2, 2, 2, 2, 2, 2, 2, 2, 2, 2, 2, 2, 2, 2, 2, 2, 2, 2, 2, 2, 2, 2, 2, 2, 2, 2, 2, 2, 2, 2, 2, 2, 2, 2, 2, 2, 2, 2, 2, 2, 2, 2, 2, 2, 2, 2, 2, 2, 2, 2, 2, 2, 2, 2, 2, 2, 2, 2, 2, 2, 2, 2, 3 ),
 ( 0.000000000000000000, 1.000000000000000000 ),
 ( 0.000000000000000000, 0.002777777777777777884, 0.005555555555555555768, 0.008333333333333333218, 0.01111111111111111154, 0.01388888888888888812, 0.01666666666666666644, 0.01944444444444444475, 0.02222222222222222307, 0.02500000000000000139, 0.02777777777777777624, 0.03055555555555555455, 0.03333333333333333287, 0.03611111111111110772, 0.03888888888888888951, 0.04166666666666666435, 0.04444444444444444614, 0.04722222222222222099, 0.05000000000000000278, 0.05277777777777777762, 0.05555555555555555247, 0.05833333333333333426, 0.06111111111111110911, 0.06388888888888888395, 0.06666666666666666574, 0.06944444444444444753, 0.07222222222222221544, 0.07499999999999999722, 0.07777777777777777901, 0.08055555555555556080, 0.08333333333333332871, 0.08611111111111111049, 0.08888888888888889228, 0.09166666666666666019, 0.09444444444444444198, 0.09722222222222222376, 0.1000000000000000056, 0.1027777777777777735, 0.1055555555555555552, 0.1083333333333333370, 0.1111111111111111049, 0.1138888888888888867, 0.1166666666666666685, 0.1194444444444444503, 0.1222222222222222182, 0.1250000000000000000, 0.1277777777777777679, 0.1305555555555555636, 0.1333333333333333315, 0.1361111111111110994, 0.1388888888888888951, 0.1416666666666666630, 0.1444444444444444309, 0.1472222222222222265, 0.1499999999999999944, 0.1527777777777777901, 0.1555555555555555580, 0.1583333333333333259, 0.1611111111111111216, 0.1638888888888888895, 0.1666666666666666574, 0.1694444444444444531, 0.1722222222222222210, 0.1749999999999999889, 0.1777777777777777846, 0.1805555555555555525, 0.1833333333333333204, 0.1861111111111111160, 0.1888888888888888840, 0.1916666666666666796, 0.1944444444444444475, 0.1972222222222222154, 0.2000000000000000111, 0.2027777777777777790, 0.2055555555555555469, 0.2083333333333333426, 0.2111111111111111105, 0.2138888888888888784, 0.2166666666666666741, 0.2194444444444444420, 0.2222222222222222099, 0.2250000000000000056, 0.2277777777777777735, 0.2305555555555555691, 0.2333333333333333370, 0.2361111111111111049, 0.2388888888888889006, 0.2416666666666666685, 0.2444444444444444364, 0.2472222222222222321, 0.2500000000000000000, 0.2527777777777777679, 0.2555555555555555358, 0.2583333333333333592, 0.2611111111111111271, 0.2638888888888888951, 0.2666666666666666630, 0.2694444444444444309, 0.2722222222222221988, 0.2750000000000000222, 0.2777777777777777901, 0.2805555555555555580, 0.2833333333333333259, 0.2861111111111110938, 0.2888888888888888618, 0.2916666666666666852, 0.2944444444444444531, 0.2972222222222222210, 0.2999999999999999889, 0.3027777777777777568, 0.3055555555555555802, 0.3083333333333333481, 0.3111111111111111160, 0.3138888888888888840, 0.3166666666666666519, 0.3194444444444444198, 0.3222222222222222432, 0.3250000000000000111, 0.3277777777777777790, 0.3305555555555555469, 0.3333333333333333148, 0.3361111111111111382, 0.3388888888888889062, 0.3416666666666666741, 0.3444444444444444420, 0.3472222222222222099, 0.3499999999999999778, 0.3527777777777778012, 0.3555555555555555691, 0.3583333333333333370, 0.3611111111111111049, 0.3638888888888888729, 0.3666666666666666408, 0.3694444444444444642, 0.3722222222222222321, 0.3750000000000000000, 0.3777777777777777679, 0.3805555555555555358, 0.3833333333333333592, 0.3861111111111111271, 0.3888888888888888951, 0.3916666666666666630, 0.3944444444444444309, 0.3972222222222221988, 0.4000000000000000222, 0.4027777777777777901, 0.4055555555555555580, 0.4083333333333333259, 0.4111111111111110938, 0.4138888888888888618, 0.4166666666666666852, 0.4194444444444444531, 0.4222222222222222210, 0.4249999999999999889, 0.4277777777777777568, 0.4305555555555555802, 0.4333333333333333481, 0.4361111111111111160, 0.4388888888888888840, 0.4416666666666666519, 0.4444444444444444198, 0.4472222222222222432, 0.4500000000000000111, 0.4527777777777777790, 0.4555555555555555469, 0.4583333333333333148, 0.4611111111111111382, 0.4638888888888889062, 0.4666666666666666741, 0.4694444444444444420, 0.4722222222222222099, 0.4749999999999999778, 0.4777777777777778012, 0.4805555555555555691, 0.4833333333333333370, 0.4861111111111111049, 0.4888888888888888729, 0.4916666666666666408, 0.4944444444444444642, 0.4972222222222222321, 0.5000000000000000000, 0.5027777777777777679, 0.5055555555555555358, 0.5083333333333333037, 0.5111111111111110716, 0.5138888888888888395, 0.5166666666666667185, 0.5194444444444444864, 0.5222222222222222543, 0.5250000000000000222, 0.5277777777777777901, 0.5305555555555555580, 0.5333333333333333259, 0.5361111111111110938, 0.5388888888888888618, 0.5416666666666666297, 0.5444444444444443976, 0.5472222222222222765, 0.5500000000000000444, 0.5527777777777778123, 0.5555555555555555802, 0.5583333333333333481, 0.5611111111111111160, 0.5638888888888888840, 0.5666666666666666519, 0.5694444444444444198, 0.5722222222222221877, 0.5749999999999999556, 0.5777777777777777235, 0.5805555555555556024, 0.5833333333333333703, 0.5861111111111111382, 0.5888888888888889062, 0.5916666666666666741, 0.5944444444444444420, 0.5972222222222222099, 0.5999999999999999778, 0.6027777777777777457, 0.6055555555555555136, 0.6083333333333332815, 0.6111111111111111605, 0.6138888888888889284, 0.6166666666666666963, 0.6194444444444444642, 0.6222222222222222321, 0.6250000000000000000, 0.6277777777777777679, 0.6305555555555555358, 0.6333333333333333037, 0.6361111111111110716, 0.6388888888888888395, 0.6416666666666667185, 0.6444444444444444864, 0.6472222222222222543, 0.6500000000000000222, 0.6527777777777777901, 0.6555555555555555580, 0.6583333333333333259, 0.6611111111111110938, 0.6638888888888888618, 0.6666666666666666297, 0.6694444444444443976, 0.6722222222222222765, 0.6750000000000000444, 0.6777777777777778123, 0.6805555555555555802, 0.6833333333333333481, 0.6861111111111111160, 0.6888888888888888840, 0.6916666666666666519, 0.6944444444444444198, 0.6972222222222221877, 0.6999999999999999556, 0.7027777777777777235, 0.7055555555555556024, 0.7083333333333333703, 0.7111111111111111382, 0.7138888888888889062, 0.7166666666666666741, 0.7194444444444444420, 0.7222222222222222099, 0.7249999999999999778, 0.7277777777777777457, 0.7305555555555555136, 0.7333333333333332815, 0.7361111111111111605, 0.7388888888888889284, 0.7416666666666666963, 0.7444444444444444642, 0.7472222222222222321, 0.7500000000000000000, 0.7527777777777777679, 0.7555555555555555358, 0.7583333333333333037, 0.7611111111111110716, 0.7638888888888888395, 0.7666666666666667185, 0.7694444444444444864, 0.7722222222222222543, 0.7750000000000000222, 0.7777777777777777901, 0.7805555555555555580, 0.7833333333333333259, 0.7861111111111110938, 0.7888888888888888618, 0.7916666666666666297, 0.7944444444444443976, 0.7972222222222222765, 0.8000000000000000444, 0.8027777777777778123, 0.8055555555555555802, 0.8083333333333333481, 0.8111111111111111160, 0.8138888888888888840, 0.8166666666666666519, 0.8194444444444444198, 0.8222222222222221877, 0.8249999999999999556, 0.8277777777777777235, 0.8305555555555556024, 0.8333333333333333703, 0.8361111111111111382, 0.8388888888888889062, 0.8416666666666666741, 0.8444444444444444420, 0.8472222222222222099, 0.8499999999999999778, 0.8527777777777777457, 0.8555555555555555136, 0.8583333333333332815, 0.8611111111111111605, 0.8638888888888889284, 0.8666666666666666963, 0.8694444444444444642, 0.8722222222222222321, 0.8750000000000000000, 0.8777777777777777679, 0.8805555555555555358, 0.8833333333333333037, 0.8861111111111110716, 0.8888888888888888395, 0.8916666666666667185, 0.8944444444444444864, 0.8972222222222222543, 0.9000000000000000222, 0.9027777777777777901, 0.9055555555555555580, 0.9083333333333333259, 0.9111111111111110938, 0.9138888888888888618, 0.9166666666666666297, 0.9194444444444443976, 0.9222222222222222765, 0.9250000000000000444, 0.9277777777777778123, 0.9305555555555555802, 0.9333333333333333481, 0.9361111111111111160, 0.9388888888888888840, 0.9416666666666666519, 0.9444444444444444198, 0.9472222222222221877, 0.9499999999999999556, 0.9527777777777777235, 0.9555555555555556024, 0.9583333333333333703, 0.9611111111111111382, 0.9638888888888889062, 0.9666666666666666741, 0.9694444444444444420, 0.9722222222222222099, 0.9749999999999999778, 0.9777777777777777457, 0.9805555555555555136, 0.9833333333333332815, 0.9861111111111111605, 0.9888888888888889284, 0.9916666666666666963, 0.9944444444444444642, 0.9972222222222222321, 1.000000000000000000 ),
 .UNSPECIFIED. ) 
 GEOMETRIC_REPRESENTATION_ITEM ( )  RATIONAL_B_SPLINE_SURFACE ( (
 ( 1.000000000000000000, 0.8660254037844387076, 1.000000000000000000, 0.8660254037844387076, 1.000000000000000000, 0.8660254037844387076, 1.000000000000000000, 0.8660254037844387076, 1.000000000000000000, 0.8660254037844387076, 1.000000000000000000, 0.8660254037844387076, 1.000000000000000000, 0.8660254037844387076, 1.000000000000000000, 0.8660254037844387076, 1.000000000000000000, 0.8660254037844387076, 1.000000000000000000, 0.8660254037844387076, 1.000000000000000000, 0.8660254037844387076, 1.000000000000000000, 0.8660254037844387076, 1.000000000000000000, 0.8660254037844387076, 1.000000000000000000, 0.8660254037844387076, 1.000000000000000000, 0.8660254037844387076, 1.000000000000000000, 0.8660254037844387076, 1.000000000000000000, 0.8660254037844387076, 1.000000000000000000, 0.8660254037844387076, 1.000000000000000000, 0.8660254037844387076, 1.000000000000000000, 0.8660254037844387076, 1.000000000000000000, 0.8660254037844387076, 1.000000000000000000, 0.8660254037844387076, 1.000000000000000000, 0.8660254037844387076, 1.000000000000000000, 0.8660254037844387076, 1.000000000000000000, 0.8660254037844387076, 1.000000000000000000, 0.8660254037844387076, 1.000000000000000000, 0.8660254037844387076, 1.000000000000000000, 0.8660254037844387076, 1.000000000000000000, 0.8660254037844387076, 1.000000000000000000, 0.8660254037844387076, 1.000000000000000000, 0.8660254037844387076, 1.000000000000000000, 0.8660254037844387076, 1.000000000000000000, 0.8660254037844387076, 1.000000000000000000, 0.8660254037844387076, 1.000000000000000000, 0.8660254037844387076, 1.000000000000000000, 0.8660254037844387076, 1.000000000000000000, 0.8660254037844387076, 1.000000000000000000, 0.8660254037844387076, 1.000000000000000000, 0.8660254037844387076, 1.000000000000000000, 0.8660254037844387076, 1.000000000000000000, 0.8660254037844387076, 1.000000000000000000, 0.8660254037844387076, 1.000000000000000000, 0.8660254037844387076, 1.000000000000000000, 0.8660254037844387076, 1.000000000000000000, 0.8660254037844387076, 1.000000000000000000, 0.8660254037844387076, 1.000000000000000000, 0.8660254037844387076, 1.000000000000000000, 0.8660254037844387076, 1.000000000000000000, 0.8660254037844387076, 1.000000000000000000, 0.8660254037844387076, 1.000000000000000000, 0.8660254037844387076, 1.000000000000000000, 0.8660254037844387076, 1.000000000000000000, 0.8660254037844387076, 1.000000000000000000, 0.8660254037844387076, 1.000000000000000000, 0.8660254037844387076, 1.000000000000000000, 0.8660254037844387076, 1.000000000000000000, 0.8660254037844387076, 1.000000000000000000, 0.8660254037844387076, 1.000000000000000000, 0.8660254037844387076, 1.000000000000000000, 0.8660254037844387076, 1.000000000000000000, 0.8660254037844387076, 1.000000000000000000, 0.8660254037844387076, 1.000000000000000000, 0.8660254037844387076, 1.000000000000000000, 0.8660254037844387076, 1.000000000000000000, 0.8660254037844387076, 1.000000000000000000, 0.8660254037844387076, 1.000000000000000000, 0.8660254037844387076, 1.000000000000000000, 0.8660254037844387076, 1.000000000000000000, 0.8660254037844387076, 1.000000000000000000, 0.8660254037844387076, 1.000000000000000000, 0.8660254037844387076, 1.000000000000000000, 0.8660254037844387076, 1.000000000000000000, 0.8660254037844387076, 1.000000000000000000, 0.8660254037844387076, 1.000000000000000000, 0.8660254037844387076, 1.000000000000000000, 0.8660254037844387076, 1.000000000000000000, 0.8660254037844387076, 1.000000000000000000, 0.8660254037844387076, 1.000000000000000000, 0.8660254037844387076, 1.000000000000000000, 0.8660254037844387076, 1.000000000000000000, 0.8660254037844387076, 1.000000000000000000, 0.8660254037844387076, 1.000000000000000000, 0.8660254037844387076, 1.000000000000000000, 0.8660254037844387076, 1.000000000000000000, 0.8660254037844387076, 1.000000000000000000, 0.8660254037844387076, 1.000000000000000000, 0.8660254037844387076, 1.000000000000000000, 0.8660254037844387076, 1.000000000000000000, 0.8660254037844387076, 1.000000000000000000, 0.8660254037844387076, 1.000000000000000000, 0.8660254037844387076, 1.000000000000000000, 0.8660254037844387076, 1.000000000000000000, 0.8660254037844387076, 1.000000000000000000, 0.8660254037844387076, 1.000000000000000000, 0.8660254037844387076, 1.000000000000000000, 0.8660254037844387076, 1.000000000000000000, 0.8660254037844387076, 1.000000000000000000, 0.8660254037844387076, 1.000000000000000000, 0.8660254037844387076, 1.000000000000000000, 0.8660254037844387076, 1.000000000000000000, 0.8660254037844387076, 1.000000000000000000, 0.8660254037844387076, 1.000000000000000000, 0.8660254037844387076, 1.000000000000000000, 0.8660254037844387076, 1.000000000000000000, 0.8660254037844387076, 1.000000000000000000, 0.8660254037844387076, 1.000000000000000000, 0.8660254037844387076, 1.000000000000000000, 0.8660254037844387076, 1.000000000000000000, 0.8660254037844387076, 1.000000000000000000, 0.8660254037844387076, 1.000000000000000000, 0.8660254037844387076, 1.000000000000000000, 0.8660254037844387076, 1.000000000000000000, 0.8660254037844387076, 1.000000000000000000, 0.8660254037844387076, 1.000000000000000000, 0.8660254037844387076, 1.000000000000000000, 0.8660254037844387076, 1.000000000000000000, 0.8660254037844387076, 1.000000000000000000, 0.8660254037844387076, 1.000000000000000000, 0.8660254037844387076, 1.000000000000000000, 0.8660254037844387076, 1.000000000000000000, 0.8660254037844387076, 1.000000000000000000, 0.8660254037844387076, 1.000000000000000000, 0.8660254037844387076, 1.000000000000000000, 0.8660254037844387076, 1.000000000000000000, 0.8660254037844387076, 1.000000000000000000, 0.8660254037844387076, 1.000000000000000000, 0.8660254037844387076, 1.000000000000000000, 0.8660254037844387076, 1.000000000000000000, 0.8660254037844387076, 1.000000000000000000, 0.8660254037844387076, 1.000000000000000000, 0.8660254037844387076, 1.000000000000000000, 0.8660254037844387076, 1.000000000000000000, 0.8660254037844387076, 1.000000000000000000, 0.8660254037844387076, 1.000000000000000000, 0.8660254037844387076, 1.000000000000000000, 0.8660254037844387076, 1.000000000000000000, 0.8660254037844387076, 1.000000000000000000, 0.8660254037844387076, 1.000000000000000000, 0.8660254037844387076, 1.000000000000000000, 0.8660254037844387076, 1.000000000000000000, 0.8660254037844387076, 1.000000000000000000, 0.8660254037844387076, 1.000000000000000000, 0.8660254037844387076, 1.000000000000000000, 0.8660254037844387076, 1.000000000000000000, 0.8660254037844387076, 1.000000000000000000, 0.8660254037844387076, 1.000000000000000000, 0.8660254037844387076, 1.000000000000000000, 0.8660254037844387076, 1.000000000000000000, 0.8660254037844387076, 1.000000000000000000, 0.8660254037844387076, 1.000000000000000000, 0.8660254037844387076, 1.000000000000000000, 0.8660254037844387076, 1.000000000000000000, 0.8660254037844387076, 1.000000000000000000, 0.8660254037844387076, 1.000000000000000000, 0.8660254037844387076, 1.000000000000000000, 0.8660254037844387076, 1.000000000000000000, 0.8660254037844387076, 1.000000000000000000, 0.8660254037844387076, 1.000000000000000000, 0.8660254037844387076, 1.000000000000000000, 0.8660254037844387076, 1.000000000000000000, 0.8660254037844387076, 1.000000000000000000, 0.8660254037844387076, 1.000000000000000000, 0.8660254037844387076, 1.000000000000000000, 0.8660254037844387076, 1.000000000000000000, 0.8660254037844387076, 1.000000000000000000, 0.8660254037844387076, 1.000000000000000000, 0.8660254037844387076, 1.000000000000000000, 0.8660254037844387076, 1.000000000000000000, 0.8660254037844387076, 1.000000000000000000, 0.8660254037844387076, 1.000000000000000000, 0.8660254037844387076, 1.000000000000000000, 0.8660254037844387076, 1.000000000000000000, 0.8660254037844387076, 1.000000000000000000, 0.8660254037844387076, 1.000000000000000000, 0.8660254037844387076, 1.000000000000000000, 0.8660254037844387076, 1.000000000000000000, 0.8660254037844387076, 1.000000000000000000, 0.8660254037844387076, 1.000000000000000000, 0.8660254037844387076, 1.000000000000000000, 0.8660254037844387076, 1.000000000000000000, 0.8660254037844387076, 1.000000000000000000, 0.8660254037844387076, 1.000000000000000000, 0.8660254037844387076, 1.000000000000000000, 0.8660254037844387076, 1.000000000000000000, 0.8660254037844387076, 1.000000000000000000, 0.8660254037844387076, 1.000000000000000000, 0.8660254037844387076, 1.000000000000000000, 0.8660254037844387076, 1.000000000000000000, 0.8660254037844387076, 1.000000000000000000, 0.8660254037844387076, 1.000000000000000000, 0.8660254037844387076, 1.000000000000000000, 0.8660254037844387076, 1.000000000000000000, 0.8660254037844387076, 1.000000000000000000, 0.8660254037844387076, 1.000000000000000000, 0.8660254037844387076, 1.000000000000000000, 0.8660254037844387076, 1.000000000000000000, 0.8660254037844387076, 1.000000000000000000, 0.8660254037844387076, 1.000000000000000000, 0.8660254037844387076, 1.000000000000000000, 0.8660254037844387076, 1.000000000000000000, 0.8660254037844387076, 1.000000000000000000, 0.8660254037844387076, 1.000000000000000000, 0.8660254037844387076, 1.000000000000000000, 0.8660254037844387076, 1.000000000000000000, 0.8660254037844387076, 1.000000000000000000, 0.8660254037844387076, 1.000000000000000000, 0.8660254037844387076, 1.000000000000000000, 0.8660254037844387076, 1.000000000000000000, 0.8660254037844387076, 1.000000000000000000, 0.8660254037844387076, 1.000000000000000000, 0.8660254037844387076, 1.000000000000000000, 0.8660254037844387076, 1.000000000000000000, 0.8660254037844387076, 1.000000000000000000, 0.8660254037844387076, 1.000000000000000000, 0.8660254037844387076, 1.000000000000000000, 0.8660254037844387076, 1.000000000000000000, 0.8660254037844387076, 1.000000000000000000, 0.8660254037844387076, 1.000000000000000000, 0.8660254037844387076, 1.000000000000000000, 0.8660254037844387076, 1.000000000000000000, 0.8660254037844387076, 1.000000000000000000, 0.8660254037844387076, 1.000000000000000000, 0.8660254037844387076, 1.000000000000000000, 0.8660254037844387076, 1.000000000000000000, 0.8660254037844387076, 1.000000000000000000, 0.8660254037844387076, 1.000000000000000000, 0.8660254037844387076, 1.000000000000000000, 0.8660254037844387076, 1.000000000000000000, 0.8660254037844387076, 1.000000000000000000, 0.8660254037844387076, 1.000000000000000000, 0.8660254037844387076, 1.000000000000000000, 0.8660254037844387076, 1.000000000000000000, 0.8660254037844387076, 1.000000000000000000, 0.8660254037844387076, 1.000000000000000000, 0.8660254037844387076, 1.000000000000000000, 0.8660254037844387076, 1.000000000000000000, 0.8660254037844387076, 1.000000000000000000, 0.8660254037844387076, 1.000000000000000000, 0.8660254037844387076, 1.000000000000000000, 0.8660254037844387076, 1.000000000000000000, 0.8660254037844387076, 1.000000000000000000, 0.8660254037844387076, 1.000000000000000000, 0.8660254037844387076, 1.000000000000000000, 0.8660254037844387076, 1.000000000000000000, 0.8660254037844387076, 1.000000000000000000, 0.8660254037844387076, 1.000000000000000000, 0.8660254037844387076, 1.000000000000000000, 0.8660254037844387076, 1.000000000000000000, 0.8660254037844387076, 1.000000000000000000, 0.8660254037844387076, 1.000000000000000000, 0.8660254037844387076, 1.000000000000000000, 0.8660254037844387076, 1.000000000000000000, 0.8660254037844387076, 1.000000000000000000, 0.8660254037844387076, 1.000000000000000000, 0.8660254037844387076, 1.000000000000000000, 0.8660254037844387076, 1.000000000000000000, 0.8660254037844387076, 1.000000000000000000, 0.8660254037844387076, 1.000000000000000000, 0.8660254037844387076, 1.000000000000000000, 0.8660254037844387076, 1.000000000000000000, 0.8660254037844387076, 1.000000000000000000, 0.8660254037844387076, 1.000000000000000000, 0.8660254037844387076, 1.000000000000000000, 0.8660254037844387076, 1.000000000000000000, 0.8660254037844387076, 1.000000000000000000, 0.8660254037844387076, 1.000000000000000000, 0.8660254037844387076, 1.000000000000000000, 0.8660254037844387076, 1.000000000000000000, 0.8660254037844387076, 1.000000000000000000, 0.8660254037844387076, 1.000000000000000000, 0.8660254037844387076, 1.000000000000000000, 0.8660254037844387076, 1.000000000000000000, 0.8660254037844387076, 1.000000000000000000, 0.8660254037844387076, 1.000000000000000000, 0.8660254037844387076, 1.000000000000000000, 0.8660254037844387076, 1.000000000000000000, 0.8660254037844387076, 1.000000000000000000, 0.8660254037844387076, 1.000000000000000000, 0.8660254037844387076, 1.000000000000000000, 0.8660254037844387076, 1.000000000000000000, 0.8660254037844387076, 1.000000000000000000, 0.8660254037844387076, 1.000000000000000000, 0.8660254037844387076, 1.000000000000000000, 0.8660254037844387076, 1.000000000000000000, 0.8660254037844387076, 1.000000000000000000, 0.8660254037844387076, 1.000000000000000000, 0.8660254037844387076, 1.000000000000000000, 0.8660254037844387076, 1.000000000000000000, 0.8660254037844387076, 1.000000000000000000, 0.8660254037844387076, 1.000000000000000000, 0.8660254037844387076, 1.000000000000000000, 0.8660254037844387076, 1.000000000000000000, 0.8660254037844387076, 1.000000000000000000, 0.8660254037844387076, 1.000000000000000000, 0.8660254037844387076, 1.000000000000000000, 0.8660254037844387076, 1.000000000000000000, 0.8660254037844387076, 1.000000000000000000, 0.8660254037844387076, 1.000000000000000000, 0.8660254037844387076, 1.000000000000000000, 0.8660254037844387076, 1.000000000000000000, 0.8660254037844387076, 1.000000000000000000, 0.8660254037844387076, 1.000000000000000000, 0.8660254037844387076, 1.000000000000000000, 0.8660254037844387076, 1.000000000000000000, 0.8660254037844387076, 1.000000000000000000, 0.8660254037844387076, 1.000000000000000000, 0.8660254037844387076, 1.000000000000000000, 0.8660254037844387076, 1.000000000000000000, 0.8660254037844387076, 1.000000000000000000, 0.8660254037844387076, 1.000000000000000000, 0.8660254037844387076, 1.000000000000000000, 0.8660254037844387076, 1.000000000000000000, 0.8660254037844387076, 1.000000000000000000, 0.8660254037844387076, 1.000000000000000000, 0.8660254037844387076, 1.000000000000000000, 0.8660254037844387076, 1.000000000000000000, 0.8660254037844387076, 1.000000000000000000, 0.8660254037844387076, 1.000000000000000000, 0.8660254037844387076, 1.000000000000000000, 0.8660254037844387076, 1.000000000000000000, 0.8660254037844387076, 1.000000000000000000, 0.8660254037844387076, 1.000000000000000000, 0.8660254037844387076, 1.000000000000000000, 0.8660254037844387076, 1.000000000000000000, 0.8660254037844387076, 1.000000000000000000, 0.8660254037844387076, 1.000000000000000000, 0.8660254037844387076, 1.000000000000000000, 0.8660254037844387076, 1.000000000000000000, 0.8660254037844387076, 1.000000000000000000, 0.8660254037844387076, 1.000000000000000000, 0.8660254037844387076, 1.000000000000000000, 0.8660254037844387076, 1.000000000000000000, 0.8660254037844387076, 1.000000000000000000, 0.8660254037844387076, 1.000000000000000000, 0.8660254037844387076, 1.000000000000000000, 0.8660254037844387076, 1.000000000000000000, 0.8660254037844387076, 1.000000000000000000, 0.8660254037844387076, 1.000000000000000000, 0.8660254037844387076, 1.000000000000000000, 0.8660254037844387076, 1.000000000000000000, 0.8660254037844387076, 1.000000000000000000, 0.8660254037844387076, 1.000000000000000000, 0.8660254037844387076, 1.000000000000000000, 0.8660254037844387076, 1.000000000000000000, 0.8660254037844387076, 1.000000000000000000, 0.8660254037844387076, 1.000000000000000000, 0.8660254037844387076, 1.000000000000000000, 0.8660254037844387076, 1.000000000000000000, 0.8660254037844387076, 1.000000000000000000, 0.8660254037844387076, 1.000000000000000000, 0.8660254037844387076, 1.000000000000000000, 0.8660254037844387076, 1.000000000000000000, 0.8660254037844387076, 1.000000000000000000, 0.8660254037844387076, 1.000000000000000000, 0.8660254037844387076, 1.000000000000000000, 0.8660254037844387076, 1.000000000000000000, 0.8660254037844387076, 1.000000000000000000, 0.8660254037844387076, 1.000000000000000000, 0.8660254037844387076, 1.000000000000000000, 0.8660254037844387076, 1.000000000000000000),
 ( 1.000000000000000000, 0.8660254037844387076, 1.000000000000000000, 0.8660254037844387076, 1.000000000000000000, 0.8660254037844387076, 1.000000000000000000, 0.8660254037844387076, 1.000000000000000000, 0.8660254037844387076, 1.000000000000000000, 0.8660254037844387076, 1.000000000000000000, 0.8660254037844387076, 1.000000000000000000, 0.8660254037844387076, 1.000000000000000000, 0.8660254037844387076, 1.000000000000000000, 0.8660254037844387076, 1.000000000000000000, 0.8660254037844387076, 1.000000000000000000, 0.8660254037844387076, 1.000000000000000000, 0.8660254037844387076, 1.000000000000000000, 0.8660254037844387076, 1.000000000000000000, 0.8660254037844387076, 1.000000000000000000, 0.8660254037844387076, 1.000000000000000000, 0.8660254037844387076, 1.000000000000000000, 0.8660254037844387076, 1.000000000000000000, 0.8660254037844387076, 1.000000000000000000, 0.8660254037844387076, 1.000000000000000000, 0.8660254037844387076, 1.000000000000000000, 0.8660254037844387076, 1.000000000000000000, 0.8660254037844387076, 1.000000000000000000, 0.8660254037844387076, 1.000000000000000000, 0.8660254037844387076, 1.000000000000000000, 0.8660254037844387076, 1.000000000000000000, 0.8660254037844387076, 1.000000000000000000, 0.8660254037844387076, 1.000000000000000000, 0.8660254037844387076, 1.000000000000000000, 0.8660254037844387076, 1.000000000000000000, 0.8660254037844387076, 1.000000000000000000, 0.8660254037844387076, 1.000000000000000000, 0.8660254037844387076, 1.000000000000000000, 0.8660254037844387076, 1.000000000000000000, 0.8660254037844387076, 1.000000000000000000, 0.8660254037844387076, 1.000000000000000000, 0.8660254037844387076, 1.000000000000000000, 0.8660254037844387076, 1.000000000000000000, 0.8660254037844387076, 1.000000000000000000, 0.8660254037844387076, 1.000000000000000000, 0.8660254037844387076, 1.000000000000000000, 0.8660254037844387076, 1.000000000000000000, 0.8660254037844387076, 1.000000000000000000, 0.8660254037844387076, 1.000000000000000000, 0.8660254037844387076, 1.000000000000000000, 0.8660254037844387076, 1.000000000000000000, 0.8660254037844387076, 1.000000000000000000, 0.8660254037844387076, 1.000000000000000000, 0.8660254037844387076, 1.000000000000000000, 0.8660254037844387076, 1.000000000000000000, 0.8660254037844387076, 1.000000000000000000, 0.8660254037844387076, 1.000000000000000000, 0.8660254037844387076, 1.000000000000000000, 0.8660254037844387076, 1.000000000000000000, 0.8660254037844387076, 1.000000000000000000, 0.8660254037844387076, 1.000000000000000000, 0.8660254037844387076, 1.000000000000000000, 0.8660254037844387076, 1.000000000000000000, 0.8660254037844387076, 1.000000000000000000, 0.8660254037844387076, 1.000000000000000000, 0.8660254037844387076, 1.000000000000000000, 0.8660254037844387076, 1.000000000000000000, 0.8660254037844387076, 1.000000000000000000, 0.8660254037844387076, 1.000000000000000000, 0.8660254037844387076, 1.000000000000000000, 0.8660254037844387076, 1.000000000000000000, 0.8660254037844387076, 1.000000000000000000, 0.8660254037844387076, 1.000000000000000000, 0.8660254037844387076, 1.000000000000000000, 0.8660254037844387076, 1.000000000000000000, 0.8660254037844387076, 1.000000000000000000, 0.8660254037844387076, 1.000000000000000000, 0.8660254037844387076, 1.000000000000000000, 0.8660254037844387076, 1.000000000000000000, 0.8660254037844387076, 1.000000000000000000, 0.8660254037844387076, 1.000000000000000000, 0.8660254037844387076, 1.000000000000000000, 0.8660254037844387076, 1.000000000000000000, 0.8660254037844387076, 1.000000000000000000, 0.8660254037844387076, 1.000000000000000000, 0.8660254037844387076, 1.000000000000000000, 0.8660254037844387076, 1.000000000000000000, 0.8660254037844387076, 1.000000000000000000, 0.8660254037844387076, 1.000000000000000000, 0.8660254037844387076, 1.000000000000000000, 0.8660254037844387076, 1.000000000000000000, 0.8660254037844387076, 1.000000000000000000, 0.8660254037844387076, 1.000000000000000000, 0.8660254037844387076, 1.000000000000000000, 0.8660254037844387076, 1.000000000000000000, 0.8660254037844387076, 1.000000000000000000, 0.8660254037844387076, 1.000000000000000000, 0.8660254037844387076, 1.000000000000000000, 0.8660254037844387076, 1.000000000000000000, 0.8660254037844387076, 1.000000000000000000, 0.8660254037844387076, 1.000000000000000000, 0.8660254037844387076, 1.000000000000000000, 0.8660254037844387076, 1.000000000000000000, 0.8660254037844387076, 1.000000000000000000, 0.8660254037844387076, 1.000000000000000000, 0.8660254037844387076, 1.000000000000000000, 0.8660254037844387076, 1.000000000000000000, 0.8660254037844387076, 1.000000000000000000, 0.8660254037844387076, 1.000000000000000000, 0.8660254037844387076, 1.000000000000000000, 0.8660254037844387076, 1.000000000000000000, 0.8660254037844387076, 1.000000000000000000, 0.8660254037844387076, 1.000000000000000000, 0.8660254037844387076, 1.000000000000000000, 0.8660254037844387076, 1.000000000000000000, 0.8660254037844387076, 1.000000000000000000, 0.8660254037844387076, 1.000000000000000000, 0.8660254037844387076, 1.000000000000000000, 0.8660254037844387076, 1.000000000000000000, 0.8660254037844387076, 1.000000000000000000, 0.8660254037844387076, 1.000000000000000000, 0.8660254037844387076, 1.000000000000000000, 0.8660254037844387076, 1.000000000000000000, 0.8660254037844387076, 1.000000000000000000, 0.8660254037844387076, 1.000000000000000000, 0.8660254037844387076, 1.000000000000000000, 0.8660254037844387076, 1.000000000000000000, 0.8660254037844387076, 1.000000000000000000, 0.8660254037844387076, 1.000000000000000000, 0.8660254037844387076, 1.000000000000000000, 0.8660254037844387076, 1.000000000000000000, 0.8660254037844387076, 1.000000000000000000, 0.8660254037844387076, 1.000000000000000000, 0.8660254037844387076, 1.000000000000000000, 0.8660254037844387076, 1.000000000000000000, 0.8660254037844387076, 1.000000000000000000, 0.8660254037844387076, 1.000000000000000000, 0.8660254037844387076, 1.000000000000000000, 0.8660254037844387076, 1.000000000000000000, 0.8660254037844387076, 1.000000000000000000, 0.8660254037844387076, 1.000000000000000000, 0.8660254037844387076, 1.000000000000000000, 0.8660254037844387076, 1.000000000000000000, 0.8660254037844387076, 1.000000000000000000, 0.8660254037844387076, 1.000000000000000000, 0.8660254037844387076, 1.000000000000000000, 0.8660254037844387076, 1.000000000000000000, 0.8660254037844387076, 1.000000000000000000, 0.8660254037844387076, 1.000000000000000000, 0.8660254037844387076, 1.000000000000000000, 0.8660254037844387076, 1.000000000000000000, 0.8660254037844387076, 1.000000000000000000, 0.8660254037844387076, 1.000000000000000000, 0.8660254037844387076, 1.000000000000000000, 0.8660254037844387076, 1.000000000000000000, 0.8660254037844387076, 1.000000000000000000, 0.8660254037844387076, 1.000000000000000000, 0.8660254037844387076, 1.000000000000000000, 0.8660254037844387076, 1.000000000000000000, 0.8660254037844387076, 1.000000000000000000, 0.8660254037844387076, 1.000000000000000000, 0.8660254037844387076, 1.000000000000000000, 0.8660254037844387076, 1.000000000000000000, 0.8660254037844387076, 1.000000000000000000, 0.8660254037844387076, 1.000000000000000000, 0.8660254037844387076, 1.000000000000000000, 0.8660254037844387076, 1.000000000000000000, 0.8660254037844387076, 1.000000000000000000, 0.8660254037844387076, 1.000000000000000000, 0.8660254037844387076, 1.000000000000000000, 0.8660254037844387076, 1.000000000000000000, 0.8660254037844387076, 1.000000000000000000, 0.8660254037844387076, 1.000000000000000000, 0.8660254037844387076, 1.000000000000000000, 0.8660254037844387076, 1.000000000000000000, 0.8660254037844387076, 1.000000000000000000, 0.8660254037844387076, 1.000000000000000000, 0.8660254037844387076, 1.000000000000000000, 0.8660254037844387076, 1.000000000000000000, 0.8660254037844387076, 1.000000000000000000, 0.8660254037844387076, 1.000000000000000000, 0.8660254037844387076, 1.000000000000000000, 0.8660254037844387076, 1.000000000000000000, 0.8660254037844387076, 1.000000000000000000, 0.8660254037844387076, 1.000000000000000000, 0.8660254037844387076, 1.000000000000000000, 0.8660254037844387076, 1.000000000000000000, 0.8660254037844387076, 1.000000000000000000, 0.8660254037844387076, 1.000000000000000000, 0.8660254037844387076, 1.000000000000000000, 0.8660254037844387076, 1.000000000000000000, 0.8660254037844387076, 1.000000000000000000, 0.8660254037844387076, 1.000000000000000000, 0.8660254037844387076, 1.000000000000000000, 0.8660254037844387076, 1.000000000000000000, 0.8660254037844387076, 1.000000000000000000, 0.8660254037844387076, 1.000000000000000000, 0.8660254037844387076, 1.000000000000000000, 0.8660254037844387076, 1.000000000000000000, 0.8660254037844387076, 1.000000000000000000, 0.8660254037844387076, 1.000000000000000000, 0.8660254037844387076, 1.000000000000000000, 0.8660254037844387076, 1.000000000000000000, 0.8660254037844387076, 1.000000000000000000, 0.8660254037844387076, 1.000000000000000000, 0.8660254037844387076, 1.000000000000000000, 0.8660254037844387076, 1.000000000000000000, 0.8660254037844387076, 1.000000000000000000, 0.8660254037844387076, 1.000000000000000000, 0.8660254037844387076, 1.000000000000000000, 0.8660254037844387076, 1.000000000000000000, 0.8660254037844387076, 1.000000000000000000, 0.8660254037844387076, 1.000000000000000000, 0.8660254037844387076, 1.000000000000000000, 0.8660254037844387076, 1.000000000000000000, 0.8660254037844387076, 1.000000000000000000, 0.8660254037844387076, 1.000000000000000000, 0.8660254037844387076, 1.000000000000000000, 0.8660254037844387076, 1.000000000000000000, 0.8660254037844387076, 1.000000000000000000, 0.8660254037844387076, 1.000000000000000000, 0.8660254037844387076, 1.000000000000000000, 0.8660254037844387076, 1.000000000000000000, 0.8660254037844387076, 1.000000000000000000, 0.8660254037844387076, 1.000000000000000000, 0.8660254037844387076, 1.000000000000000000, 0.8660254037844387076, 1.000000000000000000, 0.8660254037844387076, 1.000000000000000000, 0.8660254037844387076, 1.000000000000000000, 0.8660254037844387076, 1.000000000000000000, 0.8660254037844387076, 1.000000000000000000, 0.8660254037844387076, 1.000000000000000000, 0.8660254037844387076, 1.000000000000000000, 0.8660254037844387076, 1.000000000000000000, 0.8660254037844387076, 1.000000000000000000, 0.8660254037844387076, 1.000000000000000000, 0.8660254037844387076, 1.000000000000000000, 0.8660254037844387076, 1.000000000000000000, 0.8660254037844387076, 1.000000000000000000, 0.8660254037844387076, 1.000000000000000000, 0.8660254037844387076, 1.000000000000000000, 0.8660254037844387076, 1.000000000000000000, 0.8660254037844387076, 1.000000000000000000, 0.8660254037844387076, 1.000000000000000000, 0.8660254037844387076, 1.000000000000000000, 0.8660254037844387076, 1.000000000000000000, 0.8660254037844387076, 1.000000000000000000, 0.8660254037844387076, 1.000000000000000000, 0.8660254037844387076, 1.000000000000000000, 0.8660254037844387076, 1.000000000000000000, 0.8660254037844387076, 1.000000000000000000, 0.8660254037844387076, 1.000000000000000000, 0.8660254037844387076, 1.000000000000000000, 0.8660254037844387076, 1.000000000000000000, 0.8660254037844387076, 1.000000000000000000, 0.8660254037844387076, 1.000000000000000000, 0.8660254037844387076, 1.000000000000000000, 0.8660254037844387076, 1.000000000000000000, 0.8660254037844387076, 1.000000000000000000, 0.8660254037844387076, 1.000000000000000000, 0.8660254037844387076, 1.000000000000000000, 0.8660254037844387076, 1.000000000000000000, 0.8660254037844387076, 1.000000000000000000, 0.8660254037844387076, 1.000000000000000000, 0.8660254037844387076, 1.000000000000000000, 0.8660254037844387076, 1.000000000000000000, 0.8660254037844387076, 1.000000000000000000, 0.8660254037844387076, 1.000000000000000000, 0.8660254037844387076, 1.000000000000000000, 0.8660254037844387076, 1.000000000000000000, 0.8660254037844387076, 1.000000000000000000, 0.8660254037844387076, 1.000000000000000000, 0.8660254037844387076, 1.000000000000000000, 0.8660254037844387076, 1.000000000000000000, 0.8660254037844387076, 1.000000000000000000, 0.8660254037844387076, 1.000000000000000000, 0.8660254037844387076, 1.000000000000000000, 0.8660254037844387076, 1.000000000000000000, 0.8660254037844387076, 1.000000000000000000, 0.8660254037844387076, 1.000000000000000000, 0.8660254037844387076, 1.000000000000000000, 0.8660254037844387076, 1.000000000000000000, 0.8660254037844387076, 1.000000000000000000, 0.8660254037844387076, 1.000000000000000000, 0.8660254037844387076, 1.000000000000000000, 0.8660254037844387076, 1.000000000000000000, 0.8660254037844387076, 1.000000000000000000, 0.8660254037844387076, 1.000000000000000000, 0.8660254037844387076, 1.000000000000000000, 0.8660254037844387076, 1.000000000000000000, 0.8660254037844387076, 1.000000000000000000, 0.8660254037844387076, 1.000000000000000000, 0.8660254037844387076, 1.000000000000000000, 0.8660254037844387076, 1.000000000000000000, 0.8660254037844387076, 1.000000000000000000, 0.8660254037844387076, 1.000000000000000000, 0.8660254037844387076, 1.000000000000000000, 0.8660254037844387076, 1.000000000000000000, 0.8660254037844387076, 1.000000000000000000, 0.8660254037844387076, 1.000000000000000000, 0.8660254037844387076, 1.000000000000000000, 0.8660254037844387076, 1.000000000000000000, 0.8660254037844387076, 1.000000000000000000, 0.8660254037844387076, 1.000000000000000000, 0.8660254037844387076, 1.000000000000000000, 0.8660254037844387076, 1.000000000000000000, 0.8660254037844387076, 1.000000000000000000, 0.8660254037844387076, 1.000000000000000000, 0.8660254037844387076, 1.000000000000000000, 0.8660254037844387076, 1.000000000000000000, 0.8660254037844387076, 1.000000000000000000, 0.8660254037844387076, 1.000000000000000000, 0.8660254037844387076, 1.000000000000000000, 0.8660254037844387076, 1.000000000000000000, 0.8660254037844387076, 1.000000000000000000, 0.8660254037844387076, 1.000000000000000000, 0.8660254037844387076, 1.000000000000000000, 0.8660254037844387076, 1.000000000000000000, 0.8660254037844387076, 1.000000000000000000, 0.8660254037844387076, 1.000000000000000000, 0.8660254037844387076, 1.000000000000000000, 0.8660254037844387076, 1.000000000000000000, 0.8660254037844387076, 1.000000000000000000, 0.8660254037844387076, 1.000000000000000000, 0.8660254037844387076, 1.000000000000000000, 0.8660254037844387076, 1.000000000000000000, 0.8660254037844387076, 1.000000000000000000, 0.8660254037844387076, 1.000000000000000000, 0.8660254037844387076, 1.000000000000000000, 0.8660254037844387076, 1.000000000000000000, 0.8660254037844387076, 1.000000000000000000, 0.8660254037844387076, 1.000000000000000000, 0.8660254037844387076, 1.000000000000000000, 0.8660254037844387076, 1.000000000000000000, 0.8660254037844387076, 1.000000000000000000, 0.8660254037844387076, 1.000000000000000000, 0.8660254037844387076, 1.000000000000000000, 0.8660254037844387076, 1.000000000000000000, 0.8660254037844387076, 1.000000000000000000, 0.8660254037844387076, 1.000000000000000000, 0.8660254037844387076, 1.000000000000000000, 0.8660254037844387076, 1.000000000000000000, 0.8660254037844387076, 1.000000000000000000, 0.8660254037844387076, 1.000000000000000000, 0.8660254037844387076, 1.000000000000000000, 0.8660254037844387076, 1.000000000000000000, 0.8660254037844387076, 1.000000000000000000, 0.8660254037844387076, 1.000000000000000000, 0.8660254037844387076, 1.000000000000000000, 0.8660254037844387076, 1.000000000000000000, 0.8660254037844387076, 1.000000000000000000, 0.8660254037844387076, 1.000000000000000000, 0.8660254037844387076, 1.000000000000000000, 0.8660254037844387076, 1.000000000000000000, 0.8660254037844387076, 1.000000000000000000, 0.8660254037844387076, 1.000000000000000000, 0.8660254037844387076, 1.000000000000000000, 0.8660254037844387076, 1.000000000000000000, 0.8660254037844387076, 1.000000000000000000, 0.8660254037844387076, 1.000000000000000000, 0.8660254037844387076, 1.000000000000000000, 0.8660254037844387076, 1.000000000000000000, 0.8660254037844387076, 1.000000000000000000, 0.8660254037844387076, 1.000000000000000000, 0.8660254037844387076, 1.000000000000000000) ) ) 
 REPRESENTATION_ITEM ( '' )  SURFACE ( )  );
#47364 = CARTESIAN_POINT ( 'NONE',  ( 16.05937500061451573, -4.541064518000417216, -2.621784821875001281 ) ) ;
#47365 = CARTESIAN_POINT ( 'NONE',  ( 22.11562500061451786, 3.027376345333611329, 5.243569643749999010 ) ) ;
#47366 = CARTESIAN_POINT ( 'NONE',  ( -3.999999999999999112, 15.05000000000000071, 30.00000000000000000 ) ) ;
#47367 = CARTESIAN_POINT ( 'NONE',  ( 3.271875000614519635, 3.027376345333611329, 5.243569643749999010 ) ) ;
#47368 = CARTESIAN_POINT ( 'NONE',  ( 9.075000001229033941, -5.773502691896255534, -1.060575238724906372E-15 ) ) ;
#47369 = ORIENTED_EDGE ( 'NONE', *, *, #16702, .T. ) ;
#47370 = CARTESIAN_POINT ( 'NONE',  ( 5.175000001229033586, 2.886751345948129099, -4.999999999999998224 ) ) ;
#47371 = CARTESIAN_POINT ( 'NONE',  ( 1.999999999999998668, 18.95000000000000284, -33.46410161513775705 ) ) ;
#47372 = CARTESIAN_POINT ( 'NONE',  ( 25.31250000122903288, -4.330127018922190985, -2.500000000000001332 ) ) ;
#47373 = CARTESIAN_POINT ( 'NONE',  ( 1.878215178124997609, 13.12812499938548427, 33.25316411605952993 ) ) ;
#47374 = CARTESIAN_POINT ( 'NONE',  ( 8.146875000614516082, 6.054752690667223547, 3.707466751127219781E-16 ) ) ;
#47375 = DIRECTION ( 'NONE',  ( -1.000000000000000000, -0.000000000000000000, -0.000000000000000000 ) ) ;
#47376 = EDGE_CURVE ( 'NONE', #33433, #37978, #28836, .T. ) ;
#47377 = CARTESIAN_POINT ( 'NONE',  ( 13.90312500061451750, 4.541064518000418104, -2.621784821874998173 ) ) ;
#47378 = CARTESIAN_POINT ( 'NONE',  ( 10.95937500061451964, 0.000000000000000000, 5.243569643749999010 ) ) ;
#47379 = CARTESIAN_POINT ( 'NONE',  ( 26.85000000122903430, 5.773502691896255534, 3.535250795749688894E-16 ) ) ;
#47380 = CARTESIAN_POINT ( 'NONE',  ( 17.07187500061451502, 3.027376345333612662, -5.243569643749998122 ) ) ;
#47381 = CARTESIAN_POINT ( 'NONE',  ( 6.009375000614519458, 0.000000000000000000, 5.243569643749999010 ) ) ;
#47382 = CARTESIAN_POINT ( 'NONE',  ( 1.626862140677534273E-15, 16.17500000122903359, 34.00000000000000000 ) ) ;
#47383 = CARTESIAN_POINT ( 'NONE',  ( 6.778125000614518392, 4.541064518000418104, 2.621784821874999949 ) ) ;
#47384 = CARTESIAN_POINT ( 'NONE',  ( 17.69062500061451715, -3.027376345333614438, 5.243569643749998122 ) ) ;
#47385 = ORIENTED_EDGE ( 'NONE', *, *, #1622, .F. ) ;
#47386 = CARTESIAN_POINT ( 'NONE',  ( 14.57812500061451644, -4.541064518000419881, 2.621784821874995952 ) ) ;
#47387 = CARTESIAN_POINT ( 'NONE',  ( 10.56562500061451715, -6.054752690667223547, -1.112240025338166033E-15 ) ) ;
#47388 = CARTESIAN_POINT ( 'NONE',  ( 22.43437500061451573, 5.824947211148865298E-16, -4.756430356249998326 ) ) ;
#47389 = CARTESIAN_POINT ( 'NONE',  ( 12.15000000000000036, -4.330127018922190985, -2.500000000000001332 ) ) ;
#47390 = CARTESIAN_POINT ( 'NONE',  ( 6.075000001229034829, 2.886751345948129099, -4.999999999999998224 ) ) ;
#47391 = EDGE_CURVE ( 'NONE', #13783, #43576, #5764, .T. ) ;
#47392 = CARTESIAN_POINT ( 'NONE',  ( 13.77187500061451786, -6.054752690667223547, -1.112240025338166033E-15 ) ) ;
#47393 = CARTESIAN_POINT ( 'NONE',  ( 15.78750000122903430, -4.330127018922194537, 2.499999999999995559 ) ) ;
#47394 = CARTESIAN_POINT ( 'NONE',  ( 23.81250000000000000, -5.773502691896255534, -1.060575238724906372E-15 ) ) ;
#47395 = CARTESIAN_POINT ( 'NONE',  ( -2.121784821874996840, 18.97812500061451857, -26.32496088578401583 ) ) ;
#47396 = CARTESIAN_POINT ( 'NONE',  ( -3.999999999999999112, 16.02500000122903501, 27.69059892324149885 ) ) ;
#47397 = FACE_OUTER_BOUND ( 'NONE', #23664, .T. ) ;
#47398 = CARTESIAN_POINT ( 'NONE',  ( 7.106250001229032165, 0.000000000000000000, 4.999999999999998224 ) ) ;
#47399 = CARTESIAN_POINT ( 'NONE',  ( 18.76875000122903003, 2.886751345948098901, 5.000000000000047073 ) ) ;
#47400 = CARTESIAN_POINT ( 'NONE',  ( 15.30937500061451750, 4.541064518000418104, -2.621784821874998173 ) ) ;
#47401 = AXIS2_PLACEMENT_3D ( 'NONE', #19728, #26759, #43010 ) ;
#47402 = CARTESIAN_POINT ( 'NONE',  ( 28.64999999999999858, 0.000000000000000000, 4.999999999999998224 ) ) ;
#47403 = CARTESIAN_POINT ( 'NONE',  ( 13.04062500061451502, 6.054752690667223547, 3.707466751127219781E-16 ) ) ;
#47404 = VECTOR ( 'NONE', #69998, 1000.000000000000000 ) ;
#47405 = CARTESIAN_POINT ( 'NONE',  ( 29.70937500061451431, 2.746126346562643317, 4.756430356249998326 ) ) ;
#47406 = CARTESIAN_POINT ( 'NONE',  ( 24.30937500061451573, 4.541064518000418104, -2.621784821874998173 ) ) ;
#47407 = CARTESIAN_POINT ( 'NONE',  ( 16.24687500061451573, 0.000000000000000000, 4.756430356249998326 ) ) ;
#47408 = CARTESIAN_POINT ( 'NONE',  ( 10.67812500061451608, 6.421520780324663323E-16, -5.243569643749999010 ) ) ;
#47409 = CARTESIAN_POINT ( 'NONE',  ( 15.98437500061451821, -4.541064518000419881, 2.621784821874995952 ) ) ;
#47410 = ORIENTED_EDGE ( 'NONE', *, *, #8310, .T. ) ;
#47411 = CARTESIAN_POINT ( 'NONE',  ( 26.74687500061451573, -3.027376345333614438, 5.243569643749998122 ) ) ;
#47412 = CARTESIAN_POINT ( 'NONE',  ( 27.62812500061451360, -4.541064518000419881, 2.621784821874995952 ) ) ;
#47413 = CARTESIAN_POINT ( 'NONE',  ( 17.42812500061451786, 6.421520780324663323E-16, -5.243569643749999010 ) ) ;
#47414 = CARTESIAN_POINT ( 'NONE',  ( 1.626862140677534273E-15, 13.02500000122903323, -26.00000000000000355 ) ) ;
#47415 = CARTESIAN_POINT ( 'NONE',  ( -1.487416814333745711E-14, 14.82500000122903572, -26.00000000000000000 ) ) ;
#47416 = CARTESIAN_POINT ( 'NONE',  ( 8.025000000000000355, -4.330127018922194537, 2.499999999999995559 ) ) ;
#47417 = CARTESIAN_POINT ( 'NONE',  ( 20.06250000122903643, 4.330127018922192761, -2.499999999999997780 ) ) ;
#47418 = CARTESIAN_POINT ( 'NONE',  ( 4.898587196589412829E-16, 27.50000000000000000, 34.00000000000000000 ) ) ;
#47419 = CARTESIAN_POINT ( 'NONE',  ( 11.63437500061451502, 5.492252693125287522, 3.363034840372157021E-16 ) ) ;
#47420 = VERTEX_POINT ( 'NONE', #34923 ) ;
#47421 = CARTESIAN_POINT ( 'NONE',  ( 16.61250000000000426, -5.773502691896255534, -1.060575238724906372E-15 ) ) ;
#47422 = CARTESIAN_POINT ( 'NONE',  ( 18.93750000000000000, -2.886751345948125991, -5.000000000000000000 ) ) ;
#47423 = CARTESIAN_POINT ( 'NONE',  ( 19.24687500061452283, -3.027376345333610441, -5.243569643749999898 ) ) ;
#47424 = CARTESIAN_POINT ( 'NONE',  ( 14.09062500061451750, -3.027376345333614438, 5.243569643749998122 ) ) ;
#47425 = ORIENTED_EDGE ( 'NONE', *, *, #40932, .F. ) ;
#47426 = CARTESIAN_POINT ( 'NONE',  ( 5.728125000614515905, 6.421520780324663323E-16, -5.243569643749999010 ) ) ;
#47427 = CARTESIAN_POINT ( 'NONE',  ( 0.000000000000000000, 10.00000000000000000, 0.000000000000000000 ) ) ;
#47428 = CARTESIAN_POINT ( 'NONE',  ( 12.00000000000000000, 0.000000000000000000, 4.999999999999998224 ) ) ;
#47429 = CARTESIAN_POINT ( 'NONE',  ( 27.45937500061451431, 2.746126346562643317, 4.756430356249998326 ) ) ;
#47430 = CARTESIAN_POINT ( 'NONE',  ( -3.000416591977282496E-16, 14.74062500061451786, 25.09994784771203058 ) ) ;
#47431 = CARTESIAN_POINT ( 'NONE',  ( 26.09062500061451573, 6.054752690667223547, 3.707466751127219781E-16 ) ) ;
#47432 = CARTESIAN_POINT ( 'NONE',  ( 8.025000000000000355, -4.330127018922194537, 2.499999999999995559 ) ) ;
#47433 = CARTESIAN_POINT ( 'NONE',  ( 2.655984681222220721E-16, 18.60312499938548214, 25.66244784525396483 ) ) ;
#47434 = CARTESIAN_POINT ( 'NONE',  ( 24.27187500061452141, 3.027376345333613106, -5.243569643749998122 ) ) ;
#47435 = ORIENTED_EDGE ( 'NONE', *, *, #1622, .T. ) ;
#47436 = CARTESIAN_POINT ( 'NONE',  ( 22.04062500061451502, 6.054752690667223547, 3.707466751127219781E-16 ) ) ;
#47437 = CARTESIAN_POINT ( 'NONE',  ( 22.32187500061451502, -6.054752690667223547, -1.112240025338166033E-15 ) ) ;
#47438 = CARTESIAN_POINT ( 'NONE',  ( -4.243569643749998122, 16.24062500061459247, -27.54997392385601174 ) ) ;
#47439 = CARTESIAN_POINT ( 'NONE',  ( 7.378125000614518036, -4.541064518000419881, 2.621784821874995952 ) ) ;
#47440 = CARTESIAN_POINT ( 'NONE',  ( 27.34687500061451360, -2.746126346562641984, -4.756430356249999214 ) ) ;
#47441 = CARTESIAN_POINT ( 'NONE',  ( 24.06562500061451715, -6.054752690667223547, -1.112240025338166033E-15 ) ) ;
#47442 = CARTESIAN_POINT ( 'NONE',  ( 9.609375000614518214, 0.000000000000000000, 4.756430356249998326 ) ) ;
#47443 = CARTESIAN_POINT ( 'NONE',  ( 3.756430356249998770, 17.10312499938548214, 32.16877607737302469 ) ) ;
#47444 = CARTESIAN_POINT ( 'NONE',  ( 17.67187500061451644, 3.027376345333611329, 5.243569643749999010 ) ) ;
#47445 = CARTESIAN_POINT ( 'NONE',  ( 24.60937500061451644, -4.541064518000417216, -2.621784821875001281 ) ) ;
#47446 = CARTESIAN_POINT ( 'NONE',  ( -3.000416591977282496E-16, 14.79687500061451821, 25.09994784771203058 ) ) ;
#47447 = CARTESIAN_POINT ( 'NONE',  ( 8.278125000614515727, -4.541064518000419881, 2.621784821874995952 ) ) ;
#47448 = CARTESIAN_POINT ( 'NONE',  ( 27.96562500061451928, 3.027376345333611329, 5.243569643749999010 ) ) ;
#47449 = CARTESIAN_POINT ( 'NONE',  ( 29.27812500061451573, 4.541064518000418104, 2.621784821874999949 ) ) ;
#47450 = LINE ( 'NONE', #30094, #1809 ) ;
#47451 = CARTESIAN_POINT ( 'NONE',  ( 5.015625000614518214, 3.027376345333611329, 5.243569643749999010 ) ) ;
#47452 = CARTESIAN_POINT ( 'NONE',  ( 9.346875000614517148, -3.027376345333610441, -5.243569643749999898 ) ) ;
#47453 = CARTESIAN_POINT ( 'NONE',  ( 15.67500000122903181, 2.886751345948126879, 4.999999999999999112 ) ) ;
#47454 = CARTESIAN_POINT ( 'NONE',  ( 29.05312500061451431, -4.541064518000417216, -2.621784821875001281 ) ) ;
#47455 = CARTESIAN_POINT ( 'NONE',  ( 5.840625000614516615, 6.054752690667223547, 3.707466751127219781E-16 ) ) ;
#47456 = CARTESIAN_POINT ( 'NONE',  ( -1.999999999999999112, 13.94374999877096677, 26.53589838486224650 ) ) ;
#47457 = CARTESIAN_POINT ( 'NONE',  ( 21.61875000122903145, -5.773502691896255534, -1.060575238724906372E-15 ) ) ;
#47458 = CARTESIAN_POINT ( 'NONE',  ( 16.65937500061452070, 4.541064518000418104, -2.621784821874998173 ) ) ;
#47459 = CARTESIAN_POINT ( 'NONE',  ( 0.000000000000000000, 20.00000000000000000, 30.00000000000000000 ) ) ;
#47460 = ORIENTED_EDGE ( 'NONE', *, *, #5433, .F. ) ;
#47461 = CARTESIAN_POINT ( 'NONE',  ( 21.14062500061451289, 6.054752690667223547, 3.707466751127219781E-16 ) ) ;
#47462 = CARTESIAN_POINT ( 'NONE',  ( 9.065625000614517148, 3.027376345333611329, 5.243569643749999010 ) ) ;
#47463 = CARTESIAN_POINT ( 'NONE',  ( 23.82187500061451502, 3.027376345333612662, -5.243569643749998122 ) ) ;
#47464 = CARTESIAN_POINT ( 'NONE',  ( 7.753125000614518036, 0.000000000000000000, 5.243569643749999010 ) ) ;
#47465 = CARTESIAN_POINT ( 'NONE',  ( 20.32499999999999929, 6.123233995736764310E-16, -4.999999999999998224 ) ) ;
#47466 = CARTESIAN_POINT ( 'NONE',  ( 11.02500000122903501, 2.886751345948129099, -4.999999999999998224 ) ) ;
#47467 = CARTESIAN_POINT ( 'NONE',  ( 23.80312500061451786, 4.541064518000418104, -2.621784821874998173 ) ) ;
#47468 = AXIS2_PLACEMENT_3D ( 'NONE', #3758, #59886, #25168 ) ;
#47469 = CARTESIAN_POINT ( 'NONE',  ( 4.243569643749999898, 11.02812500061451750, -30.00000000000000000 ) ) ;
#47470 = CARTESIAN_POINT ( 'NONE',  ( 13.46250000122903323, 0.000000000000000000, 4.999999999999998224 ) ) ;
#47471 = CARTESIAN_POINT ( 'NONE',  ( 22.52812500061451573, 4.541064518000418104, 2.621784821874999949 ) ) ;
#47472 = CARTESIAN_POINT ( 'NONE',  ( 17.27812500061451217, -4.541064518000419881, 2.621784821874995952 ) ) ;
#47473 = CARTESIAN_POINT ( 'NONE',  ( 5.221875000614519813, -6.054752690667223547, -1.112240025338166033E-15 ) ) ;
#47474 = CARTESIAN_POINT ( 'NONE',  ( 18.82500000000000284, -4.330127018922194537, 2.499999999999995559 ) ) ;
#47475 = EDGE_CURVE ( 'NONE', #17152, #27917, #69634, .T. ) ;
#47476 = CARTESIAN_POINT ( 'NONE',  ( 13.61250000122903359, -4.330127018922190985, -2.500000000000001332 ) ) ;
#47477 = CARTESIAN_POINT ( 'NONE',  ( 11.05312500061451608, -4.541064518000417216, -2.621784821875001281 ) ) ;
#47478 = CARTESIAN_POINT ( 'NONE',  ( 12.96562500061451750, 3.027376345333613106, -5.243569643749998122 ) ) ;
#47479 = CARTESIAN_POINT ( 'NONE',  ( 24.37500000122903288, -5.773502691896255534, -1.060575238724906372E-15 ) ) ;
#47480 = CARTESIAN_POINT ( 'NONE',  ( 21.87187500061451573, -6.054752690667223547, -1.112240025338166033E-15 ) ) ;
#47481 = CARTESIAN_POINT ( 'NONE',  ( 21.04687500061451644, -3.027376345333610441, -5.243569643749999898 ) ) ;
#47482 = CARTESIAN_POINT ( 'NONE',  ( 30.00000000000000000, 0.000000000000000000, 0.000000000000000000 ) ) ;
#47483 = EDGE_CURVE ( 'NONE', #34653, #16314, #33144, .T. ) ;
#47484 = CARTESIAN_POINT ( 'NONE',  ( 8.475000001229034297, 2.886751345948126879, 4.999999999999999112 ) ) ;
#47485 = CARTESIAN_POINT ( 'NONE',  ( 6.346875000614517148, 6.054752690667223547, 3.707466751127219781E-16 ) ) ;
#47486 = CARTESIAN_POINT ( 'NONE',  ( 24.90937500061451715, 0.000000000000000000, 5.243569643749999010 ) ) ;
#47487 = ADVANCED_FACE ( 'NONE', ( #40844 ), #13104, .F. ) ;
#47488 = CARTESIAN_POINT ( 'NONE',  ( 4.286481933758009788, -2.574115893188666959, -4.460274119859103159 ) ) ;
#47489 = CARTESIAN_POINT ( 'NONE',  ( 22.19062500061451715, -3.027376345333614438, 5.243569643749998122 ) ) ;
#47490 = CARTESIAN_POINT ( 'NONE',  ( 26.22187500061451715, 3.027376345333611329, 5.243569643749999010 ) ) ;
#47491 = CARTESIAN_POINT ( 'NONE',  ( -7.967954043666661671E-16, 17.59062499938548285, 34.33755215474603517 ) ) ;
#47492 = CARTESIAN_POINT ( 'NONE',  ( -5.810221930991193690E-16, 15.83749999999999680, 26.00000000000000355 ) ) ;
#47493 = CARTESIAN_POINT ( 'NONE',  ( 6.646875000614518747, -3.027376345333610441, -5.243569643749999898 ) ) ;
#47494 = CARTESIAN_POINT ( 'NONE',  ( 16.71562500061451573, 3.027376345333611329, 5.243569643749999010 ) ) ;
#47495 = ORIENTED_EDGE ( 'NONE', *, *, #37141, .F. ) ;
#47496 = CARTESIAN_POINT ( 'NONE',  ( 22.91250000000000142, -5.773502691896255534, -1.060575238724906372E-15 ) ) ;
#47497 = CARTESIAN_POINT ( 'NONE',  ( 25.82812500061451644, -4.541064518000419881, 2.621784821874995952 ) ) ;
#47498 = CARTESIAN_POINT ( 'NONE',  ( 3.646875000614520079, 6.054752690667223547, 3.707466751127219781E-16 ) ) ;
#47499 = CARTESIAN_POINT ( 'NONE',  ( 10.27500000122903145, 2.886751345948193936, 4.999999999999883649 ) ) ;
#47500 = CARTESIAN_POINT ( 'NONE',  ( 3.675409193445907441, 3.389947486076141381, -3.797828392354649640 ) ) ;
#47501 = CARTESIAN_POINT ( 'NONE',  ( 16.38749999999999929, 5.773502691896255534, 3.535250795749688894E-16 ) ) ;
#47502 = CARTESIAN_POINT ( 'NONE',  ( 19.94062500061451715, -3.027376345333614438, 5.243569643749998122 ) ) ;
#47503 = ORIENTED_EDGE ( 'NONE', *, *, #31085, .T. ) ;
#47504 = CARTESIAN_POINT ( 'NONE',  ( 25.23749999999999716, -2.886751345948125991, -5.000000000000000000 ) ) ;
#47505 =( BOUNDED_CURVE ( )  B_SPLINE_CURVE ( 2, ( #70477, #37585, #48315, #54581, #25406, #71203, #9877 ),
 .UNSPECIFIED., .F., .F. ) 
 B_SPLINE_CURVE_WITH_KNOTS ( ( 3, 2, 2, 3 ),
 ( 0.1300000000000000322, 0.1333333333333333592, 0.1366666666666666585, 0.1400000000000000133 ),
 .UNSPECIFIED. ) 
 CURVE ( )  GEOMETRIC_REPRESENTATION_ITEM ( )  RATIONAL_B_SPLINE_CURVE ( ( 0.9999999999999988898, 0.8660254037844398178, 1.000000000000000000, 0.8660254037844387076, 1.000000000000000000, 0.8660254037844387076, 1.000000000000000000 ) ) 
 REPRESENTATION_ITEM ( '' )  );
#47506 = CARTESIAN_POINT ( 'NONE',  ( 26.93437500061451573, 6.421520780324663323E-16, -5.243569643749999010 ) ) ;
#47507 = ORIENTED_EDGE ( 'NONE', *, *, #6118, .T. ) ;
#47508 =( GEOMETRIC_REPRESENTATION_CONTEXT ( 3 ) GLOBAL_UNCERTAINTY_ASSIGNED_CONTEXT ( ( #35121 ) ) GLOBAL_UNIT_ASSIGNED_CONTEXT ( ( #24909, #47095, #13829 ) ) REPRESENTATION_CONTEXT ( 'NONE', 'WORKASPACE' ) );
#47509 = CARTESIAN_POINT ( 'NONE',  ( 2.989682168262277173, -4.007725729151955463, -3.381303433842018258 ) ) ;
#47510 = CARTESIAN_POINT ( 'NONE',  ( 12.96562500061451750, 3.027376345333613106, -5.243569643749998122 ) ) ;
#47511 = CARTESIAN_POINT ( 'NONE',  ( 6.665625000614515905, 3.027376345333613106, -5.243569643749998122 ) ) ;
#47512 = CARTESIAN_POINT ( 'NONE',  ( 16.69687500061451502, 0.000000000000000000, 4.756430356249998326 ) ) ;
#47513 = CARTESIAN_POINT ( 'NONE',  ( 2.896875000614518747, -3.027376345333614438, 5.243569643749998122 ) ) ;
#47514 = CARTESIAN_POINT ( 'NONE',  ( 14.73750000122903359, 4.330127018922191873, 2.499999999999999556 ) ) ;
#47515 = CARTESIAN_POINT ( 'NONE',  ( 19.38749999999999929, -2.886751345948125991, -5.000000000000000000 ) ) ;
#47516 = CARTESIAN_POINT ( 'NONE',  ( 27.52500000000000213, 6.123233995736764310E-16, -4.999999999999998224 ) ) ;
#47517 = LINE ( 'NONE', #64867, #61589 ) ;
#47518 = CARTESIAN_POINT ( 'NONE',  ( 8.409375000614518925, -4.541064518000417216, -2.621784821875001281 ) ) ;
#47519 = CARTESIAN_POINT ( 'NONE',  ( 18.68437500061451928, -4.541064518000419881, 2.621784821874995952 ) ) ;
#47520 = CARTESIAN_POINT ( 'NONE',  ( 26.06250000000000000, -5.773502691896255534, -1.060575238724906372E-15 ) ) ;
#47521 = ORIENTED_EDGE ( 'NONE', *, *, #36932, .T. ) ;
#47522 = CARTESIAN_POINT ( 'NONE',  ( 27.89062500061451289, 6.054752690667223547, 3.707466751127219781E-16 ) ) ;
#47523 = CARTESIAN_POINT ( 'NONE',  ( 3.787500000000002753, 5.773502691896255534, 3.535250795749688894E-16 ) ) ;
#47524 = CARTESIAN_POINT ( 'NONE',  ( 4.246875000614519280, -3.027376345333614438, 5.243569643749998122 ) ) ;
#47525 = CARTESIAN_POINT ( 'NONE',  ( 15.45000000000000107, 4.330127018922192761, -2.499999999999997780 ) ) ;
#47526 = CARTESIAN_POINT ( 'NONE',  ( 14.69062500061451537, -3.027376345333610441, -5.243569643749999898 ) ) ;
#47527 = CARTESIAN_POINT ( 'NONE',  ( 45.00000000000000000, -2.499999999999999556, -3.499999999999999556 ) ) ;
#47528 = CARTESIAN_POINT ( 'NONE',  ( 45.00000000000000000, 0.000000000000000000, 4.999999999999998224 ) ) ;
#47529 = CARTESIAN_POINT ( 'NONE',  ( 13.46250000122903323, 0.000000000000000000, 4.999999999999998224 ) ) ;
#47530 = CARTESIAN_POINT ( 'NONE',  ( 17.92500000122903359, 2.886751345948126879, 4.999999999999999112 ) ) ;
#47531 = CARTESIAN_POINT ( 'NONE',  ( -1.071796769724488563, 13.45490381179670081, 34.00000000000000000 ) ) ;
#47532 = CARTESIAN_POINT ( 'NONE',  ( 18.00937500061451502, 4.119189519843966529, -2.378215178124998275 ) ) ;
#47533 = CARTESIAN_POINT ( 'NONE',  ( 8.690625000614515372, -3.027376345333614438, 5.243569643749998122 ) ) ;
#47534 = CARTESIAN_POINT ( 'NONE',  ( 24.57187500061451502, -6.054752690667223547, -1.112240025338166033E-15 ) ) ;
#47535 = FACE_OUTER_BOUND ( 'NONE', #25330, .T. ) ;
#47536 = CARTESIAN_POINT ( 'NONE',  ( 22.92187500061451644, 3.027376345333613106, -5.243569643749998122 ) ) ;
#47537 = CARTESIAN_POINT ( 'NONE',  ( 5.475000000000000533, 6.123233995736764310E-16, -4.999999999999998224 ) ) ;
#47538 = CARTESIAN_POINT ( 'NONE',  ( 8.484601909799253346E-16, 11.22500000122903607, 34.61880215351700230 ) ) ;
#47539 = CARTESIAN_POINT ( 'NONE',  ( 14.65312500061451573, -4.541064518000417216, -2.621784821875001281 ) ) ;
#47540 = CARTESIAN_POINT ( 'NONE',  ( 5.625000001229036428, 2.886751345948129099, -4.999999999999998224 ) ) ;
#47541 = CARTESIAN_POINT ( 'NONE',  ( 9.871875000614517504, 3.027376345333613106, -5.243569643749998122 ) ) ;
#47542 = CARTESIAN_POINT ( 'NONE',  ( 1.999999999999998668, 15.01250000122903394, 26.53589838486224650 ) ) ;
#47543 = ORIENTED_EDGE ( 'NONE', *, *, #27431, .F. ) ;
#47544 = CARTESIAN_POINT ( 'NONE',  ( 12.32812500061451821, -4.541064518000419881, 2.621784821874995952 ) ) ;
#47545 = CARTESIAN_POINT ( 'NONE',  ( 24.30000000122903359, -2.886751345948129988, 4.999999999999997335 ) ) ;
#47546 = CARTESIAN_POINT ( 'NONE',  ( 10.77187500061451786, 3.027376345333613106, -5.243569643749998122 ) ) ;
#47547 = CARTESIAN_POINT ( 'NONE',  ( 13.97812500061451679, 4.541064518000418104, 2.621784821874999949 ) ) ;
#47548 = CARTESIAN_POINT ( 'NONE',  ( 28.89375000122903003, -2.886751345948125991, -5.000000000000000000 ) ) ;
#47549 = CARTESIAN_POINT ( 'NONE',  ( 24.72187500061451360, 3.027376345333613106, -5.243569643749998122 ) ) ;
#47550 = CARTESIAN_POINT ( 'NONE',  ( 8.625000000000000000, 6.123233995736764310E-16, -4.999999999999998224 ) ) ;
#47551 = DIRECTION ( 'NONE',  ( 0.000000000000000000, 0.000000000000000000, 1.000000000000000000 ) ) ;
#47552 = CARTESIAN_POINT ( 'NONE',  ( 20.51250000122903216, 4.330127018922192761, -2.499999999999997780 ) ) ;
#47553 = CARTESIAN_POINT ( 'NONE',  ( 4.243569643749999010, 14.27187500061451786, -32.45002607614398471 ) ) ;
#47554 = CARTESIAN_POINT ( 'NONE',  ( 15.45937500061451608, 0.000000000000000000, 5.243569643749999010 ) ) ;
#47555 = CARTESIAN_POINT ( 'NONE',  ( 17.13750000122903216, -4.330127018922194537, 2.499999999999995559 ) ) ;
#47556 = CARTESIAN_POINT ( 'NONE',  ( 12.45937500061451786, -4.541064518000417216, -2.621784821875001281 ) ) ;
#47557 = CARTESIAN_POINT ( 'NONE',  ( -2.121784821874999949, 17.92812500061451786, -33.67503911421598417 ) ) ;
#47558 = CARTESIAN_POINT ( 'NONE',  ( 20.66250000122903074, 0.000000000000000000, 4.999999999999998224 ) ) ;
#47559 = CARTESIAN_POINT ( 'NONE',  ( 12.02812500061451573, 6.421520780324663323E-16, -5.243569643749999010 ) ) ;
#47560 = VERTEX_POINT ( 'NONE', #30104 ) ;
#47561 = ORIENTED_EDGE ( 'NONE', *, *, #48761, .T. ) ;
#47562 = CARTESIAN_POINT ( 'NONE',  ( 15.71250000000000213, -5.773502691896255534, -1.060575238724906372E-15 ) ) ;
#47563 = FACE_OUTER_BOUND ( 'NONE', #39204, .T. ) ;
#47564 = CARTESIAN_POINT ( 'NONE',  ( 13.39687500061451608, -3.027376345333610441, -5.243569643749999898 ) ) ;
#47565 = CARTESIAN_POINT ( 'NONE',  ( 65.00000000000000000, 0.000000000000000000, 0.000000000000000000 ) ) ;
#47566 = CARTESIAN_POINT ( 'NONE',  ( 12.71250000122903145, -4.330127018922190985, -2.500000000000001332 ) ) ;
#47567 = CARTESIAN_POINT ( 'NONE',  ( 20.32500000122903572, -5.773502691896255534, -1.060575238724906372E-15 ) ) ;
#47568 = CARTESIAN_POINT ( 'NONE',  ( 17.76562500061451644, -6.054752690667223547, -1.112240025338166033E-15 ) ) ;
#47569 = CARTESIAN_POINT ( 'NONE',  ( 20.80312500061451431, 0.000000000000000000, 5.243569643749999010 ) ) ;
#47570 = CARTESIAN_POINT ( 'NONE',  ( 28.46250000122903145, -4.330127018922190985, -2.500000000000001332 ) ) ;
#47571 =( BOUNDED_CURVE ( )  B_SPLINE_CURVE ( 2, ( #15975, #61048, #38147, #10446, #66974, #38894, #62141 ),
 .UNSPECIFIED., .F., .F. ) 
 B_SPLINE_CURVE_WITH_KNOTS ( ( 3, 2, 2, 3 ),
 ( 0.03333333333333339532, 0.03611111111111116323, 0.03888888888888894502, 0.04166666666666671293 ),
 .UNSPECIFIED. ) 
 CURVE ( )  GEOMETRIC_REPRESENTATION_ITEM ( )  RATIONAL_B_SPLINE_CURVE ( ( 0.9999999999999968914, 0.8660254037844417052, 1.000000000000000000, 0.8660254037844387076, 1.000000000000000000, 0.8660254037844363761, 1.000000000000002442 ) ) 
 REPRESENTATION_ITEM ( '' )  );
#47572 = CARTESIAN_POINT ( 'NONE',  ( 28.19999999999999929, 0.000000000000000000, 4.999999999999998224 ) ) ;
#47573 = CARTESIAN_POINT ( 'NONE',  ( 10.00000000000000000, 1.224646799147353256E-15, 10.00000000000000178 ) ) ;
#47574 = CARTESIAN_POINT ( 'NONE',  ( 29.36250000000000071, 2.886751345948129099, -4.999999999999998224 ) ) ;
#47575 = CARTESIAN_POINT ( 'NONE',  ( 27.00937500061451857, 4.541064518000418104, -2.621784821874998173 ) ) ;
#47576 = CARTESIAN_POINT ( 'NONE',  ( -0.6945863667395647534, 9.663023495605401081, -33.93923213064925903 ) ) ;
#47577 = CARTESIAN_POINT ( 'NONE',  ( -2.121784821874999949, 13.48437500061451821, -33.67503911421598417 ) ) ;
#47578 = CARTESIAN_POINT ( 'NONE',  ( 2.737500001229034474, -4.330127018922194537, 2.499999999999995559 ) ) ;
#47579 = CARTESIAN_POINT ( 'NONE',  ( 6.524999999999999467, 4.330127018922191873, 2.499999999999999556 ) ) ;
#47580 = ADVANCED_FACE ( 'NONE', ( #29742 ), #7568, .F. ) ;
#47581 = CARTESIAN_POINT ( 'NONE',  ( 3.646875000614519635, 6.054752690667223547, 3.707466751127219781E-16 ) ) ;
#47582 = CARTESIAN_POINT ( 'NONE',  ( 9.159375000614515372, 0.000000000000000000, 5.243569643749999010 ) ) ;
#47583 = CARTESIAN_POINT ( 'NONE',  ( 28.97812500061451502, -4.541064518000419881, 2.621784821874995952 ) ) ;
#47584 = CARTESIAN_POINT ( 'NONE',  ( -5.810221930991193690E-16, 10.88749999999999929, 26.00000000000000355 ) ) ;
#47585 = CARTESIAN_POINT ( 'NONE',  ( -4.761366016028763859, 8.797204459235659968, -26.32883817404464821 ) ) ;
#47586 = CARTESIAN_POINT ( 'NONE',  ( -2.000000000000000000, 19.13750000122903216, 26.53589838486224650 ) ) ;
#47587 = CARTESIAN_POINT ( 'NONE',  ( 4.246875000614519280, -3.027376345333614438, 5.243569643749998122 ) ) ;
#47588 = CARTESIAN_POINT ( 'NONE',  ( 10.88437500061451679, 4.541064518000418104, 2.621784821874999949 ) ) ;
#47589 = CARTESIAN_POINT ( 'NONE',  ( 3.450000000000001510, 0.000000000000000000, 4.999999999999998224 ) ) ;
#47590 = CARTESIAN_POINT ( 'NONE',  ( -2.121784821874999949, 13.87812500061459531, 26.32496088578401938 ) ) ;
#47591 = CARTESIAN_POINT ( 'NONE',  ( 5.025000000000002132, 6.123233995736764310E-16, -4.999999999999998224 ) ) ;
#47592 = CARTESIAN_POINT ( 'NONE',  ( 7.350000000000002309, 4.330127018922192761, -2.499999999999997780 ) ) ;
#47593 = CARTESIAN_POINT ( 'NONE',  ( 16.24687500061451573, 0.000000000000000000, 4.756430356249998326 ) ) ;
#47594 = CARTESIAN_POINT ( 'NONE',  ( 19.41562500061451146, 3.027376345333611329, 5.243569643749999010 ) ) ;
#47595 = CARTESIAN_POINT ( 'NONE',  ( 13.86562500061451431, 3.027376345333613106, -5.243569643749998122 ) ) ;
#47596 = CARTESIAN_POINT ( 'NONE',  ( 23.33437500061451786, 5.492252693125287522, 3.363034840372157021E-16 ) ) ;
#47597 = CARTESIAN_POINT ( 'NONE',  ( 9.496875000614517504, 6.054752690667223547, 3.707466751127219781E-16 ) ) ;
#47598 = CARTESIAN_POINT ( 'NONE',  ( 25.27499999999999858, 6.123233995736764310E-16, -4.999999999999998224 ) ) ;
#47599 = CARTESIAN_POINT ( 'NONE',  ( 21.78750000122903074, 6.123233995736764310E-16, -4.999999999999998224 ) ) ;
#47600 = CARTESIAN_POINT ( 'NONE',  ( 23.92499999999999716, 6.123233995736764310E-16, -4.999999999999998224 ) ) ;
#47601 = CARTESIAN_POINT ( 'NONE',  ( 9.721875000614517148, -6.054752690667223547, -1.112240025338166033E-15 ) ) ;
#47602 = CARTESIAN_POINT ( 'NONE',  ( 26.85937500061451644, -4.541064518000417216, -2.621784821875001281 ) ) ;
#47603 = DIRECTION ( 'NONE',  ( -1.000000000000000000, -0.000000000000000000, -0.000000000000000000 ) ) ;
#47604 = DIRECTION ( 'NONE',  ( -1.000000000000000000, 0.000000000000000000, 0.000000000000000000 ) ) ;
#47605 = CARTESIAN_POINT ( 'NONE',  ( 20.70937500061451786, 4.541064518000418104, -2.621784821874998173 ) ) ;
#47606 = CARTESIAN_POINT ( 'NONE',  ( 12.75937500061451857, 0.000000000000000000, 5.243569643749999010 ) ) ;
#47607 = CARTESIAN_POINT ( 'NONE',  ( -7.967954043666661671E-16, 20.29062499938548214, 34.33755215474603517 ) ) ;
#47608 = CARTESIAN_POINT ( 'NONE',  ( 22.23750000000000071, 5.773502691896255534, 3.535250795749688894E-16 ) ) ;
#47609 = CARTESIAN_POINT ( 'NONE',  ( 2.000000000000000444, 13.92500000000000071, 26.53589838486224650 ) ) ;
#47610 = CARTESIAN_POINT ( 'NONE',  ( 4.243569643749999898, 12.43437500061451750, -30.00000000000000000 ) ) ;
#47611 = CARTESIAN_POINT ( 'NONE',  ( 24.83437500061451431, 4.119189519843966529, 2.378215178124999607 ) ) ;
#47612 = CARTESIAN_POINT ( 'NONE',  ( 15.74062500061451608, 6.054752690667223547, 3.707466751127219781E-16 ) ) ;
#47613 = CARTESIAN_POINT ( 'NONE',  ( 4.012500000000001954, -5.773502691896255534, -1.060575238724906372E-15 ) ) ;
#47614 = CARTESIAN_POINT ( 'NONE',  ( 25.16250000000000142, -5.773502691896255534, -1.060575238724906372E-15 ) ) ;
#47615 = CARTESIAN_POINT ( 'NONE',  ( 15.22500000000000142, -4.330127018922194537, 2.499999999999995559 ) ) ;
#47616 = CARTESIAN_POINT ( 'NONE',  ( -2.121784821874996840, 11.32812500061451644, 33.67503911421598417 ) ) ;
#47617 = CARTESIAN_POINT ( 'NONE',  ( 13.05000000122903536, -2.886751345948129988, 4.999999999999997335 ) ) ;
#47618 = CARTESIAN_POINT ( 'NONE',  ( 23.78437500061451360, 6.421520780324663323E-16, -5.243569643749999010 ) ) ;
#47619 = CARTESIAN_POINT ( 'NONE',  ( 19.73437500061451644, 6.421520780324663323E-16, -5.243569643749999010 ) ) ;
#47620 = CARTESIAN_POINT ( 'NONE',  ( 25.14375000122903359, -2.886751345948116221, 5.000000000000021316 ) ) ;
#47621 = ORIENTED_EDGE ( 'NONE', *, *, #13863, .T. ) ;
#47622 = CARTESIAN_POINT ( 'NONE',  ( 20.72812500061451502, 4.541064518000418104, 2.621784821874999949 ) ) ;
#47623 = CARTESIAN_POINT ( 'NONE',  ( 4.265625000614517326, -6.054752690667223547, -1.112240025338166033E-15 ) ) ;
#47624 = CARTESIAN_POINT ( 'NONE',  ( 17.22187500061451715, 3.027376345333611329, 5.243569643749999010 ) ) ;
#47625 = CARTESIAN_POINT ( 'NONE',  ( 28.13437500061451502, -4.541064518000419881, 2.621784821874995952 ) ) ;
#47626 = CARTESIAN_POINT ( 'NONE',  ( 4.378125000614518925, 6.421520780324663323E-16, -5.243569643749999010 ) ) ;
#47627 = CARTESIAN_POINT ( 'NONE',  ( 21.44062500061452070, -3.027376345333610441, -5.243569643749999898 ) ) ;
#47628 = CARTESIAN_POINT ( 'NONE',  ( -2.121784821874999949, 15.22812500061451679, 26.32496088578401938 ) ) ;
#47629 = CARTESIAN_POINT ( 'NONE',  ( 16.46250000122903501, 4.330127018922192761, -2.499999999999997780 ) ) ;
#47630 = CARTESIAN_POINT ( 'NONE',  ( 12.34687500061451892, -2.746126346562646425, 4.756430356249996549 ) ) ;
#47631 = CARTESIAN_POINT ( 'NONE',  ( 7.490625000614516082, -3.027376345333610441, -5.243569643749999898 ) ) ;
#47632 = LINE ( 'NONE', #70165, #39635 ) ;
#47633 = CARTESIAN_POINT ( 'NONE',  ( 28.94062500061452070, -3.027376345333614438, 5.243569643749998122 ) ) ;
#47634 = CARTESIAN_POINT ( 'NONE',  ( 23.52187500061451786, 3.027376345333611329, 5.243569643749999010 ) ) ;
#47635 = CARTESIAN_POINT ( 'NONE',  ( 14.09062500061451750, -3.027376345333614438, 5.243569643749998122 ) ) ;
#47636 = CARTESIAN_POINT ( 'NONE',  ( 24.30000000122903359, -2.886751345948129988, 4.999999999999997335 ) ) ;
#47637 = EDGE_CURVE ( 'NONE', #50074, #19796, #26035, .T. ) ;
#47638 = CARTESIAN_POINT ( 'NONE',  ( 25.11562500061451431, 3.027376345333613106, -5.243569643749998122 ) ) ;
#47639 = CARTESIAN_POINT ( 'NONE',  ( 18.83437500061451431, 6.421520780324663323E-16, -5.243569643749999010 ) ) ;
#47640 = CARTESIAN_POINT ( 'NONE',  ( 13.90312500061451750, 4.541064518000418104, -2.621784821874998173 ) ) ;
#47641 = CARTESIAN_POINT ( 'NONE',  ( -4.243569643749999898, 17.60937500061451999, 30.00000000000000000 ) ) ;
#47642 = CARTESIAN_POINT ( 'NONE',  ( 19.04062500061451146, -3.027376345333614438, 5.243569643749998122 ) ) ;
#47643 = DIRECTION ( 'NONE',  ( -1.000000000000000000, -0.000000000000000000, -0.000000000000000000 ) ) ;
#47644 = ORIENTED_EDGE ( 'NONE', *, *, #69064, .T. ) ;
#47645 = CARTESIAN_POINT ( 'NONE',  ( 25.50000000000000000, 0.000000000000000000, 4.999999999999998224 ) ) ;
#47646 = CARTESIAN_POINT ( 'NONE',  ( -2.000000000000000000, 11.82500000000000107, -33.46410161513775705 ) ) ;
#47647 = CARTESIAN_POINT ( 'NONE',  ( -3.756430356250001434, 18.86562499938548498, 32.16877607737301048 ) ) ;
#47648 = CARTESIAN_POINT ( 'NONE',  ( 26.72812500061451502, -4.541064518000419881, 2.621784821874995952 ) ) ;
#47649 = CARTESIAN_POINT ( 'NONE',  ( 8.728125000614518569, -4.541064518000419881, 2.621784821874995952 ) ) ;
#47650 = CARTESIAN_POINT ( 'NONE',  ( 21.00000000122903288, 5.773502691896255534, 3.535250795749688894E-16 ) ) ;
#47651 = CARTESIAN_POINT ( 'NONE',  ( 24.10312500061451502, -4.541064518000417216, -2.621784821875001281 ) ) ;
#47652 = CARTESIAN_POINT ( 'NONE',  ( 26.25000000000000000, 4.330127018922192761, -2.499999999999997780 ) ) ;
#47653 = CARTESIAN_POINT ( 'NONE',  ( 27.14062500061451644, -3.027376345333614438, 5.243569643749998122 ) ) ;
#47654 = CARTESIAN_POINT ( 'NONE',  ( 7.678125000614516082, 4.541064518000418104, 2.621784821874999949 ) ) ;
#47655 = ORIENTED_EDGE ( 'NONE', *, *, #31978, .T. ) ;
#47656 = CARTESIAN_POINT ( 'NONE',  ( 24.89062500061451644, -3.027376345333614438, 5.243569643749998122 ) ) ;
#47657 = CARTESIAN_POINT ( 'NONE',  ( 4.528125000614516615, 4.541064518000418104, 2.621784821874999949 ) ) ;
#47658 = CARTESIAN_POINT ( 'NONE',  ( 13.77187500061451786, -5.492252693125287522, -1.008910452111647106E-15 ) ) ;
#47659 = EDGE_CURVE ( 'NONE', #24506, #53197, #68546, .T. ) ;
#47660 = FACE_OUTER_BOUND ( 'NONE', #5742, .T. ) ;
#47661 = CARTESIAN_POINT ( 'NONE',  ( 12.00000000000000000, 0.000000000000000000, 4.999999999999998224 ) ) ;
#47662 = CARTESIAN_POINT ( 'NONE',  ( 13.20937500061451786, 0.000000000000000000, 5.243569643749999010 ) ) ;
#47663 = CARTESIAN_POINT ( 'NONE',  ( 9.112500001229033586, -4.330127018922190985, -2.500000000000001332 ) ) ;
#47664 = CARTESIAN_POINT ( 'NONE',  ( 17.14687500061451786, 6.054752690667223547, 3.707466751127219781E-16 ) ) ;
#47665 = CARTESIAN_POINT ( 'NONE',  ( 16.16250000000000142, -5.773502691896255534, -1.060575238724906372E-15 ) ) ;
#47666 = CARTESIAN_POINT ( 'NONE',  ( 7.284375000614518036, 4.541064518000418104, 2.621784821874999949 ) ) ;
#47667 = CARTESIAN_POINT ( 'NONE',  ( 2.121784821875001281, 11.40312500061451750, -26.32496088578401938 ) ) ;
#47668 = CARTESIAN_POINT ( 'NONE',  ( -5.810221930991193690E-16, 14.03750000000000142, -34.00000000000000000 ) ) ;
#47669 = CARTESIAN_POINT ( 'NONE',  ( 22.05937500061451573, 2.746126346562643317, 4.756430356249998326 ) ) ;
#47670 = CARTESIAN_POINT ( 'NONE',  ( 15.59999999999999964, 0.000000000000000000, 4.999999999999998224 ) ) ;
#47671 = CARTESIAN_POINT ( 'NONE',  ( 25.19062500061451715, 6.054752690667223547, 3.707466751127219781E-16 ) ) ;
#47672 = CARTESIAN_POINT ( 'NONE',  ( 4.243569643749999898, 10.18437500061451750, 30.00000000000000000 ) ) ;
#47673 = DIRECTION ( 'NONE',  ( 0.000000000000000000, 0.000000000000000000, -1.000000000000000000 ) ) ;
#47674 = CARTESIAN_POINT ( 'NONE',  ( 25.47187500061451715, -6.054752690667223547, -1.112240025338166033E-15 ) ) ;
#47675 = CARTESIAN_POINT ( 'NONE',  ( 27.98437500061451289, 4.541064518000418104, 2.621784821874999949 ) ) ;
#47676 = CARTESIAN_POINT ( 'NONE',  ( 4.528125000614516615, 4.541064518000418104, 2.621784821874999949 ) ) ;
#47677 = CARTESIAN_POINT ( 'NONE',  ( 23.07187500061451502, -4.119189519843968306, 2.378215178124996054 ) ) ;
#47678 = CARTESIAN_POINT ( 'NONE',  ( 17.52187500061451431, 3.027376345333613106, -5.243569643749998122 ) ) ;
#47679 = CARTESIAN_POINT ( 'NONE',  ( 8.971875000614515372, 4.119189519843966529, 2.378215178124999607 ) ) ;
#47680 = CARTESIAN_POINT ( 'NONE',  ( 3.328125000614516438, -4.541064518000419881, 2.621784821874995952 ) ) ;
#47681 = CARTESIAN_POINT ( 'NONE',  ( 8.409375000614518925, -4.541064518000417216, -2.621784821875001281 ) ) ;
#47682 = CARTESIAN_POINT ( 'NONE',  ( 17.52187500061451431, 3.027376345333613106, -5.243569643749998122 ) ) ;
#47683 = CARTESIAN_POINT ( 'NONE',  ( 13.72500000122903074, 2.886751345948062486, -5.000000000000113687 ) ) ;
#47684 = CARTESIAN_POINT ( 'NONE',  ( 27.29999999999999716, 0.000000000000000000, 4.999999999999998224 ) ) ;
#47685 = CARTESIAN_POINT ( 'NONE',  ( 27.87187500061451573, 3.027376345333613106, -5.243569643749998122 ) ) ;
#47686 = CARTESIAN_POINT ( 'NONE',  ( 1.878215178125000495, 14.17812499938548321, 26.74683588394047007 ) ) ;
#47687 = CARTESIAN_POINT ( 'NONE',  ( 8.906250001229031099, 0.000000000000000000, 4.999999999999998224 ) ) ;
#47688 = VERTEX_POINT ( 'NONE', #54107 ) ;
#47689 = CARTESIAN_POINT ( 'NONE',  ( 7.124999999999999112, -4.330127018922194537, 2.499999999999995559 ) ) ;
#47690 = CARTESIAN_POINT ( 'NONE',  ( 8.671875000614518214, -4.119189519843968306, 2.378215178124996054 ) ) ;
#47691 = CARTESIAN_POINT ( 'NONE',  ( 22.82812500061451644, 6.421520780324663323E-16, -5.243569643749999010 ) ) ;
#47692 = CARTESIAN_POINT ( 'NONE',  ( 12.75000000000000178, 4.330127018922192761, -2.499999999999997780 ) ) ;
#47693 = CARTESIAN_POINT ( 'NONE',  ( 7.912500001229033408, 4.330127018922192761, -2.499999999999997780 ) ) ;
#47694 = CARTESIAN_POINT ( 'NONE',  ( 6.928125000614516082, -4.541064518000419881, 2.621784821874995952 ) ) ;
#47695 = CARTESIAN_POINT ( 'NONE',  ( 22.50000000000000000, -4.330127018922190985, -2.500000000000001332 ) ) ;
#47696 = CARTESIAN_POINT ( 'NONE',  ( 17.95312500061451644, 4.541064518000418104, -2.621784821874998173 ) ) ;
#47697 = CARTESIAN_POINT ( 'NONE',  ( 4.087540598844761064, -2.879707068604791420, 4.153959617388856884 ) ) ;
#47698 = CARTESIAN_POINT ( 'NONE',  ( 25.35000000122903074, -2.886751345948125991, -5.000000000000000000 ) ) ;
#47699 = CARTESIAN_POINT ( 'NONE',  ( 3.756430356249998770, 19.80312499938548143, 32.16877607737301759 ) ) ;
#47700 = CARTESIAN_POINT ( 'NONE',  ( 4.650000000000001243, 4.330127018922192761, -2.499999999999997780 ) ) ;
#47701 = ORIENTED_EDGE ( 'NONE', *, *, #54220, .T. ) ;
#47702 = CARTESIAN_POINT ( 'NONE',  ( 18.81562500061452070, 3.027376345333613106, -5.243569643749998122 ) ) ;
#47703 = CARTESIAN_POINT ( 'NONE',  ( 27.74062500061451431, -3.027376345333610441, -5.243569643749999898 ) ) ;
#47704 = CARTESIAN_POINT ( 'NONE',  ( 26.97187500061451360, 3.027376345333613106, -5.243569643749998122 ) ) ;
#47705 = CARTESIAN_POINT ( 'NONE',  ( 8.474999999999999645, -4.330127018922194537, 2.499999999999995559 ) ) ;
#47706 = CARTESIAN_POINT ( 'NONE',  ( 10.90312500061451928, 0.000000000000000000, 5.243569643749999010 ) ) ;
#47707 = CARTESIAN_POINT ( 'NONE',  ( 29.27812500061451573, 4.541064518000418104, 2.621784821874999949 ) ) ;
#47708 = CARTESIAN_POINT ( 'NONE',  ( 8.203125000614518214, 0.000000000000000000, 5.243569643749999010 ) ) ;
#47709 = CARTESIAN_POINT ( 'NONE',  ( 14.30625000122903145, 0.000000000000000000, 4.999999999999998224 ) ) ;
#47710 = CARTESIAN_POINT ( 'NONE',  ( -3.000416591977282496E-16, 13.44687500061451857, 25.09994784771203058 ) ) ;
#47711 = CARTESIAN_POINT ( 'NONE',  ( 26.58750000122903145, -4.330127018922194537, 2.499999999999995559 ) ) ;
#47712 = CARTESIAN_POINT ( 'NONE',  ( 19.99687500061451573, -2.746126346562646425, 4.756430356249996549 ) ) ;
#47713 = CARTESIAN_POINT ( 'NONE',  ( 13.64062500061451289, -3.027376345333614438, 5.243569643749998122 ) ) ;
#47714 = CARTESIAN_POINT ( 'NONE',  ( 28.70625000122903003, 0.000000000000000000, 4.999999999999998224 ) ) ;
#47715 = CARTESIAN_POINT ( 'NONE',  ( 9.196875000614518569, -3.027376345333614438, 5.243569643749998122 ) ) ;
#47716 = CARTESIAN_POINT ( 'NONE',  ( 9.271875000614516082, -6.054752690667223547, -1.112240025338166033E-15 ) ) ;
#47717 = CARTESIAN_POINT ( 'NONE',  ( 17.18437500061451573, 4.541064518000418104, 2.621784821874999949 ) ) ;
#47718 = ORIENTED_EDGE ( 'NONE', *, *, #15878, .T. ) ;
#47719 = CARTESIAN_POINT ( 'NONE',  ( 29.44687500061451857, -3.027376345333614438, 5.243569643749998122 ) ) ;
#47720 = CARTESIAN_POINT ( 'NONE',  ( 22.19062500061451715, -3.027376345333614438, 5.243569643749998122 ) ) ;
#47721 = ADVANCED_FACE ( 'NONE', ( #9403 ), #3505, .F. ) ;
#47722 = CARTESIAN_POINT ( 'NONE',  ( 15.83437500061451608, 4.541064518000418104, 2.621784821874999949 ) ) ;
#47723 = CARTESIAN_POINT ( 'NONE',  ( 22.04062500061451502, 6.054752690667223547, 3.707466751127219781E-16 ) ) ;
#47724 = CARTESIAN_POINT ( 'NONE',  ( 8.484601909799253346E-16, 13.81250000000000000, 34.61880215351700230 ) ) ;
#47725 = CARTESIAN_POINT ( 'NONE',  ( 27.62812500061451360, -4.541064518000419881, 2.621784821874995952 ) ) ;
#47726 = CARTESIAN_POINT ( 'NONE',  ( 7.162500001229032520, 0.000000000000000000, 4.999999999999998224 ) ) ;
#47727 = VERTEX_POINT ( 'NONE', #10133 ) ;
#47728 = CARTESIAN_POINT ( 'NONE',  ( 5.775000001229033231, 2.886751345948126879, 4.999999999999999112 ) ) ;
#47729 = CARTESIAN_POINT ( 'NONE',  ( -3.999999999999999112, 18.64999999999999858, -30.00000000000000000 ) ) ;
#47730 = CARTESIAN_POINT ( 'NONE',  ( 25.50000000122903288, 5.773502691896255534, 3.535250795749688894E-16 ) ) ;
#47731 = CARTESIAN_POINT ( 'NONE',  ( -4.000000000000000888, 20.35624999877096641, 32.30940107675850470 ) ) ;
#47732 = EDGE_CURVE ( 'NONE', #48333, #37161, #35501, .T. ) ;
#47733 = CARTESIAN_POINT ( 'NONE',  ( 8.071875000614518569, 3.027376345333613106, -5.243569643749998122 ) ) ;
#47734 = CARTESIAN_POINT ( 'NONE',  ( 4.276577733362700862, 2.590537181842085257, -4.276577733362700862 ) ) ;
#47735 = CARTESIAN_POINT ( 'NONE',  ( 15.25312500061451715, 4.541064518000418104, -2.621784821874998173 ) ) ;
#47736 = CARTESIAN_POINT ( 'NONE',  ( 8.221875000614518925, 3.027376345333611329, 5.243569643749999010 ) ) ;
#47737 = CARTESIAN_POINT ( 'NONE',  ( 27.86250000122903359, 0.000000000000000000, 4.999999999999998224 ) ) ;
#47738 = CLOSED_SHELL ( 'NONE', ( #63892, #56255, #58996, #51871, #45638, #3977, #34487, #22381, #54331, #46002, #37578, #42909, #45503, #38148, #50000, #70271, #1478, #70933, #72125, #12590, #28872, #28309, #29071, #27330, #1080, #27821, #43521, #71684, #61479, #35138, #31836 ) ) ;
#47739 = CARTESIAN_POINT ( 'NONE',  ( 17.85937500061451999, -4.541064518000417216, -2.621784821875001281 ) ) ;
#47740 = CARTESIAN_POINT ( 'NONE',  ( 4.359375000614517326, -4.541064518000417216, -2.621784821875001281 ) ) ;
#47741 = CARTESIAN_POINT ( 'NONE',  ( 1.071796769724491893, 16.19509619066136707, 33.99999999999999289 ) ) ;
#47742 = EDGE_CURVE ( 'NONE', #25563, #66176, #28406, .T. ) ;
#47743 = CARTESIAN_POINT ( 'NONE',  ( 6.065625000614516260, -6.054752690667223547, -1.112240025338166033E-15 ) ) ;
#47744 = CARTESIAN_POINT ( 'NONE',  ( 16.86562500061451786, -6.054752690667223547, -1.112240025338166033E-15 ) ) ;
#47745 = ORIENTED_EDGE ( 'NONE', *, *, #7942, .F. ) ;
#47746 = AXIS2_PLACEMENT_3D ( 'NONE', #54781, #15606, #66599 ) ;
#47747 = CARTESIAN_POINT ( 'NONE',  ( 12.62812500061451537, 4.541064518000418104, 2.621784821874999949 ) ) ;
#47748 = CARTESIAN_POINT ( 'NONE',  ( 5.062500001229035540, -4.330127018922190985, -2.500000000000001332 ) ) ;
#47749 = AXIS2_PLACEMENT_3D ( 'NONE', #35045, #62395, #46139 ) ;
#47750 = CARTESIAN_POINT ( 'NONE',  ( 10.26562500061451644, 3.027376345333613106, -5.243569643749998122 ) ) ;
#47751 = CARTESIAN_POINT ( 'NONE',  ( 20.59687500061451360, -2.746126346562642428, -4.756430356249999214 ) ) ;
#47752 = CARTESIAN_POINT ( 'NONE',  ( 12.00000000000000000, 0.000000000000000000, 4.999999999999998224 ) ) ;
#47753 = CARTESIAN_POINT ( 'NONE',  ( 5.775000001229033231, 2.886751345948126879, 4.999999999999999112 ) ) ;
#47754 = CARTESIAN_POINT ( 'NONE',  ( 20.24999999999999645, -4.330127018922190985, -2.500000000000001332 ) ) ;
#47755 = CARTESIAN_POINT ( 'NONE',  ( 14.52187500061451608, 3.027376345333611329, 5.243569643749999010 ) ) ;
#47756 = CARTESIAN_POINT ( 'NONE',  ( 16.35000000122903430, -2.886751345948125991, -5.000000000000000000 ) ) ;
#47757 = CARTESIAN_POINT ( 'NONE',  ( 22.46250000000000213, -5.773502691896255534, -1.060575238724906372E-15 ) ) ;
#47758 = CARTESIAN_POINT ( 'NONE',  ( 2.121784821874999061, 19.65312500061451573, -33.67503911421598417 ) ) ;
#47759 = CARTESIAN_POINT ( 'NONE',  ( 11.92500000122902826, 2.886751345948062486, -5.000000000000113687 ) ) ;
#47760 = CARTESIAN_POINT ( 'NONE',  ( 4.000000000000000000, 14.90000000122903323, -27.69059892324149885 ) ) ;
#47761 = CARTESIAN_POINT ( 'NONE',  ( 45.00000000000000000, 6.123233995736764310E-16, -4.999999999999998224 ) ) ;
#47762 = EDGE_CURVE ( 'NONE', #2667, #885, #61405, .T. ) ;
#47763 = CARTESIAN_POINT ( 'NONE',  ( 3.912032792714240870, -3.113839981233385679, -4.218888856100475593 ) ) ;
#47764 = CARTESIAN_POINT ( 'NONE',  ( 17.22187500061451715, 3.027376345333611329, 5.243569643749999010 ) ) ;
#47765 = CARTESIAN_POINT ( 'NONE',  ( 29.09999999999999787, 0.000000000000000000, 4.999999999999998224 ) ) ;
#47766 = CARTESIAN_POINT ( 'NONE',  ( 11.95312500061451644, -4.541064518000417216, -2.621784821875001281 ) ) ;
#47767 = CARTESIAN_POINT ( 'NONE',  ( 8.006250001229034297, 0.000000000000000000, 4.999999999999998224 ) ) ;
#47768 = CARTESIAN_POINT ( 'NONE',  ( 24.19687500061451857, -3.027376345333610441, -5.243569643749999898 ) ) ;
#47769 = CARTESIAN_POINT ( 'NONE',  ( 14.97187500061451537, -4.119189519843968306, 2.378215178124996054 ) ) ;
#47770 = CARTESIAN_POINT ( 'NONE',  ( 9.890625000614516438, 6.054752690667223547, 3.707466751127219781E-16 ) ) ;
#47771 = CARTESIAN_POINT ( 'NONE',  ( 15.49687500061451750, -3.027376345333614438, 5.243569643749998122 ) ) ;
#47772 = ORIENTED_EDGE ( 'NONE', *, *, #39082, .F. ) ;
#47773 = CARTESIAN_POINT ( 'NONE',  ( 25.69687500061451502, 6.054752690667223547, 3.707466751127219781E-16 ) ) ;
#47774 = CARTESIAN_POINT ( 'NONE',  ( 28.07812500061451289, -4.541064518000419881, 2.621784821874995952 ) ) ;
#47775 = CARTESIAN_POINT ( 'NONE',  ( 18.29062500061451502, -3.027376345333610441, -5.243569643749999898 ) ) ;
#47776 = CARTESIAN_POINT ( 'NONE',  ( 28.71562500061451573, 3.027376345333613106, -5.243569643749998122 ) ) ;
#47777 = AXIS2_PLACEMENT_3D ( 'NONE', #19411, #7984, #43066 ) ;
#47778 = CARTESIAN_POINT ( 'NONE',  ( 6.600000000000001421, 0.000000000000000000, 4.999999999999998224 ) ) ;
#47779 = CARTESIAN_POINT ( 'NONE',  ( 20.43750000122903643, 6.123233995736764310E-16, -4.999999999999998224 ) ) ;
#47780 = FACE_OUTER_BOUND ( 'NONE', #42477, .T. ) ;
#47781 = CARTESIAN_POINT ( 'NONE',  ( 7.434375000614515727, -2.746126346562642428, -4.756430356249999214 ) ) ;
#47782 = ORIENTED_EDGE ( 'NONE', *, *, #65590, .T. ) ;
#47783 = CARTESIAN_POINT ( 'NONE',  ( 14.62500000000000000, 4.330127018922191873, 2.499999999999999556 ) ) ;
#47784 = CARTESIAN_POINT ( 'NONE',  ( 19.53749999999999432, 5.773502691896255534, 3.535250795749688894E-16 ) ) ;
#47785 = CARTESIAN_POINT ( 'NONE',  ( 16.80937500061451573, 0.000000000000000000, 5.243569643749999010 ) ) ;
#47786 = CARTESIAN_POINT ( 'NONE',  ( 13.41562500061451502, 3.027376345333613106, -5.243569643749998122 ) ) ;
#47787 =( BOUNDED_CURVE ( )  B_SPLINE_CURVE ( 2, ( #71931, #48666, #54570, #43123, #9867, #4700, #54939, #4344, #38301 ),
 .UNSPECIFIED., .F., .F. ) 
 B_SPLINE_CURVE_WITH_KNOTS ( ( 3, 2, 2, 2, 3 ),
 ( 0.4861111111111111049, 0.4907407407407407551, 0.5000000000000000000, 0.5092592592592593004, 0.5138888888888889506 ),
 .UNSPECIFIED. ) 
 CURVE ( )  GEOMETRIC_REPRESENTATION_ITEM ( )  RATIONAL_B_SPLINE_CURVE ( ( 0.9330127018922194093, 0.9330127018922194093, 1.000000000000000000, 0.8660254037844387076, 1.000000000000000000, 0.8660254037844387076, 1.000000000000000000, 0.9330127018922185211, 0.9330127018922192983 ) ) 
 REPRESENTATION_ITEM ( '' )  );
#47789 = EDGE_LOOP ( 'NONE', ( #3032, #70547, #50156, #3506 ) ) ;
#47788 = VECTOR ( 'NONE', #48632, 1000.000000000000000 ) ;
#47790 = CARTESIAN_POINT ( 'NONE',  ( -0.7368805616696195715, 9.859898480082234684, -34.17910162106521454 ) ) ;
#47791 = CARTESIAN_POINT ( 'NONE',  ( -4.243569643749997233, 16.74687500061451928, -27.54997392385601174 ) ) ;
#47792 = CARTESIAN_POINT ( 'NONE',  ( 5.915625000614515905, 3.027376345333611329, 5.243569643749999010 ) ) ;
#47793 = CARTESIAN_POINT ( 'NONE',  ( -1.878215178125001827, 12.94062499938548427, 33.25316411605952283 ) ) ;
#47794 = CARTESIAN_POINT ( 'NONE',  ( 11.58750000000000036, -2.886751345948129988, 4.999999999999997335 ) ) ;
#47795 = CARTESIAN_POINT ( 'NONE',  ( 29.07187500061451502, 5.824947211148865298E-16, -4.756430356249998326 ) ) ;
#47796 = VERTEX_POINT ( 'NONE', #48563 ) ;
#47797 = CARTESIAN_POINT ( 'NONE',  ( 2.121784821875001281, 14.55312500061451786, 33.67503911421598417 ) ) ;
#47798 = CARTESIAN_POINT ( 'NONE',  ( 27.10312500061451502, 0.000000000000000000, 5.243569643749999010 ) ) ;
#47799 = CARTESIAN_POINT ( 'NONE',  ( 7.612500000000000711, -5.773502691896255534, -1.060575238724906372E-15 ) ) ;
#47800 = AXIS2_PLACEMENT_3D ( 'NONE', #36486, #25030, #25403 ) ;
#47801 = CARTESIAN_POINT ( 'NONE',  ( -3.756430356250000102, 17.81562499938548427, 30.00000000000000000 ) ) ;
#47802 = CARTESIAN_POINT ( 'NONE',  ( 23.14687500061451786, -3.027376345333614438, 5.243569643749998122 ) ) ;
#47803 = CARTESIAN_POINT ( 'NONE',  ( 20.69062500061451715, 6.054752690667223547, 3.707466751127219781E-16 ) ) ;
#47804 = CARTESIAN_POINT ( 'NONE',  ( -4.243569643749999898, 17.51562500061459104, -32.45002607614398471 ) ) ;
#47805 = CARTESIAN_POINT ( 'NONE',  ( 23.25000000122903288, 5.773502691896255534, 3.535250795749688894E-16 ) ) ;
#47806 = CARTESIAN_POINT ( 'NONE',  ( 6.178125000614518747, 6.421520780324663323E-16, -5.243569643749999010 ) ) ;
#47807 = CARTESIAN_POINT ( 'NONE',  ( 25.69687500061451502, 5.492252693125287522, 3.363034840372157021E-16 ) ) ;
#47808 = CARTESIAN_POINT ( 'NONE',  ( 23.39062500061451289, 6.054752690667223547, 3.707466751127219781E-16 ) ) ;
#47809 = CARTESIAN_POINT ( 'NONE',  ( 11.33437500061451608, 4.119189519843966529, 2.378215178124999607 ) ) ;
#47810 = CARTESIAN_POINT ( 'NONE',  ( -3.756430356249999214, 15.07812499938548356, 27.83122392262697531 ) ) ;
#47811 = CARTESIAN_POINT ( 'NONE',  ( 17.52187500061451431, 3.027376345333613106, -5.243569643749998122 ) ) ;
#47812 = CARTESIAN_POINT ( 'NONE',  ( 23.89687500061451786, 6.054752690667223547, 3.707466751127219781E-16 ) ) ;
#47813 = CARTESIAN_POINT ( 'NONE',  ( 9.001249775931846008E-16, 13.67187500061451999, 34.90005215228797653 ) ) ;
#47814 = CARTESIAN_POINT ( 'NONE',  ( 5.653125000614517504, -4.541064518000417216, -2.621784821875001281 ) ) ;
#47815 = CARTESIAN_POINT ( 'NONE',  ( 28.82812500061451644, 4.541064518000418104, 2.621784821874999949 ) ) ;
#47816 = CARTESIAN_POINT ( 'NONE',  ( 29.65312500061451573, 4.541064518000418104, -2.621784821874998173 ) ) ;
#47817 = CARTESIAN_POINT ( 'NONE',  ( -2.000000000000001776, 13.70000000000000107, 33.46410161513775705 ) ) ;
#47818 = CARTESIAN_POINT ( 'NONE',  ( 3.374999999999999556, 4.330127018922191873, 2.499999999999999556 ) ) ;
#47819 = CARTESIAN_POINT ( 'NONE',  ( 3.553125000614516082, 4.541064518000418104, -2.621784821874998173 ) ) ;
#47820 = CARTESIAN_POINT ( 'NONE',  ( 7.959375000614516971, -4.541064518000417216, -2.621784821875001281 ) ) ;
#47821 = SHAPE_REPRESENTATION_RELATIONSHIP ( 'NONE' , 'NONE' ,  #25944, #10934 ) ;
#47822 = CARTESIAN_POINT ( 'NONE',  ( 16.46250000122903501, 4.330127018922192761, -2.499999999999997780 ) ) ;
#47823 = CARTESIAN_POINT ( 'NONE',  ( 4.021875000614516082, 3.027376345333613106, -5.243569643749998122 ) ) ;
#47824 = CARTESIAN_POINT ( 'NONE',  ( 11.25000000122903288, -2.886751345948129988, 4.999999999999997335 ) ) ;
#47825 = CARTESIAN_POINT ( 'NONE',  ( 4.190625000614518925, -3.027376345333614438, 5.243569643749998122 ) ) ;
#47826 = CARTESIAN_POINT ( 'NONE',  ( 1.999999999999997335, 13.26874999877096606, 33.46410161513775705 ) ) ;
#47827 = CARTESIAN_POINT ( 'NONE',  ( 20.41875000122903216, 2.886751345948129099, -4.999999999999998224 ) ) ;
#47828 = CARTESIAN_POINT ( 'NONE',  ( 14.22187500061451537, -6.054752690667223547, -1.112240025338166033E-15 ) ) ;
#47829 = CYLINDRICAL_SURFACE ( 'NONE', #4292, 4.999999999999998224 ) ;
#47830 = ORIENTED_EDGE ( 'NONE', *, *, #48575, .F. ) ;
#47831 = CARTESIAN_POINT ( 'NONE',  ( 22.64062500061451644, -3.027376345333614438, 5.243569643749998122 ) ) ;
#47832 = CARTESIAN_POINT ( 'NONE',  ( 8.165625000614516793, 3.027376345333611329, 5.243569643749999010 ) ) ;
#47833 = CARTESIAN_POINT ( 'NONE',  ( 25.39687500061451431, -3.027376345333614438, 5.243569643749998122 ) ) ;
#47834 = CARTESIAN_POINT ( 'NONE',  ( 8.690625000614515372, -3.027376345333614438, 5.243569643749998122 ) ) ;
#47835 = DIRECTION ( 'NONE',  ( -0.000000000000000000, -1.000000000000000000, -0.000000000000000000 ) ) ;
#47836 = CARTESIAN_POINT ( 'NONE',  ( 9.900000001229033231, -2.886751345948129988, 4.999999999999997335 ) ) ;
#47837 = EDGE_CURVE ( 'NONE', #22971, #37048, #60354, .T. ) ;
#47838 = CARTESIAN_POINT ( 'NONE',  ( 24.77812500061451217, 4.541064518000418104, 2.621784821874999949 ) ) ;
#47839 = CARTESIAN_POINT ( 'NONE',  ( 4.243569643749999898, 10.99062500061451786, -27.54997392385601529 ) ) ;
#47840 = CARTESIAN_POINT ( 'NONE',  ( 10.83750000122903501, -4.330127018922194537, 2.499999999999995559 ) ) ;
#47841 = CARTESIAN_POINT ( 'NONE',  ( 20.27812500061451573, 4.541064518000418104, 2.621784821874999949 ) ) ;
#47842 = AXIS2_PLACEMENT_3D ( 'NONE', #13928, #69003, #35731 ) ;
#47843 = CARTESIAN_POINT ( 'NONE',  ( 17.42812500061451786, 6.421520780324663323E-16, -5.243569643749999010 ) ) ;
#47844 = CARTESIAN_POINT ( 'NONE',  ( 29.44687500061451857, -2.746126346562646425, 4.756430356249996549 ) ) ;
#47845 = CARTESIAN_POINT ( 'NONE',  ( 18.59999999999999787, 4.330127018922192761, -2.499999999999997780 ) ) ;
#47846 = CARTESIAN_POINT ( 'NONE',  ( 14.06250000122903288, -4.330127018922190985, -2.500000000000001332 ) ) ;
#47847 = AXIS2_PLACEMENT_3D ( 'NONE', #32177, #66522, #49179 ) ;
#47848 = CARTESIAN_POINT ( 'NONE',  ( 10.90312500061451928, 0.000000000000000000, 5.243569643749999010 ) ) ;
#47849 = CARTESIAN_POINT ( 'NONE',  ( 14.46562500061451750, 3.027376345333611329, 5.243569643749999010 ) ) ;
#47850 = AXIS2_PLACEMENT_3D ( 'NONE', #54197, #43482, #37928 ) ;
#47851 = CARTESIAN_POINT ( 'NONE',  ( 23.51250000122903216, -4.330127018922190985, -2.500000000000001332 ) ) ;
#47852 = CARTESIAN_POINT ( 'NONE',  ( 21.42187500061451644, -6.054752690667223547, -1.112240025338166033E-15 ) ) ;
#47853 = CARTESIAN_POINT ( 'NONE',  ( 21.94687500061451857, -3.027376345333610441, -5.243569643749999898 ) ) ;
#47854 = CARTESIAN_POINT ( 'NONE',  ( 7.320879633048903241E-15, 18.20000000122903216, 26.00000000000000355 ) ) ;
#47855 = CARTESIAN_POINT ( 'NONE',  ( 8.325000001229033941, 2.886751345948129099, -4.999999999999998224 ) ) ;
#47856 = CARTESIAN_POINT ( 'NONE',  ( 5.484375000614518214, 4.541064518000418104, 2.621784821874999949 ) ) ;
#47857 = CARTESIAN_POINT ( 'NONE',  ( 24.23437500061451644, 6.421520780324663323E-16, -5.243569643749999010 ) ) ;
#47858 = CARTESIAN_POINT ( 'NONE',  ( 26.62500000122902932, -5.773502691896255534, -1.060575238724906372E-15 ) ) ;
#47859 = CARTESIAN_POINT ( 'NONE',  ( 21.25312500061451715, 0.000000000000000000, 5.243569643749999010 ) ) ;
#47860 = CARTESIAN_POINT ( 'NONE',  ( 25.35937500061451644, 0.000000000000000000, 5.243569643749999010 ) ) ;
#47861 = CARTESIAN_POINT ( 'NONE',  ( -1.878215178124999163, 19.65312499938548285, 26.74683588394047007 ) ) ;
#47862 = CARTESIAN_POINT ( 'NONE',  ( 23.02499999999999858, 6.123233995736764310E-16, -4.999999999999998224 ) ) ;
#47863 = CARTESIAN_POINT ( 'NONE',  ( 11.15625000122903288, 0.000000000000000000, 4.999999999999998224 ) ) ;
#47864 = CARTESIAN_POINT ( 'NONE',  ( 4.921875000614518214, 3.027376345333613106, -5.243569643749998122 ) ) ;
#47865 = CARTESIAN_POINT ( 'NONE',  ( 16.41562500061451857, -6.054752690667223547, -1.112240025338166033E-15 ) ) ;
#47866 = VERTEX_POINT ( 'NONE', #9763 ) ;
#47867 = CARTESIAN_POINT ( 'NONE',  ( 11.36250000000000071, 2.886751345948129099, -4.999999999999997335 ) ) ;
#47868 = CARTESIAN_POINT ( 'NONE',  ( 26.12812500061451360, 4.541064518000418104, 2.621784821874999949 ) ) ;
#47869 = DIRECTION ( 'NONE',  ( -0.000000000000000000, -1.000000000000000000, -0.000000000000000000 ) ) ;
#47870 = DIRECTION ( 'NONE',  ( -1.000000000000000000, -0.000000000000000000, -0.000000000000000000 ) ) ;
#47871 = ADVANCED_FACE ( 'NONE', ( #25283 ), #47829, .T. ) ;
#47872 = CARTESIAN_POINT ( 'NONE',  ( 3.027206758929959385, 3.985217399322934284, -32.62660190005471605 ) ) ;
#47873 = CARTESIAN_POINT ( 'NONE',  ( 14.96250000000000036, 2.886751345948129099, -4.999999999999998224 ) ) ;
#47874 = CARTESIAN_POINT ( 'NONE',  ( 26.77500000122903145, 2.886751345948129099, -4.999999999999998224 ) ) ;
#47875 = CARTESIAN_POINT ( 'NONE',  ( 21.02812500061451573, 6.421520780324663323E-16, -5.243569643749999010 ) ) ;
#47876 = VERTEX_POINT ( 'NONE', #42286 ) ;
#47877 = CARTESIAN_POINT ( 'NONE',  ( 22.19999999999999574, 4.330127018922192761, -2.499999999999997780 ) ) ;
#47878 = CARTESIAN_POINT ( 'NONE',  ( 23.40937500061451715, 4.541064518000418104, -2.621784821874998173 ) ) ;
#47879 = ORIENTED_EDGE ( 'NONE', *, *, #11716, .T. ) ;
#47880 = LINE ( 'NONE', #25335, #25379 ) ;
#47881 = CARTESIAN_POINT ( 'NONE',  ( 13.60312500061451679, 0.000000000000000000, 5.243569643749999010 ) ) ;
#47882 = CARTESIAN_POINT ( 'NONE',  ( 30.00000000000000000, 6.123233995736764310E-16, -4.999999999999998224 ) ) ;
#47883 = CARTESIAN_POINT ( 'NONE',  ( 17.59687500061451360, 0.000000000000000000, 4.756430356249998326 ) ) ;
#47884 = CARTESIAN_POINT ( 'NONE',  ( 28.41562500061451502, 3.027376345333611329, 5.243569643749999010 ) ) ;
#47885 = CARTESIAN_POINT ( 'NONE',  ( 12.03750000122903430, 4.330127018922191873, 2.499999999999999556 ) ) ;
#47886 = VECTOR ( 'NONE', #17298, 1000.000000000000000 ) ;
#47887 = CARTESIAN_POINT ( 'NONE',  ( 18.78749999999999432, -2.886751345948129988, 4.999999999999997335 ) ) ;
#47888 = CARTESIAN_POINT ( 'NONE',  ( 27.29999999999999716, 0.000000000000000000, 4.999999999999998224 ) ) ;
#47889 = CARTESIAN_POINT ( 'NONE',  ( 6.646875000614518747, -3.027376345333610441, -5.243569643749999898 ) ) ;
#47890 = CARTESIAN_POINT ( 'NONE',  ( 20.25937500061451857, 4.541064518000418104, -2.621784821874998173 ) ) ;
#47891 = COLOUR_RGB ( '',0.8941176470588234615, 0.8941176470588234615, 0.8941176470588234615 ) ;
#47892 = DIRECTION ( 'NONE',  ( -1.000000000000000000, -0.000000000000000000, -0.000000000000000000 ) ) ;
#47893 = EDGE_LOOP ( 'NONE', ( #26864, #70926, #51059, #35317 ) ) ;
#47894 = CARTESIAN_POINT ( 'NONE',  ( 27.62812500061451360, -4.541064518000419881, 2.621784821874995952 ) ) ;
#47895 = CARTESIAN_POINT ( 'NONE',  ( 29.18437500061451573, 6.421520780324663323E-16, -5.243569643749999010 ) ) ;
#47896 = CARTESIAN_POINT ( 'NONE',  ( 3.459375000614519635, -4.541064518000417216, -2.621784821875001281 ) ) ;
#47897 = CARTESIAN_POINT ( 'NONE',  ( 16.68750000000000000, -2.886751345948125991, -5.000000000000000000 ) ) ;
#47898 = CARTESIAN_POINT ( 'NONE',  ( 13.49062500061451608, 6.054752690667223547, 3.707466751127219781E-16 ) ) ;
#47899 = DIRECTION ( 'NONE',  ( -0.000000000000000000, -1.000000000000000000, -0.000000000000000000 ) ) ;
#47900 = FACE_OUTER_BOUND ( 'NONE', #9894, .T. ) ;
#47901 = CARTESIAN_POINT ( 'NONE',  ( 27.00000000000000000, -4.330127018922190985, -2.500000000000001332 ) ) ;
#47902 = CARTESIAN_POINT ( 'NONE',  ( 18.00000000122903288, -2.886751345948129988, 4.999999999999997335 ) ) ;
#47903 = CARTESIAN_POINT ( 'NONE',  ( 17.14687500061451786, 5.492252693125287522, 3.363034840372157021E-16 ) ) ;
#47904 = CARTESIAN_POINT ( 'NONE',  ( 6.740625000614516082, 6.054752690667223547, 3.707466751127219781E-16 ) ) ;
#47905 = CARTESIAN_POINT ( 'NONE',  ( 25.43437500061451573, -4.541064518000419881, 2.621784821874995952 ) ) ;
#47906 = CARTESIAN_POINT ( 'NONE',  ( 2.121784821874999061, 17.00937500061451857, 26.32496088578401583 ) ) ;
#47907 = CARTESIAN_POINT ( 'NONE',  ( 23.93437500061451573, 4.541064518000418104, 2.621784821874999949 ) ) ;
#47908 = CARTESIAN_POINT ( 'NONE',  ( 4.500000000000000888, -4.330127018922190985, -2.500000000000001332 ) ) ;
#47909 = CARTESIAN_POINT ( 'NONE',  ( 3.999999999999998668, 11.37500000122903288, 27.69059892324149175 ) ) ;
#47910 = CARTESIAN_POINT ( 'NONE',  ( 11.69062500061451360, 6.054752690667223547, 3.707466751127219781E-16 ) ) ;
#47911 = CARTESIAN_POINT ( 'NONE',  ( 4.875000001229034652, 2.886751345948126879, 4.999999999999999112 ) ) ;
#47912 = CARTESIAN_POINT ( 'NONE',  ( 8.634375000614518569, 4.541064518000418104, 2.621784821874999949 ) ) ;
#47913 = CARTESIAN_POINT ( 'NONE',  ( -0.1380872570243177055, 5.000000000000001776, -26.00000000000000000 ) ) ;
#47914 = VERTEX_POINT ( 'NONE', #42651 ) ;
#47915 = CARTESIAN_POINT ( 'NONE',  ( 8.803125000614517859, -4.541064518000417216, -2.621784821875001281 ) ) ;
#47916 = CARTESIAN_POINT ( 'NONE',  ( 14.22187500061451537, -6.054752690667223547, -1.112240025338166033E-15 ) ) ;
#47917 = DIRECTION ( 'NONE',  ( -1.000000000000000000, -0.000000000000000000, -0.000000000000000000 ) ) ;
#47918 = CARTESIAN_POINT ( 'NONE',  ( 24.07500000122903216, 2.886751345948129099, -4.999999999999998224 ) ) ;
#47919 = CARTESIAN_POINT ( 'NONE',  ( 9.384375000614518569, 6.421520780324663323E-16, -5.243569643749999010 ) ) ;
#47920 = CARTESIAN_POINT ( 'NONE',  ( 11.31562500061451892, 3.027376345333611329, 5.243569643749999010 ) ) ;
#47921 = CARTESIAN_POINT ( 'NONE',  ( 28.18125000122903145, 4.330127018922191873, 2.499999999999999556 ) ) ;
#47922 = CARTESIAN_POINT ( 'NONE',  ( 21.12187500061451573, 3.027376345333613106, -5.243569643749998122 ) ) ;
#47923 = CARTESIAN_POINT ( 'NONE',  ( 0.000000000000000000, 20.00000000000000000, 30.00000000000000000 ) ) ;
#47924 = CARTESIAN_POINT ( 'NONE',  ( 5.437500000000000888, -2.886751345948193048, -4.999999999999883649 ) ) ;
#47925 = CARTESIAN_POINT ( 'NONE',  ( 15.15000000000000036, 0.000000000000000000, 4.999999999999998224 ) ) ;
#47926 = CARTESIAN_POINT ( 'NONE',  ( 2.121784821874999061, 14.30937500061451750, -33.67503911421598417 ) ) ;
#47927 = CARTESIAN_POINT ( 'NONE',  ( 15.23437500061451644, 6.421520780324663323E-16, -5.243569643749999010 ) ) ;
#47928 = CARTESIAN_POINT ( 'NONE',  ( 16.68750000122903288, -4.330127018922194537, 2.499999999999995559 ) ) ;
#47929 = ADVANCED_FACE ( 'NONE', ( #31568 ), #14566, .F. ) ;
#47930 = CARTESIAN_POINT ( 'NONE',  ( 11.37187500061451750, 3.027376345333611329, 5.243569643749999010 ) ) ;
#47931 = CARTESIAN_POINT ( 'NONE',  ( 4.243569643749999898, 17.74062500061451786, -27.54997392385601529 ) ) ;
#47932 = CARTESIAN_POINT ( 'NONE',  ( 17.51250000122903216, 0.000000000000000000, 4.999999999999998224 ) ) ;
#47933 = CARTESIAN_POINT ( 'NONE',  ( 11.95312500061451644, -4.541064518000417216, -2.621784821875001281 ) ) ;
#47934 = ORIENTED_EDGE ( 'NONE', *, *, #38674, .T. ) ;
#47935 = CARTESIAN_POINT ( 'NONE',  ( 16.80000000000000071, 4.330127018922192761, -2.499999999999997780 ) ) ;
#47936 = CARTESIAN_POINT ( 'NONE',  ( 29.28749999999999787, -2.886751345948095793, -5.000000000000054179 ) ) ;
#47937 = CARTESIAN_POINT ( 'NONE',  ( 9.796875000614518214, -3.027376345333610441, -5.243569643749999898 ) ) ;
#47938 = CARTESIAN_POINT ( 'NONE',  ( -1.626862140677534273E-15, 19.53124999877096357, 34.00000000000000000 ) ) ;
#47939 = CARTESIAN_POINT ( 'NONE',  ( 11.51250000122903216, 4.330127018922192761, -2.499999999999997780 ) ) ;
#47940 = CARTESIAN_POINT ( 'NONE',  ( 20.02500000122903145, 2.886751345948129099, -4.999999999999998224 ) ) ;
#47941 = CARTESIAN_POINT ( 'NONE',  ( 17.99062500061451786, 6.054752690667223547, 3.707466751127219781E-16 ) ) ;
#47942 = CARTESIAN_POINT ( 'NONE',  ( 19.90312500061451573, 0.000000000000000000, 5.243569643749999010 ) ) ;
#47943 = CARTESIAN_POINT ( 'NONE',  ( 27.33750000122903145, 4.330127018922191873, 2.499999999999999556 ) ) ;
#47944 = CARTESIAN_POINT ( 'NONE',  ( 25.68750000000000000, -2.886751345948125991, -5.000000000000000000 ) ) ;
#47945 = CARTESIAN_POINT ( 'NONE',  ( 12.67499999999999893, 6.123233995736764310E-16, -4.999999999999998224 ) ) ;
#47946 = AXIS2_PLACEMENT_3D ( 'NONE', #50954, #719, #38789 ) ;
#47947 = CARTESIAN_POINT ( 'NONE',  ( 29.39999999999999858, 4.330127018922192761, -2.499999999999997780 ) ) ;
#47948 = CARTESIAN_POINT ( 'NONE',  ( 28.24687500061451573, -3.027376345333610441, -5.243569643749999898 ) ) ;
#47949 = DIRECTION ( 'NONE',  ( 0.000000000000000000, 1.000000000000000000, -8.673617379884036705E-17 ) ) ;
#47950 = CARTESIAN_POINT ( 'NONE',  ( 2.121784821874999061, 13.85937500061451821, -33.67503911421598417 ) ) ;
#47951 = CARTESIAN_POINT ( 'NONE',  ( 4.162500001229033408, -4.330127018922190985, -2.500000000000001332 ) ) ;
#47952 = CARTESIAN_POINT ( 'NONE',  ( 29.63437500061451502, 6.421520780324663323E-16, -5.243569643749999010 ) ) ;
#47953 =( BOUNDED_CURVE ( )  B_SPLINE_CURVE ( 2, ( #23042, #34128, #44147, #33773, #72215, #45230, #72575 ),
 .UNSPECIFIED., .F., .F. ) 
 B_SPLINE_CURVE_WITH_KNOTS ( ( 3, 2, 2, 3 ),
 ( 0.8900000000000000133, 0.8933333333333333126, 0.8966666666666666119, 0.9000000000000000222 ),
 .UNSPECIFIED. ) 
 CURVE ( )  GEOMETRIC_REPRESENTATION_ITEM ( )  RATIONAL_B_SPLINE_CURVE ( ( 1.000000000000000000, 0.8660254037844387076, 1.000000000000000000, 0.8660254037844387076, 1.000000000000000000, 0.8660254037844387076, 1.000000000000000000 ) ) 
 REPRESENTATION_ITEM ( '' )  );
#47954 = ADVANCED_BREP_SHAPE_REPRESENTATION ( '', ( #22240, #23765 ), #56785 ) ;
#47955 = CARTESIAN_POINT ( 'NONE',  ( 8.634375000614518569, 4.541064518000418104, 2.621784821874999949 ) ) ;
#47956 = CARTESIAN_POINT ( 'NONE',  ( 27.47812500061451502, 4.541064518000418104, 2.621784821874999949 ) ) ;
#47957 = DIRECTION ( 'NONE',  ( 0.000000000000000000, 0.000000000000000000, -1.000000000000000000 ) ) ;
#47958 = CARTESIAN_POINT ( 'NONE',  ( -1.394453263437886604E-15, 19.32500000122903216, 33.99999999999999289 ) ) ;
#47959 = CARTESIAN_POINT ( 'NONE',  ( 6.459375000614518747, 0.000000000000000000, 5.243569643749999010 ) ) ;
#47960 = CARTESIAN_POINT ( 'NONE',  ( 10.39687500061451786, 6.054752690667223547, 3.707466751127219781E-16 ) ) ;
#47961 = CARTESIAN_POINT ( 'NONE',  ( 4.162499999999999645, 2.886751345948129099, -4.999999999999998224 ) ) ;
#47962 = CARTESIAN_POINT ( 'NONE',  ( -3.000416591977282496E-16, 13.84062500061459744, 25.09994784771203058 ) ) ;
#47963 = CARTESIAN_POINT ( 'NONE',  ( 1.071796769724489673, 13.49240381056766758, 26.00000000000000000 ) ) ;
#47964 = CARTESIAN_POINT ( 'NONE',  ( 6.037500000000001421, 5.773502691896255534, 3.535250795749688894E-16 ) ) ;
#47965 = CARTESIAN_POINT ( 'NONE',  ( 14.89687500061451608, 0.000000000000000000, 4.756430356249998326 ) ) ;
#47966 = CARTESIAN_POINT ( 'NONE',  ( 21.14062500061451289, 6.054752690667223547, 3.707466751127219781E-16 ) ) ;
#47967 = CARTESIAN_POINT ( 'NONE',  ( 10.56562500061451715, -6.054752690667223547, -1.112240025338166033E-15 ) ) ;
#47968 = CARTESIAN_POINT ( 'NONE',  ( 24.38437500061451502, -2.746126346562646425, 4.756430356249996549 ) ) ;
#47969 = CARTESIAN_POINT ( 'NONE',  ( 9.271875000614516082, -6.054752690667223547, -1.112240025338166033E-15 ) ) ;
#47970 = CARTESIAN_POINT ( 'NONE',  ( 25.08749999999999858, -2.886751345948129988, 4.999999999999997335 ) ) ;
#47971 = CARTESIAN_POINT ( 'NONE',  ( 21.11250000122903359, 0.000000000000000000, 4.999999999999998224 ) ) ;
#47972 = CARTESIAN_POINT ( 'NONE',  ( 27.81562500061452070, 3.027376345333613106, -5.243569643749998122 ) ) ;
#47973 = FACE_OUTER_BOUND ( 'NONE', #22185, .T. ) ;
#47974 = CARTESIAN_POINT ( 'NONE',  ( 9.684375000614517504, -4.541064518000419881, 2.621784821874995952 ) ) ;
#47975 = CARTESIAN_POINT ( 'NONE',  ( 13.73437500061451821, -4.541064518000419881, 2.621784821874995952 ) ) ;
#47976 = CARTESIAN_POINT ( 'NONE',  ( 26.82187500061451857, -6.054752690667223547, -1.112240025338166033E-15 ) ) ;
#47977 = AXIS2_PLACEMENT_3D ( 'NONE', #32766, #61556, #10232 ) ;
#47978 = DIRECTION ( 'NONE',  ( -0.000000000000000000, -1.000000000000000000, -0.000000000000000000 ) ) ;
#47979 = CARTESIAN_POINT ( 'NONE',  ( 11.92500000000000071, 4.330127018922191873, 2.499999999999999556 ) ) ;
#47980 = CARTESIAN_POINT ( 'NONE',  ( 20.97187500061451715, -6.054752690667223547, -1.112240025338166033E-15 ) ) ;
#47981 = CARTESIAN_POINT ( 'NONE',  ( 12.34687500061452070, -3.027376345333614438, 5.243569643749998122 ) ) ;
#47982 = CARTESIAN_POINT ( 'NONE',  ( 3.756430356250000102, 13.54062499938548392, 30.00000000000000000 ) ) ;
#47983 = CARTESIAN_POINT ( 'NONE',  ( 23.43750000000000000, -2.886751345948125991, -5.000000000000000000 ) ) ;
#47984 = CARTESIAN_POINT ( 'NONE',  ( -2.000000000000001776, 15.94999999999999929, 33.46410161513775705 ) ) ;
#47985 = CARTESIAN_POINT ( 'NONE',  ( 2.121784821875001281, 12.80937500061451928, -26.32496088578401938 ) ) ;
#47986 = CARTESIAN_POINT ( 'NONE',  ( 23.63437500061451502, -4.119189519843968306, 2.378215178124996054 ) ) ;
#47987 = CARTESIAN_POINT ( 'NONE',  ( 14.24062500061451608, -3.027376345333610441, -5.243569643749999898 ) ) ;
#47988 = CARTESIAN_POINT ( 'NONE',  ( 3.412500000000002309, 2.886751345948126879, 4.999999999999999112 ) ) ;
#47989 = CARTESIAN_POINT ( 'NONE',  ( 5.810221930991193690E-16, 18.01249999999999218, 26.00000000000000000 ) ) ;
#47990 = CARTESIAN_POINT ( 'NONE',  ( 25.61250000000000071, -5.773502691896255534, -1.060575238724906372E-15 ) ) ;
#47991 = CARTESIAN_POINT ( 'NONE',  ( 13.04999999999999893, -4.330127018922190985, -2.500000000000001332 ) ) ;
#47992 = CARTESIAN_POINT ( 'NONE',  ( -2.828200636599751609E-16, 17.75000000122903288, 25.38119784648299770 ) ) ;
#47993 = CARTESIAN_POINT ( 'NONE',  ( 10.76250000122903572, 0.000000000000000000, 4.999999999999998224 ) ) ;
#47994 = ADVANCED_FACE ( 'NONE', ( #25660 ), #71831, .F. ) ;
#47995 = CARTESIAN_POINT ( 'NONE',  ( 22.20937500061451431, 0.000000000000000000, 5.243569643749999010 ) ) ;
#47996 = CARTESIAN_POINT ( 'NONE',  ( 17.52187500061451431, 3.027376345333613106, -5.243569643749998122 ) ) ;
#47997 = CARTESIAN_POINT ( 'NONE',  ( 20.32500000122903572, -5.773502691896255534, -1.060575238724906372E-15 ) ) ;
#47998 = ORIENTED_EDGE ( 'NONE', *, *, #57780, .T. ) ;
#47999 = CARTESIAN_POINT ( 'NONE',  ( 18.92812500061451431, 4.541064518000418104, 2.621784821874999949 ) ) ;
#48000 = CARTESIAN_POINT ( 'NONE',  ( 4.078125000614517326, 4.541064518000418104, 2.621784821874999949 ) ) ;
#48001 = CARTESIAN_POINT ( 'NONE',  ( 16.84687500061451715, -3.027376345333614438, 5.243569643749998122 ) ) ;
#48002 = CARTESIAN_POINT ( 'NONE',  ( 28.88437500061451502, 4.541064518000418104, 2.621784821874999949 ) ) ;
#48003 = CARTESIAN_POINT ( 'NONE',  ( 3.890625000614517326, -3.027376345333610441, -5.243569643749999898 ) ) ;
#48004 = CARTESIAN_POINT ( 'NONE',  ( 19.97812500061451502, -4.541064518000419881, 2.621784821874995952 ) ) ;
#48005 = CARTESIAN_POINT ( 'NONE',  ( -2.121784821874996840, 16.27812500061451573, 33.67503911421598417 ) ) ;
#48006 = CARTESIAN_POINT ( 'NONE',  ( 16.80000000122903359, -2.886751345948125991, -5.000000000000000000 ) ) ;
#48007 = CARTESIAN_POINT ( 'NONE',  ( 11.97187500061451892, -5.492252693125287522, -1.008910452111647106E-15 ) ) ;
#48008 = CARTESIAN_POINT ( 'NONE',  ( 7.528125000614515727, 6.421520780324663323E-16, -5.243569643749999010 ) ) ;
#48009 = CARTESIAN_POINT ( 'NONE',  ( 29.42812500061451431, -4.541064518000419881, 2.621784821874995952 ) ) ;
#48010 = CARTESIAN_POINT ( 'NONE',  ( 23.33437500061451786, 6.421520780324663323E-16, -5.243569643749999010 ) ) ;
#48011 = CARTESIAN_POINT ( 'NONE',  ( 13.49062500061451608, 6.054752690667223547, 3.707466751127219781E-16 ) ) ;
#48012 = CARTESIAN_POINT ( 'NONE',  ( 25.57500000122903216, 2.886751345948126879, 4.999999999999999112 ) ) ;
#48013 =( BOUNDED_SURFACE ( )  B_SPLINE_SURFACE ( 1, 2, ( 
 ( #72047, #59856, #31795, #48789, #71316, #20692, #45068, #365, #5899, #34690, #56150, #29163, #40250, #67605, #16970, #63131, #734, #17689, #23966, #18052, #39526, #5544, #11447, #69053, #23243, #68692, #6634, #29521, #35060, #28432, #61679, #6990, #52056, #62052, #6263, #22521, #1460, #28082, #57221, #46514, #39164, #12162, #11078, #33967, #57587, #22872, #33606, #28791, #23607, #50610, #40610, #45794, #68329, #62771, #51695, #1099, #14, #56506, #50969, #46152, #45430, #67964, #39896, #56857, #17337, #62409, #12527, #11808, #34325, #51332, #13973, #40981, #57942, #52415, #13240, #12884, #18773, #41339, #64214, #36511, #19875, #31339, #7349, #19505, #29879, #2896, #36875, #24692, #35778, #46879, #59393, #3272, #63496, #25800, #69418, #1823, #35417, #24330, #53880, #63849, #59031, #64949, #41691, #47236, #42062, #13603, #42428, #8433, #2535, #58301, #7710, #30244, #52777, #2179, #69769, #19137, #36149, #8076, #30969, #58668, #48338, #70127, #30608, #53136, #18415, #25055, #47598, #64585, #53504, #14341, #25427, #47970, #70498, #8803, #16798, #28265, #61869, #50796, #54604, #199, #11637, #26532, #3639, #39355, #44900, #5368, #26163, #56341, #37244, #48702, #11277, #33797, #60493, #20975, #17163, #42789, #22704, #9172, #43528, #37607, #39722, #20603, #27907, #71225, #65310, #5730, #45256, #14700, #67789, #50441, #62240, #34152, #56689, #6089, #28620, #59765, #4009, #72966, #22348, #67436, #31707, #9899, #70863, #32435, #49072, #20237, #66050, #54242, #43162, #60129, #65682, #15070, #71600, #9538, #55974, #32072, #15428, #37972, #28985, #68157, #23431, #7896, #12707, #7530, #18601, #41518, #47062, #40433, #558, #18958, #64037, #923, #18229, #34515, #13416, #40082, #46703, #35965, #58487, #24150, #51157, #57044, #69596, #12344, #23068, #40803, #35603, #45623, #52601, #35244, #7174, #52240, #29702, #57765, #17520, #62596, #11992, #1644, #6450, #68512, #51879, #68873, #51523, #45977, #17874, #69239, #34879, #63316, #41165, #23788, #58122, #57408, #30063, #62950, #6813, #63674, #13064, #29347, #1278, #2007, #24518, #46339, #25617, #3088, #24875, #37432, #2358, #36338, #2722, #20425, #59954, #59583, #53323, #8262, #8996, #25238, #64770, #48154, #14160, #47784, #70318, #19693, #42246, #19322, #31894, #36694, #60313, #30433, #64405, #59216, #15255, #9361, #53694, #70679, #54430, #47422, #31528, #8624, #3829, #31153, #54068, #69952, #41876, #13798, #20054, #52961, #42609, #65134, #14525, #37059, #3464, #26350, #58852, #25984, #48523, #71050, #30793, #42974, #65504, #14892, #48889, #71419, #20796, #43352, #37792, #65874, #45169, #66236, #72507, #5645, #38156, #10815, #15614, #49620, #27820, #39267, #72880, #61779, #66608, #11183, #22618, #38533, #60679, #50353, #55887, #16347, #10093, #67349, #49259, #32623, #22262, #44815, #21896, #32984, #28181, #54789, #33707, #21161, #55524, #72147, #50709, #55163, #38902, #4560, #4195, #16711, #56254, #26724, #112, #61421, #67700, #17072, #39632, #9723, #32256, #71792, #15983, #33349, #5275, #43714, #27088, #44453, #21525, #66983, #61056, #44080, #4918, #10455, #27453, #49983, #41078, #12623, #68422, #62505, #63592, #28531, #12980, #68066, #57682, #11546, #51069, #22975, #56956, #56604, #11903, #34428, #34790, #7087, #35517, #1923, #467, #63229, #45537, #46611, #7446, #17784, #6360, #17434, #29972, #46977, #34063, #69512, #39992, #28892, #6000, #51431, #24428, #833, #29616, #58036, #12259, #40343, #35158, #57323, #52513, #52152, #46248, #23341, #45890, #62864, #6727, #29261, #51791, #1192, #23700, #68788, #1555, #18144, #18872, #40711, #62150, #24065, #69154, #18513, #20337, #64685, #8537, #48439, #35873, #70595, #47692, #65413, #58763, #42523, #13335, #7810, #58397, #14070, #71331, #42158, #70228, #8173, #31066, #30701, #14803, #47333, #2630, #53233, #36973, #30347, #31440, #65049, #69866, #19232, #37346, #2998, #19970, #26265, #42890, #41786, #52875, #13706, #41434, #25526, #70964, #8909, #31808, #59869, #25152, #63950, #9273, #54346, #64316, #53604, #24789, #3740, #2273, #59496, #48802, #36249, #14439, #19602, #36609, #59130, #48069, #53980, #3378, #25899, #39178, #22177, #55441, #49898, #21806, #72423, #27367, #16623, #60225, #43264, #44370, #4111, #38071, #21439, #38445, #54706, #71706, #26639, #66897, #4476, #32901, #60971, #66518, #5193, #55076, #72794, #11093, #33621, #16265, #10371, #43629, #43996, #50269, #44730, #21078, #15898, #4833, #15167, #27731, #65785, #49175, #66151, #10733, #67265, #38820, #15529, #60595, #61335, #10004, #27006, #33265, #49536, #32539, #72060, #55803, #61694, #9639, #56165, #5559, #50624, #28096, #20706, #32173, #37704, #18066, #12541, #62785, #23257, #18430, #45082, #1475, #11460, #45807, #39910, #40996, #22887, #6649, #379, #67618, #35075, #40627, #16984, #29535, #29176, #23981, #7004, #63146, #57601, #63512, #39541, #56873, #1113, #51710, #46166, #62066, #12177, #35432, #34705, #28805, #52070, #68343, #68706, #45445, #62423, #46529, #23620, #6277, #67978, #69071, #33981, #12899, #5913, #57956, #22535, #56520, #28447, #17351, #50982, #11822, #34339, #17703, #7364, #29893, #29, #51346, #748, #40264, #57234, #70880, #58682, #69785, #7726, #20254, #37261, #1838, #59783, #30260, #41354, #69432, #24346, #14719, #52793, #70516, #25817, #2551, #8092, #53520, #25070, #3289, #42445, #36527, #2194, #46894, #18789, #24708, #47252, #58315, #30622, #19152, #42079, #64967, #63864, #9189, #30987, #53152, #36164, #52432, #13254, #35792, #41706, #64601, #48355, #64230, #2914, #13619, #47613, #19892, #8820, #14358, #31357, #70143, #53898, #65328, #19521, #13988, #36893, #25445, #59047, #59412, #42806, #8451, #47988, #32818, #38356, #4750, #26179, #21356, #67181, #43912, #60510, #10649, #54989, #27284 ),
 ( #33179, #44651, #71242, #55356, #43180, #16184, #50182, #37988, #49091, #60145, #72710, #16542, #54260, #39095, #9554, #20622, #48720, #3656, #61612, #32088, #49817, #5112, #4395, #9916, #72341, #26924, #55717, #21722, #15814, #54619, #65699, #15086, #4025, #26550, #37623, #32454, #71619, #66436, #44281, #20992, #31724, #10288, #49449, #15444, #43545, #66066, #71983, #60883, #66812, #27646, #38735, #61255, #22093, #50900, #29094, #40543, #1030, #63059, #67895, #12461, #23899, #39829, #16901, #51630, #57150, #17625, #39456, #68622, #50543, #61977, #23536, #46086, #665, #34256, #29452, #56084, #34992, #22452, #56789, #300, #51989, #33898, #40184, #11379, #5476, #17984, #57521, #28015, #6922, #62705, #1390, #46447, #68985, #56442, #22809, #18342, #34620, #17267, #5832, #40916, #73071, #11013, #28364, #6562, #33534, #45001, #67538, #45361, #62344, #11739, #6194, #28722, #51263, #23173, #45727, #68262, #12099, #1751, #47905, #8735, #69705, #7640, #18708, #31269, #48271, #12816, #70795, #41272, #52348, #7284, #35350, #25733, #63784, #8371, #36810, #13534, #19071, #64517, #36081, #14272, #53441, #47534, #13173, #57874, #29813, #35713, #58235, #69350, #41627, #30178, #53071, #2832, #24264, #20170, #41997, #64147, #47173, #63429, #46813, #52709, #2115, #2466, #59325, #24626, #13910, #58602, #8009, #30899, #19809, #25360, #42362, #30544, #64884, #3205, #24989, #70062, #70434, #36449, #19436, #58963, #53811, #9107, #48635, #60797, #55275, #32366, #65986, #61173, #14634, #44197, #54177, #15366, #9475, #10568, #65616, #49371, #43089, #37174, #4670, #10202, #59700, #72262, #71901, #66728, #49735, #32738, #27200, #33096, #31645, #26465, #43828, #21274, #15730, #3574, #54904, #5028, #4312, #71535, #21639, #37908, #38269, #26097, #60426, #32005, #55635, #15005, #66352, #37542, #71160, #16099, #38649, #20532, #27566, #50097, #72628, #42724, #65245, #60064, #54540, #3942, #49004, #20910, #43462, #9837, #26837, #11659, #57432, #34174, #50819, #947, #45280, #68180, #22371, #11300, #23455, #45646, #28288, #44923, #46000, #61529, #68537, #27929, #17542, #44568, #10927, #55998, #16822, #16456, #67459, #39376, #67813, #40104, #17898, #34905, #33454, #23089, #5391, #6474, #40458, #222, #61895, #50462, #62974, #6836, #67098, #29371, #72989, #33820, #39014, #56364, #51903, #5754, #62617, #12370, #17187, #22727, #12014, #39747, #22012, #34537, #6111, #62263, #56710, #28642, #51180, #584, #57067, #29009, #51546, #65064, #65429, #23811, #32189, #53997, #3013, #58146, #9655, #68896, #37721, #57787, #14455, #71347, #29724, #3394, #7196, #41188, #20354, #31823, #14819, #54362, #7552, #3756, #15182, #30086, #52262, #42905, #48455, #8925, #1665, #59884, #40826, #24174, #37362, #9290, #36989, #25543, #20722, #46362, #26280, #46726, #43280, #35626, #1301, #59511, #48817, #65801, #60241, #31455, #25915, #70979, #18253, #63343, #12729, #35265, #69261, #18623, #63697, #13088, #48086, #19985, #52624, #70612, #42538, #33279, #38460, #66911, #21821, #27381, #39194, #15912, #33637, #45097, #67632, #55818, #44386, #4491, #4847, #11108, #5574, #32554, #49913, #72437, #49190, #61709, #26654, #60609, #27020, #44746, #56181, #10746, #49552, #55091, #5205, #72074, #60986, #16279, #10385, #21455, #44010, #66532, #32917, #43643, #28111, #55454, #11474, #54722, #15543, #38835, #39556, #50640, #61350, #27746, #44, #71720, #50285, #72809, #22549, #22192, #67280, #21092, #66167, #38087, #16639, #4125, #16999, #62081, #10018, #34717, #6291, #23994, #67992, #761, #18078, #40639, #68718, #51723, #17366, #57613, #50996, #39923, #63158, #35087, #57247, #40276, #69083, #5927, #52083, #394, #62797, #28820, #18444, #11835, #1124, #62437, #28461, #7016, #12553, #56534, #29547, #23633, #1488, #46541, #41009, #63524, #12911, #22901, #23269, #45460, #35444, #34353, #57968, #33997, #45819, #68355, #6660, #51358, #12190, #29189, #56886, #17716, #46179, #39794, #66405, #27981, #38323, #11349, #45327, #33147, #44248, #55324, #67863, #11707, #49417, #34223, #4718, #15781, #43879, #71950, #62311, #27252, #44967, #266, #50149, #55684, #50511, #72679, #50868, #16869, #10979, #49785, #21326, #60850, #72310, #21691, #32787, #5080, #66779, #16509, #39424, #10256, #56756, #5441, #27614, #10617, #26891, #16151, #38703, #61223, #39062, #22776, #22061, #73037, #44619, #67149, #67505, #56409, #61944, #5800, #61576, #33866, #17235, #33500, #22420, #28330, #56049, #12778, #12065, #63746, #45695, #34588, #24226, #18672, #68948, #29420, #24587, #51229, #7600, #17592, #51954, #46052, #47135, #29061, #35315, #6528, #633, #41234, #46776, #23140, #35674, #57837, #30139, #13135, #69311, #58197, #69666, #68229, #63025, #7246, #29775, #52311, #40151, #18306, #41590, #40878, #34957, #52670, #1354, #1713, #51597, #68586, #2078, #19032, #12424, #997, #64108, #13493, #62670, #36041, #57116, #6161, #28690, #57484, #23504, #17948, #40510, #6888, #23863, #46411, #63393, #47493, #2427, #30505, #20872, #13870, #3534, #31964, #8697, #64845, #59660, #31229, #9436, #48597, #42684, #36410, #7969, #53032, #30862, #53400, #64477, #14233, #2792, #48230, #71122, #24950, #15326, #37131, #59288, #42320, #65947, #70024, #43425, #41956, #70754, #54501, #58924, #9068, #8332, #25318, #26057, #14966, #20494, #37504, #36771, #43050, #3903, #47864, #31603, #65576, #54140, #65206, #70393, #60024, #19395, #19769, #26424, #48965, #20129, #53771, #71495, #3167, #58562, #25694, #14596, #57592, #1827, #1465, #18057, #51337, #69774, #41696, #51700, #69059, #12167, #19142, #17694, #24335, #64220, #13609, #46884, #36154, #34696, #47242, #63137, #58673, #18420, #13245, #28796, #30250, #63502, #57947, #29883, #7354, #35422, #24698, #68334, #739, #52421, #57225, #46157, #29526, #46519 ) ),
 .UNSPECIFIED., .F., .F., .F. ) 
 B_SPLINE_SURFACE_WITH_KNOTS ( ( 2, 2 ),
 ( 3, 2, 2, 2, 2, 2, 2, 2, 2, 2, 2, 2, 2, 2, 2, 2, 2, 2, 2, 2, 2, 2, 2, 2, 2, 2, 2, 2, 2, 2, 2, 2, 2, 2, 2, 2, 2, 2, 2, 2, 2, 2, 2, 2, 2, 2, 2, 2, 2, 2, 2, 2, 2, 2, 2, 2, 2, 2, 2, 2, 2, 2, 2, 2, 2, 2, 2, 2, 2, 2, 2, 2, 2, 2, 2, 2, 2, 2, 2, 2, 2, 2, 2, 2, 2, 2, 2, 2, 2, 2, 2, 2, 2, 2, 2, 2, 2, 2, 2, 2, 2, 2, 2, 2, 2, 2, 2, 2, 2, 2, 2, 2, 2, 2, 2, 2, 2, 2, 2, 2, 2, 2, 2, 2, 2, 2, 2, 2, 2, 2, 2, 2, 2, 2, 2, 2, 2, 2, 2, 2, 2, 2, 2, 2, 2, 2, 2, 2, 2, 2, 2, 2, 2, 2, 2, 2, 2, 2, 2, 2, 2, 2, 2, 2, 2, 2, 2, 2, 2, 2, 2, 2, 2, 2, 2, 2, 2, 2, 2, 2, 2, 2, 2, 2, 2, 2, 2, 2, 2, 2, 2, 2, 2, 2, 2, 2, 2, 2, 2, 2, 2, 2, 2, 2, 2, 2, 2, 2, 2, 2, 2, 2, 2, 2, 2, 2, 2, 2, 2, 2, 2, 2, 2, 2, 2, 2, 2, 2, 2, 2, 2, 2, 2, 2, 2, 2, 2, 2, 2, 2, 2, 2, 2, 2, 2, 2, 2, 2, 2, 2, 2, 2, 2, 2, 2, 2, 2, 2, 2, 2, 2, 2, 2, 2, 2, 2, 2, 2, 2, 2, 2, 2, 2, 2, 2, 2, 2, 2, 2, 2, 2, 2, 2, 2, 2, 2, 2, 2, 2, 2, 2, 2, 2, 2, 2, 2, 2, 2, 2, 2, 2, 2, 2, 2, 2, 2, 2, 2, 2, 2, 2, 2, 2, 2, 2, 2, 2, 2, 2, 2, 2, 2, 2, 2, 2, 2, 2, 2, 2, 2, 2, 2, 2, 2, 2, 2, 2, 2, 2, 2, 2, 2, 2, 2, 2, 2, 2, 2, 2, 2, 2, 2, 2, 2, 2, 2, 2, 2, 2, 2, 3 ),
 ( 0.000000000000000000, 1.000000000000000000 ),
 ( 0.000000000000000000, 0.002777777777777777884, 0.005555555555555555768, 0.008333333333333333218, 0.01111111111111111154, 0.01388888888888888812, 0.01666666666666666644, 0.01944444444444444475, 0.02222222222222222307, 0.02500000000000000139, 0.02777777777777777624, 0.03055555555555555455, 0.03333333333333333287, 0.03611111111111110772, 0.03888888888888888951, 0.04166666666666666435, 0.04444444444444444614, 0.04722222222222222099, 0.05000000000000000278, 0.05277777777777777762, 0.05555555555555555247, 0.05833333333333333426, 0.06111111111111110911, 0.06388888888888888395, 0.06666666666666666574, 0.06944444444444444753, 0.07222222222222221544, 0.07499999999999999722, 0.07777777777777777901, 0.08055555555555556080, 0.08333333333333332871, 0.08611111111111111049, 0.08888888888888889228, 0.09166666666666666019, 0.09444444444444444198, 0.09722222222222222376, 0.1000000000000000056, 0.1027777777777777735, 0.1055555555555555552, 0.1083333333333333370, 0.1111111111111111049, 0.1138888888888888867, 0.1166666666666666685, 0.1194444444444444503, 0.1222222222222222182, 0.1250000000000000000, 0.1277777777777777679, 0.1305555555555555636, 0.1333333333333333315, 0.1361111111111110994, 0.1388888888888888951, 0.1416666666666666630, 0.1444444444444444309, 0.1472222222222222265, 0.1499999999999999944, 0.1527777777777777901, 0.1555555555555555580, 0.1583333333333333259, 0.1611111111111111216, 0.1638888888888888895, 0.1666666666666666574, 0.1694444444444444531, 0.1722222222222222210, 0.1749999999999999889, 0.1777777777777777846, 0.1805555555555555525, 0.1833333333333333204, 0.1861111111111111160, 0.1888888888888888840, 0.1916666666666666796, 0.1944444444444444475, 0.1972222222222222154, 0.2000000000000000111, 0.2027777777777777790, 0.2055555555555555469, 0.2083333333333333426, 0.2111111111111111105, 0.2138888888888888784, 0.2166666666666666741, 0.2194444444444444420, 0.2222222222222222099, 0.2250000000000000056, 0.2277777777777777735, 0.2305555555555555691, 0.2333333333333333370, 0.2361111111111111049, 0.2388888888888889006, 0.2416666666666666685, 0.2444444444444444364, 0.2472222222222222321, 0.2500000000000000000, 0.2527777777777777679, 0.2555555555555555358, 0.2583333333333333592, 0.2611111111111111271, 0.2638888888888888951, 0.2666666666666666630, 0.2694444444444444309, 0.2722222222222221988, 0.2750000000000000222, 0.2777777777777777901, 0.2805555555555555580, 0.2833333333333333259, 0.2861111111111110938, 0.2888888888888888618, 0.2916666666666666852, 0.2944444444444444531, 0.2972222222222222210, 0.2999999999999999889, 0.3027777777777777568, 0.3055555555555555802, 0.3083333333333333481, 0.3111111111111111160, 0.3138888888888888840, 0.3166666666666666519, 0.3194444444444444198, 0.3222222222222222432, 0.3250000000000000111, 0.3277777777777777790, 0.3305555555555555469, 0.3333333333333333148, 0.3361111111111111382, 0.3388888888888889062, 0.3416666666666666741, 0.3444444444444444420, 0.3472222222222222099, 0.3499999999999999778, 0.3527777777777778012, 0.3555555555555555691, 0.3583333333333333370, 0.3611111111111111049, 0.3638888888888888729, 0.3666666666666666408, 0.3694444444444444642, 0.3722222222222222321, 0.3750000000000000000, 0.3777777777777777679, 0.3805555555555555358, 0.3833333333333333592, 0.3861111111111111271, 0.3888888888888888951, 0.3916666666666666630, 0.3944444444444444309, 0.3972222222222221988, 0.4000000000000000222, 0.4027777777777777901, 0.4055555555555555580, 0.4083333333333333259, 0.4111111111111110938, 0.4138888888888888618, 0.4166666666666666852, 0.4194444444444444531, 0.4222222222222222210, 0.4249999999999999889, 0.4277777777777777568, 0.4305555555555555802, 0.4333333333333333481, 0.4361111111111111160, 0.4388888888888888840, 0.4416666666666666519, 0.4444444444444444198, 0.4472222222222222432, 0.4500000000000000111, 0.4527777777777777790, 0.4555555555555555469, 0.4583333333333333148, 0.4611111111111111382, 0.4638888888888889062, 0.4666666666666666741, 0.4694444444444444420, 0.4722222222222222099, 0.4749999999999999778, 0.4777777777777778012, 0.4805555555555555691, 0.4833333333333333370, 0.4861111111111111049, 0.4888888888888888729, 0.4916666666666666408, 0.4944444444444444642, 0.4972222222222222321, 0.5000000000000000000, 0.5027777777777777679, 0.5055555555555555358, 0.5083333333333333037, 0.5111111111111110716, 0.5138888888888888395, 0.5166666666666667185, 0.5194444444444444864, 0.5222222222222222543, 0.5250000000000000222, 0.5277777777777777901, 0.5305555555555555580, 0.5333333333333333259, 0.5361111111111110938, 0.5388888888888888618, 0.5416666666666666297, 0.5444444444444443976, 0.5472222222222222765, 0.5500000000000000444, 0.5527777777777778123, 0.5555555555555555802, 0.5583333333333333481, 0.5611111111111111160, 0.5638888888888888840, 0.5666666666666666519, 0.5694444444444444198, 0.5722222222222221877, 0.5749999999999999556, 0.5777777777777777235, 0.5805555555555556024, 0.5833333333333333703, 0.5861111111111111382, 0.5888888888888889062, 0.5916666666666666741, 0.5944444444444444420, 0.5972222222222222099, 0.5999999999999999778, 0.6027777777777777457, 0.6055555555555555136, 0.6083333333333332815, 0.6111111111111111605, 0.6138888888888889284, 0.6166666666666666963, 0.6194444444444444642, 0.6222222222222222321, 0.6250000000000000000, 0.6277777777777777679, 0.6305555555555555358, 0.6333333333333333037, 0.6361111111111110716, 0.6388888888888888395, 0.6416666666666667185, 0.6444444444444444864, 0.6472222222222222543, 0.6500000000000000222, 0.6527777777777777901, 0.6555555555555555580, 0.6583333333333333259, 0.6611111111111110938, 0.6638888888888888618, 0.6666666666666666297, 0.6694444444444443976, 0.6722222222222222765, 0.6750000000000000444, 0.6777777777777778123, 0.6805555555555555802, 0.6833333333333333481, 0.6861111111111111160, 0.6888888888888888840, 0.6916666666666666519, 0.6944444444444444198, 0.6972222222222221877, 0.6999999999999999556, 0.7027777777777777235, 0.7055555555555556024, 0.7083333333333333703, 0.7111111111111111382, 0.7138888888888889062, 0.7166666666666666741, 0.7194444444444444420, 0.7222222222222222099, 0.7249999999999999778, 0.7277777777777777457, 0.7305555555555555136, 0.7333333333333332815, 0.7361111111111111605, 0.7388888888888889284, 0.7416666666666666963, 0.7444444444444444642, 0.7472222222222222321, 0.7500000000000000000, 0.7527777777777777679, 0.7555555555555555358, 0.7583333333333333037, 0.7611111111111110716, 0.7638888888888888395, 0.7666666666666667185, 0.7694444444444444864, 0.7722222222222222543, 0.7750000000000000222, 0.7777777777777777901, 0.7805555555555555580, 0.7833333333333333259, 0.7861111111111110938, 0.7888888888888888618, 0.7916666666666666297, 0.7944444444444443976, 0.7972222222222222765, 0.8000000000000000444, 0.8027777777777778123, 0.8055555555555555802, 0.8083333333333333481, 0.8111111111111111160, 0.8138888888888888840, 0.8166666666666666519, 0.8194444444444444198, 0.8222222222222221877, 0.8249999999999999556, 0.8277777777777777235, 0.8305555555555556024, 0.8333333333333333703, 0.8361111111111111382, 0.8388888888888889062, 0.8416666666666666741, 0.8444444444444444420, 0.8472222222222222099, 0.8499999999999999778, 0.8527777777777777457, 0.8555555555555555136, 0.8583333333333332815, 0.8611111111111111605, 0.8638888888888889284, 0.8666666666666666963, 0.8694444444444444642, 0.8722222222222222321, 0.8750000000000000000, 0.8777777777777777679, 0.8805555555555555358, 0.8833333333333333037, 0.8861111111111110716, 0.8888888888888888395, 0.8916666666666667185, 0.8944444444444444864, 0.8972222222222222543, 0.9000000000000000222, 0.9027777777777777901, 0.9055555555555555580, 0.9083333333333333259, 0.9111111111111110938, 0.9138888888888888618, 0.9166666666666666297, 0.9194444444444443976, 0.9222222222222222765, 0.9250000000000000444, 0.9277777777777778123, 0.9305555555555555802, 0.9333333333333333481, 0.9361111111111111160, 0.9388888888888888840, 0.9416666666666666519, 0.9444444444444444198, 0.9472222222222221877, 0.9499999999999999556, 0.9527777777777777235, 0.9555555555555556024, 0.9583333333333333703, 0.9611111111111111382, 0.9638888888888889062, 0.9666666666666666741, 0.9694444444444444420, 0.9722222222222222099, 0.9749999999999999778, 0.9777777777777777457, 0.9805555555555555136, 0.9833333333333332815, 0.9861111111111111605, 0.9888888888888889284, 0.9916666666666666963, 0.9944444444444444642, 0.9972222222222222321, 1.000000000000000000 ),
 .UNSPECIFIED. ) 
 GEOMETRIC_REPRESENTATION_ITEM ( )  RATIONAL_B_SPLINE_SURFACE ( (
 ( 1.000000000000000000, 0.8660254037844387076, 1.000000000000000000, 0.8660254037844387076, 1.000000000000000000, 0.8660254037844387076, 1.000000000000000000, 0.8660254037844387076, 1.000000000000000000, 0.8660254037844387076, 1.000000000000000000, 0.8660254037844387076, 1.000000000000000000, 0.8660254037844387076, 1.000000000000000000, 0.8660254037844387076, 1.000000000000000000, 0.8660254037844387076, 1.000000000000000000, 0.8660254037844387076, 1.000000000000000000, 0.8660254037844387076, 1.000000000000000000, 0.8660254037844387076, 1.000000000000000000, 0.8660254037844387076, 1.000000000000000000, 0.8660254037844387076, 1.000000000000000000, 0.8660254037844387076, 1.000000000000000000, 0.8660254037844387076, 1.000000000000000000, 0.8660254037844387076, 1.000000000000000000, 0.8660254037844387076, 1.000000000000000000, 0.8660254037844387076, 1.000000000000000000, 0.8660254037844387076, 1.000000000000000000, 0.8660254037844387076, 1.000000000000000000, 0.8660254037844387076, 1.000000000000000000, 0.8660254037844387076, 1.000000000000000000, 0.8660254037844387076, 1.000000000000000000, 0.8660254037844387076, 1.000000000000000000, 0.8660254037844387076, 1.000000000000000000, 0.8660254037844387076, 1.000000000000000000, 0.8660254037844387076, 1.000000000000000000, 0.8660254037844387076, 1.000000000000000000, 0.8660254037844387076, 1.000000000000000000, 0.8660254037844387076, 1.000000000000000000, 0.8660254037844387076, 1.000000000000000000, 0.8660254037844387076, 1.000000000000000000, 0.8660254037844387076, 1.000000000000000000, 0.8660254037844387076, 1.000000000000000000, 0.8660254037844387076, 1.000000000000000000, 0.8660254037844387076, 1.000000000000000000, 0.8660254037844387076, 1.000000000000000000, 0.8660254037844387076, 1.000000000000000000, 0.8660254037844387076, 1.000000000000000000, 0.8660254037844387076, 1.000000000000000000, 0.8660254037844387076, 1.000000000000000000, 0.8660254037844387076, 1.000000000000000000, 0.8660254037844387076, 1.000000000000000000, 0.8660254037844387076, 1.000000000000000000, 0.8660254037844387076, 1.000000000000000000, 0.8660254037844387076, 1.000000000000000000, 0.8660254037844387076, 1.000000000000000000, 0.8660254037844387076, 1.000000000000000000, 0.8660254037844387076, 1.000000000000000000, 0.8660254037844387076, 1.000000000000000000, 0.8660254037844387076, 1.000000000000000000, 0.8660254037844387076, 1.000000000000000000, 0.8660254037844387076, 1.000000000000000000, 0.8660254037844387076, 1.000000000000000000, 0.8660254037844387076, 1.000000000000000000, 0.8660254037844387076, 1.000000000000000000, 0.8660254037844387076, 1.000000000000000000, 0.8660254037844387076, 1.000000000000000000, 0.8660254037844387076, 1.000000000000000000, 0.8660254037844387076, 1.000000000000000000, 0.8660254037844387076, 1.000000000000000000, 0.8660254037844387076, 1.000000000000000000, 0.8660254037844387076, 1.000000000000000000, 0.8660254037844387076, 1.000000000000000000, 0.8660254037844387076, 1.000000000000000000, 0.8660254037844387076, 1.000000000000000000, 0.8660254037844387076, 1.000000000000000000, 0.8660254037844387076, 1.000000000000000000, 0.8660254037844387076, 1.000000000000000000, 0.8660254037844387076, 1.000000000000000000, 0.8660254037844387076, 1.000000000000000000, 0.8660254037844387076, 1.000000000000000000, 0.8660254037844387076, 1.000000000000000000, 0.8660254037844387076, 1.000000000000000000, 0.8660254037844387076, 1.000000000000000000, 0.8660254037844387076, 1.000000000000000000, 0.8660254037844387076, 1.000000000000000000, 0.8660254037844387076, 1.000000000000000000, 0.8660254037844387076, 1.000000000000000000, 0.8660254037844387076, 1.000000000000000000, 0.8660254037844387076, 1.000000000000000000, 0.8660254037844387076, 1.000000000000000000, 0.8660254037844387076, 1.000000000000000000, 0.8660254037844387076, 1.000000000000000000, 0.8660254037844387076, 1.000000000000000000, 0.8660254037844387076, 1.000000000000000000, 0.8660254037844387076, 1.000000000000000000, 0.8660254037844387076, 1.000000000000000000, 0.8660254037844387076, 1.000000000000000000, 0.8660254037844387076, 1.000000000000000000, 0.8660254037844387076, 1.000000000000000000, 0.8660254037844387076, 1.000000000000000000, 0.8660254037844387076, 1.000000000000000000, 0.8660254037844387076, 1.000000000000000000, 0.8660254037844387076, 1.000000000000000000, 0.8660254037844387076, 1.000000000000000000, 0.8660254037844387076, 1.000000000000000000, 0.8660254037844387076, 1.000000000000000000, 0.8660254037844387076, 1.000000000000000000, 0.8660254037844387076, 1.000000000000000000, 0.8660254037844387076, 1.000000000000000000, 0.8660254037844387076, 1.000000000000000000, 0.8660254037844387076, 1.000000000000000000, 0.8660254037844387076, 1.000000000000000000, 0.8660254037844387076, 1.000000000000000000, 0.8660254037844387076, 1.000000000000000000, 0.8660254037844387076, 1.000000000000000000, 0.8660254037844387076, 1.000000000000000000, 0.8660254037844387076, 1.000000000000000000, 0.8660254037844387076, 1.000000000000000000, 0.8660254037844387076, 1.000000000000000000, 0.8660254037844387076, 1.000000000000000000, 0.8660254037844387076, 1.000000000000000000, 0.8660254037844387076, 1.000000000000000000, 0.8660254037844387076, 1.000000000000000000, 0.8660254037844387076, 1.000000000000000000, 0.8660254037844387076, 1.000000000000000000, 0.8660254037844387076, 1.000000000000000000, 0.8660254037844387076, 1.000000000000000000, 0.8660254037844387076, 1.000000000000000000, 0.8660254037844387076, 1.000000000000000000, 0.8660254037844387076, 1.000000000000000000, 0.8660254037844387076, 1.000000000000000000, 0.8660254037844387076, 1.000000000000000000, 0.8660254037844387076, 1.000000000000000000, 0.8660254037844387076, 1.000000000000000000, 0.8660254037844387076, 1.000000000000000000, 0.8660254037844387076, 1.000000000000000000, 0.8660254037844387076, 1.000000000000000000, 0.8660254037844387076, 1.000000000000000000, 0.8660254037844387076, 1.000000000000000000, 0.8660254037844387076, 1.000000000000000000, 0.8660254037844387076, 1.000000000000000000, 0.8660254037844387076, 1.000000000000000000, 0.8660254037844387076, 1.000000000000000000, 0.8660254037844387076, 1.000000000000000000, 0.8660254037844387076, 1.000000000000000000, 0.8660254037844387076, 1.000000000000000000, 0.8660254037844387076, 1.000000000000000000, 0.8660254037844387076, 1.000000000000000000, 0.8660254037844387076, 1.000000000000000000, 0.8660254037844387076, 1.000000000000000000, 0.8660254037844387076, 1.000000000000000000, 0.8660254037844387076, 1.000000000000000000, 0.8660254037844387076, 1.000000000000000000, 0.8660254037844387076, 1.000000000000000000, 0.8660254037844387076, 1.000000000000000000, 0.8660254037844387076, 1.000000000000000000, 0.8660254037844387076, 1.000000000000000000, 0.8660254037844387076, 1.000000000000000000, 0.8660254037844387076, 1.000000000000000000, 0.8660254037844387076, 1.000000000000000000, 0.8660254037844387076, 1.000000000000000000, 0.8660254037844387076, 1.000000000000000000, 0.8660254037844387076, 1.000000000000000000, 0.8660254037844387076, 1.000000000000000000, 0.8660254037844387076, 1.000000000000000000, 0.8660254037844387076, 1.000000000000000000, 0.8660254037844387076, 1.000000000000000000, 0.8660254037844387076, 1.000000000000000000, 0.8660254037844387076, 1.000000000000000000, 0.8660254037844387076, 1.000000000000000000, 0.8660254037844387076, 1.000000000000000000, 0.8660254037844387076, 1.000000000000000000, 0.8660254037844387076, 1.000000000000000000, 0.8660254037844387076, 1.000000000000000000, 0.8660254037844387076, 1.000000000000000000, 0.8660254037844387076, 1.000000000000000000, 0.8660254037844387076, 1.000000000000000000, 0.8660254037844387076, 1.000000000000000000, 0.8660254037844387076, 1.000000000000000000, 0.8660254037844387076, 1.000000000000000000, 0.8660254037844387076, 1.000000000000000000, 0.8660254037844387076, 1.000000000000000000, 0.8660254037844387076, 1.000000000000000000, 0.8660254037844387076, 1.000000000000000000, 0.8660254037844387076, 1.000000000000000000, 0.8660254037844387076, 1.000000000000000000, 0.8660254037844387076, 1.000000000000000000, 0.8660254037844387076, 1.000000000000000000, 0.8660254037844387076, 1.000000000000000000, 0.8660254037844387076, 1.000000000000000000, 0.8660254037844387076, 1.000000000000000000, 0.8660254037844387076, 1.000000000000000000, 0.8660254037844387076, 1.000000000000000000, 0.8660254037844387076, 1.000000000000000000, 0.8660254037844387076, 1.000000000000000000, 0.8660254037844387076, 1.000000000000000000, 0.8660254037844387076, 1.000000000000000000, 0.8660254037844387076, 1.000000000000000000, 0.8660254037844387076, 1.000000000000000000, 0.8660254037844387076, 1.000000000000000000, 0.8660254037844387076, 1.000000000000000000, 0.8660254037844387076, 1.000000000000000000, 0.8660254037844387076, 1.000000000000000000, 0.8660254037844387076, 1.000000000000000000, 0.8660254037844387076, 1.000000000000000000, 0.8660254037844387076, 1.000000000000000000, 0.8660254037844387076, 1.000000000000000000, 0.8660254037844387076, 1.000000000000000000, 0.8660254037844387076, 1.000000000000000000, 0.8660254037844387076, 1.000000000000000000, 0.8660254037844387076, 1.000000000000000000, 0.8660254037844387076, 1.000000000000000000, 0.8660254037844387076, 1.000000000000000000, 0.8660254037844387076, 1.000000000000000000, 0.8660254037844387076, 1.000000000000000000, 0.8660254037844387076, 1.000000000000000000, 0.8660254037844387076, 1.000000000000000000, 0.8660254037844387076, 1.000000000000000000, 0.8660254037844387076, 1.000000000000000000, 0.8660254037844387076, 1.000000000000000000, 0.8660254037844387076, 1.000000000000000000, 0.8660254037844387076, 1.000000000000000000, 0.8660254037844387076, 1.000000000000000000, 0.8660254037844387076, 1.000000000000000000, 0.8660254037844387076, 1.000000000000000000, 0.8660254037844387076, 1.000000000000000000, 0.8660254037844387076, 1.000000000000000000, 0.8660254037844387076, 1.000000000000000000, 0.8660254037844387076, 1.000000000000000000, 0.8660254037844387076, 1.000000000000000000, 0.8660254037844387076, 1.000000000000000000, 0.8660254037844387076, 1.000000000000000000, 0.8660254037844387076, 1.000000000000000000, 0.8660254037844387076, 1.000000000000000000, 0.8660254037844387076, 1.000000000000000000, 0.8660254037844387076, 1.000000000000000000, 0.8660254037844387076, 1.000000000000000000, 0.8660254037844387076, 1.000000000000000000, 0.8660254037844387076, 1.000000000000000000, 0.8660254037844387076, 1.000000000000000000, 0.8660254037844387076, 1.000000000000000000, 0.8660254037844387076, 1.000000000000000000, 0.8660254037844387076, 1.000000000000000000, 0.8660254037844387076, 1.000000000000000000, 0.8660254037844387076, 1.000000000000000000, 0.8660254037844387076, 1.000000000000000000, 0.8660254037844387076, 1.000000000000000000, 0.8660254037844387076, 1.000000000000000000, 0.8660254037844387076, 1.000000000000000000, 0.8660254037844387076, 1.000000000000000000, 0.8660254037844387076, 1.000000000000000000, 0.8660254037844387076, 1.000000000000000000, 0.8660254037844387076, 1.000000000000000000, 0.8660254037844387076, 1.000000000000000000, 0.8660254037844387076, 1.000000000000000000, 0.8660254037844387076, 1.000000000000000000, 0.8660254037844387076, 1.000000000000000000, 0.8660254037844387076, 1.000000000000000000, 0.8660254037844387076, 1.000000000000000000, 0.8660254037844387076, 1.000000000000000000, 0.8660254037844387076, 1.000000000000000000, 0.8660254037844387076, 1.000000000000000000, 0.8660254037844387076, 1.000000000000000000, 0.8660254037844387076, 1.000000000000000000, 0.8660254037844387076, 1.000000000000000000, 0.8660254037844387076, 1.000000000000000000, 0.8660254037844387076, 1.000000000000000000, 0.8660254037844387076, 1.000000000000000000, 0.8660254037844387076, 1.000000000000000000, 0.8660254037844387076, 1.000000000000000000, 0.8660254037844387076, 1.000000000000000000, 0.8660254037844387076, 1.000000000000000000, 0.8660254037844387076, 1.000000000000000000, 0.8660254037844387076, 1.000000000000000000, 0.8660254037844387076, 1.000000000000000000, 0.8660254037844387076, 1.000000000000000000, 0.8660254037844387076, 1.000000000000000000, 0.8660254037844387076, 1.000000000000000000, 0.8660254037844387076, 1.000000000000000000, 0.8660254037844387076, 1.000000000000000000, 0.8660254037844387076, 1.000000000000000000, 0.8660254037844387076, 1.000000000000000000, 0.8660254037844387076, 1.000000000000000000, 0.8660254037844387076, 1.000000000000000000, 0.8660254037844387076, 1.000000000000000000, 0.8660254037844387076, 1.000000000000000000, 0.8660254037844387076, 1.000000000000000000, 0.8660254037844387076, 1.000000000000000000, 0.8660254037844387076, 1.000000000000000000, 0.8660254037844387076, 1.000000000000000000, 0.8660254037844387076, 1.000000000000000000, 0.8660254037844387076, 1.000000000000000000, 0.8660254037844387076, 1.000000000000000000, 0.8660254037844387076, 1.000000000000000000, 0.8660254037844387076, 1.000000000000000000, 0.8660254037844387076, 1.000000000000000000, 0.8660254037844387076, 1.000000000000000000, 0.8660254037844387076, 1.000000000000000000, 0.8660254037844387076, 1.000000000000000000, 0.8660254037844387076, 1.000000000000000000, 0.8660254037844387076, 1.000000000000000000, 0.8660254037844387076, 1.000000000000000000, 0.8660254037844387076, 1.000000000000000000, 0.8660254037844387076, 1.000000000000000000, 0.8660254037844387076, 1.000000000000000000, 0.8660254037844387076, 1.000000000000000000, 0.8660254037844387076, 1.000000000000000000, 0.8660254037844387076, 1.000000000000000000, 0.8660254037844387076, 1.000000000000000000, 0.8660254037844387076, 1.000000000000000000, 0.8660254037844387076, 1.000000000000000000, 0.8660254037844387076, 1.000000000000000000, 0.8660254037844387076, 1.000000000000000000, 0.8660254037844387076, 1.000000000000000000, 0.8660254037844387076, 1.000000000000000000, 0.8660254037844387076, 1.000000000000000000, 0.8660254037844387076, 1.000000000000000000, 0.8660254037844387076, 1.000000000000000000, 0.8660254037844387076, 1.000000000000000000, 0.8660254037844387076, 1.000000000000000000, 0.8660254037844387076, 1.000000000000000000, 0.8660254037844387076, 1.000000000000000000, 0.8660254037844387076, 1.000000000000000000, 0.8660254037844387076, 1.000000000000000000, 0.8660254037844387076, 1.000000000000000000, 0.8660254037844387076, 1.000000000000000000, 0.8660254037844387076, 1.000000000000000000, 0.8660254037844387076, 1.000000000000000000, 0.8660254037844387076, 1.000000000000000000, 0.8660254037844387076, 1.000000000000000000, 0.8660254037844387076, 1.000000000000000000, 0.8660254037844387076, 1.000000000000000000, 0.8660254037844387076, 1.000000000000000000, 0.8660254037844387076, 1.000000000000000000, 0.8660254037844387076, 1.000000000000000000, 0.8660254037844387076, 1.000000000000000000, 0.8660254037844387076, 1.000000000000000000, 0.8660254037844387076, 1.000000000000000000, 0.8660254037844387076, 1.000000000000000000, 0.8660254037844387076, 1.000000000000000000, 0.8660254037844387076, 1.000000000000000000, 0.8660254037844387076, 1.000000000000000000, 0.8660254037844387076, 1.000000000000000000, 0.8660254037844387076, 1.000000000000000000, 0.8660254037844387076, 1.000000000000000000, 0.8660254037844387076, 1.000000000000000000, 0.8660254037844387076, 1.000000000000000000, 0.8660254037844387076, 1.000000000000000000, 0.8660254037844387076, 1.000000000000000000, 0.8660254037844387076, 1.000000000000000000, 0.8660254037844387076, 1.000000000000000000, 0.8660254037844387076, 1.000000000000000000, 0.8660254037844387076, 1.000000000000000000, 0.8660254037844387076, 1.000000000000000000, 0.8660254037844387076, 1.000000000000000000, 0.8660254037844387076, 1.000000000000000000, 0.8660254037844387076, 1.000000000000000000, 0.8660254037844387076, 1.000000000000000000, 0.8660254037844387076, 1.000000000000000000, 0.8660254037844387076, 1.000000000000000000, 0.8660254037844387076, 1.000000000000000000, 0.8660254037844387076, 1.000000000000000000, 0.8660254037844387076, 1.000000000000000000, 0.8660254037844387076, 1.000000000000000000, 0.8660254037844387076, 1.000000000000000000, 0.8660254037844387076, 1.000000000000000000, 0.8660254037844387076, 1.000000000000000000),
 ( 1.000000000000000000, 0.8660254037844387076, 1.000000000000000000, 0.8660254037844387076, 1.000000000000000000, 0.8660254037844387076, 1.000000000000000000, 0.8660254037844387076, 1.000000000000000000, 0.8660254037844387076, 1.000000000000000000, 0.8660254037844387076, 1.000000000000000000, 0.8660254037844387076, 1.000000000000000000, 0.8660254037844387076, 1.000000000000000000, 0.8660254037844387076, 1.000000000000000000, 0.8660254037844387076, 1.000000000000000000, 0.8660254037844387076, 1.000000000000000000, 0.8660254037844387076, 1.000000000000000000, 0.8660254037844387076, 1.000000000000000000, 0.8660254037844387076, 1.000000000000000000, 0.8660254037844387076, 1.000000000000000000, 0.8660254037844387076, 1.000000000000000000, 0.8660254037844387076, 1.000000000000000000, 0.8660254037844387076, 1.000000000000000000, 0.8660254037844387076, 1.000000000000000000, 0.8660254037844387076, 1.000000000000000000, 0.8660254037844387076, 1.000000000000000000, 0.8660254037844387076, 1.000000000000000000, 0.8660254037844387076, 1.000000000000000000, 0.8660254037844387076, 1.000000000000000000, 0.8660254037844387076, 1.000000000000000000, 0.8660254037844387076, 1.000000000000000000, 0.8660254037844387076, 1.000000000000000000, 0.8660254037844387076, 1.000000000000000000, 0.8660254037844387076, 1.000000000000000000, 0.8660254037844387076, 1.000000000000000000, 0.8660254037844387076, 1.000000000000000000, 0.8660254037844387076, 1.000000000000000000, 0.8660254037844387076, 1.000000000000000000, 0.8660254037844387076, 1.000000000000000000, 0.8660254037844387076, 1.000000000000000000, 0.8660254037844387076, 1.000000000000000000, 0.8660254037844387076, 1.000000000000000000, 0.8660254037844387076, 1.000000000000000000, 0.8660254037844387076, 1.000000000000000000, 0.8660254037844387076, 1.000000000000000000, 0.8660254037844387076, 1.000000000000000000, 0.8660254037844387076, 1.000000000000000000, 0.8660254037844387076, 1.000000000000000000, 0.8660254037844387076, 1.000000000000000000, 0.8660254037844387076, 1.000000000000000000, 0.8660254037844387076, 1.000000000000000000, 0.8660254037844387076, 1.000000000000000000, 0.8660254037844387076, 1.000000000000000000, 0.8660254037844387076, 1.000000000000000000, 0.8660254037844387076, 1.000000000000000000, 0.8660254037844387076, 1.000000000000000000, 0.8660254037844387076, 1.000000000000000000, 0.8660254037844387076, 1.000000000000000000, 0.8660254037844387076, 1.000000000000000000, 0.8660254037844387076, 1.000000000000000000, 0.8660254037844387076, 1.000000000000000000, 0.8660254037844387076, 1.000000000000000000, 0.8660254037844387076, 1.000000000000000000, 0.8660254037844387076, 1.000000000000000000, 0.8660254037844387076, 1.000000000000000000, 0.8660254037844387076, 1.000000000000000000, 0.8660254037844387076, 1.000000000000000000, 0.8660254037844387076, 1.000000000000000000, 0.8660254037844387076, 1.000000000000000000, 0.8660254037844387076, 1.000000000000000000, 0.8660254037844387076, 1.000000000000000000, 0.8660254037844387076, 1.000000000000000000, 0.8660254037844387076, 1.000000000000000000, 0.8660254037844387076, 1.000000000000000000, 0.8660254037844387076, 1.000000000000000000, 0.8660254037844387076, 1.000000000000000000, 0.8660254037844387076, 1.000000000000000000, 0.8660254037844387076, 1.000000000000000000, 0.8660254037844387076, 1.000000000000000000, 0.8660254037844387076, 1.000000000000000000, 0.8660254037844387076, 1.000000000000000000, 0.8660254037844387076, 1.000000000000000000, 0.8660254037844387076, 1.000000000000000000, 0.8660254037844387076, 1.000000000000000000, 0.8660254037844387076, 1.000000000000000000, 0.8660254037844387076, 1.000000000000000000, 0.8660254037844387076, 1.000000000000000000, 0.8660254037844387076, 1.000000000000000000, 0.8660254037844387076, 1.000000000000000000, 0.8660254037844387076, 1.000000000000000000, 0.8660254037844387076, 1.000000000000000000, 0.8660254037844387076, 1.000000000000000000, 0.8660254037844387076, 1.000000000000000000, 0.8660254037844387076, 1.000000000000000000, 0.8660254037844387076, 1.000000000000000000, 0.8660254037844387076, 1.000000000000000000, 0.8660254037844387076, 1.000000000000000000, 0.8660254037844387076, 1.000000000000000000, 0.8660254037844387076, 1.000000000000000000, 0.8660254037844387076, 1.000000000000000000, 0.8660254037844387076, 1.000000000000000000, 0.8660254037844387076, 1.000000000000000000, 0.8660254037844387076, 1.000000000000000000, 0.8660254037844387076, 1.000000000000000000, 0.8660254037844387076, 1.000000000000000000, 0.8660254037844387076, 1.000000000000000000, 0.8660254037844387076, 1.000000000000000000, 0.8660254037844387076, 1.000000000000000000, 0.8660254037844387076, 1.000000000000000000, 0.8660254037844387076, 1.000000000000000000, 0.8660254037844387076, 1.000000000000000000, 0.8660254037844387076, 1.000000000000000000, 0.8660254037844387076, 1.000000000000000000, 0.8660254037844387076, 1.000000000000000000, 0.8660254037844387076, 1.000000000000000000, 0.8660254037844387076, 1.000000000000000000, 0.8660254037844387076, 1.000000000000000000, 0.8660254037844387076, 1.000000000000000000, 0.8660254037844387076, 1.000000000000000000, 0.8660254037844387076, 1.000000000000000000, 0.8660254037844387076, 1.000000000000000000, 0.8660254037844387076, 1.000000000000000000, 0.8660254037844387076, 1.000000000000000000, 0.8660254037844387076, 1.000000000000000000, 0.8660254037844387076, 1.000000000000000000, 0.8660254037844387076, 1.000000000000000000, 0.8660254037844387076, 1.000000000000000000, 0.8660254037844387076, 1.000000000000000000, 0.8660254037844387076, 1.000000000000000000, 0.8660254037844387076, 1.000000000000000000, 0.8660254037844387076, 1.000000000000000000, 0.8660254037844387076, 1.000000000000000000, 0.8660254037844387076, 1.000000000000000000, 0.8660254037844387076, 1.000000000000000000, 0.8660254037844387076, 1.000000000000000000, 0.8660254037844387076, 1.000000000000000000, 0.8660254037844387076, 1.000000000000000000, 0.8660254037844387076, 1.000000000000000000, 0.8660254037844387076, 1.000000000000000000, 0.8660254037844387076, 1.000000000000000000, 0.8660254037844387076, 1.000000000000000000, 0.8660254037844387076, 1.000000000000000000, 0.8660254037844387076, 1.000000000000000000, 0.8660254037844387076, 1.000000000000000000, 0.8660254037844387076, 1.000000000000000000, 0.8660254037844387076, 1.000000000000000000, 0.8660254037844387076, 1.000000000000000000, 0.8660254037844387076, 1.000000000000000000, 0.8660254037844387076, 1.000000000000000000, 0.8660254037844387076, 1.000000000000000000, 0.8660254037844387076, 1.000000000000000000, 0.8660254037844387076, 1.000000000000000000, 0.8660254037844387076, 1.000000000000000000, 0.8660254037844387076, 1.000000000000000000, 0.8660254037844387076, 1.000000000000000000, 0.8660254037844387076, 1.000000000000000000, 0.8660254037844387076, 1.000000000000000000, 0.8660254037844387076, 1.000000000000000000, 0.8660254037844387076, 1.000000000000000000, 0.8660254037844387076, 1.000000000000000000, 0.8660254037844387076, 1.000000000000000000, 0.8660254037844387076, 1.000000000000000000, 0.8660254037844387076, 1.000000000000000000, 0.8660254037844387076, 1.000000000000000000, 0.8660254037844387076, 1.000000000000000000, 0.8660254037844387076, 1.000000000000000000, 0.8660254037844387076, 1.000000000000000000, 0.8660254037844387076, 1.000000000000000000, 0.8660254037844387076, 1.000000000000000000, 0.8660254037844387076, 1.000000000000000000, 0.8660254037844387076, 1.000000000000000000, 0.8660254037844387076, 1.000000000000000000, 0.8660254037844387076, 1.000000000000000000, 0.8660254037844387076, 1.000000000000000000, 0.8660254037844387076, 1.000000000000000000, 0.8660254037844387076, 1.000000000000000000, 0.8660254037844387076, 1.000000000000000000, 0.8660254037844387076, 1.000000000000000000, 0.8660254037844387076, 1.000000000000000000, 0.8660254037844387076, 1.000000000000000000, 0.8660254037844387076, 1.000000000000000000, 0.8660254037844387076, 1.000000000000000000, 0.8660254037844387076, 1.000000000000000000, 0.8660254037844387076, 1.000000000000000000, 0.8660254037844387076, 1.000000000000000000, 0.8660254037844387076, 1.000000000000000000, 0.8660254037844387076, 1.000000000000000000, 0.8660254037844387076, 1.000000000000000000, 0.8660254037844387076, 1.000000000000000000, 0.8660254037844387076, 1.000000000000000000, 0.8660254037844387076, 1.000000000000000000, 0.8660254037844387076, 1.000000000000000000, 0.8660254037844387076, 1.000000000000000000, 0.8660254037844387076, 1.000000000000000000, 0.8660254037844387076, 1.000000000000000000, 0.8660254037844387076, 1.000000000000000000, 0.8660254037844387076, 1.000000000000000000, 0.8660254037844387076, 1.000000000000000000, 0.8660254037844387076, 1.000000000000000000, 0.8660254037844387076, 1.000000000000000000, 0.8660254037844387076, 1.000000000000000000, 0.8660254037844387076, 1.000000000000000000, 0.8660254037844387076, 1.000000000000000000, 0.8660254037844387076, 1.000000000000000000, 0.8660254037844387076, 1.000000000000000000, 0.8660254037844387076, 1.000000000000000000, 0.8660254037844387076, 1.000000000000000000, 0.8660254037844387076, 1.000000000000000000, 0.8660254037844387076, 1.000000000000000000, 0.8660254037844387076, 1.000000000000000000, 0.8660254037844387076, 1.000000000000000000, 0.8660254037844387076, 1.000000000000000000, 0.8660254037844387076, 1.000000000000000000, 0.8660254037844387076, 1.000000000000000000, 0.8660254037844387076, 1.000000000000000000, 0.8660254037844387076, 1.000000000000000000, 0.8660254037844387076, 1.000000000000000000, 0.8660254037844387076, 1.000000000000000000, 0.8660254037844387076, 1.000000000000000000, 0.8660254037844387076, 1.000000000000000000, 0.8660254037844387076, 1.000000000000000000, 0.8660254037844387076, 1.000000000000000000, 0.8660254037844387076, 1.000000000000000000, 0.8660254037844387076, 1.000000000000000000, 0.8660254037844387076, 1.000000000000000000, 0.8660254037844387076, 1.000000000000000000, 0.8660254037844387076, 1.000000000000000000, 0.8660254037844387076, 1.000000000000000000, 0.8660254037844387076, 1.000000000000000000, 0.8660254037844387076, 1.000000000000000000, 0.8660254037844387076, 1.000000000000000000, 0.8660254037844387076, 1.000000000000000000, 0.8660254037844387076, 1.000000000000000000, 0.8660254037844387076, 1.000000000000000000, 0.8660254037844387076, 1.000000000000000000, 0.8660254037844387076, 1.000000000000000000, 0.8660254037844387076, 1.000000000000000000, 0.8660254037844387076, 1.000000000000000000, 0.8660254037844387076, 1.000000000000000000, 0.8660254037844387076, 1.000000000000000000, 0.8660254037844387076, 1.000000000000000000, 0.8660254037844387076, 1.000000000000000000, 0.8660254037844387076, 1.000000000000000000, 0.8660254037844387076, 1.000000000000000000, 0.8660254037844387076, 1.000000000000000000, 0.8660254037844387076, 1.000000000000000000, 0.8660254037844387076, 1.000000000000000000, 0.8660254037844387076, 1.000000000000000000, 0.8660254037844387076, 1.000000000000000000, 0.8660254037844387076, 1.000000000000000000, 0.8660254037844387076, 1.000000000000000000, 0.8660254037844387076, 1.000000000000000000, 0.8660254037844387076, 1.000000000000000000, 0.8660254037844387076, 1.000000000000000000, 0.8660254037844387076, 1.000000000000000000, 0.8660254037844387076, 1.000000000000000000, 0.8660254037844387076, 1.000000000000000000, 0.8660254037844387076, 1.000000000000000000, 0.8660254037844387076, 1.000000000000000000, 0.8660254037844387076, 1.000000000000000000, 0.8660254037844387076, 1.000000000000000000, 0.8660254037844387076, 1.000000000000000000, 0.8660254037844387076, 1.000000000000000000, 0.8660254037844387076, 1.000000000000000000, 0.8660254037844387076, 1.000000000000000000, 0.8660254037844387076, 1.000000000000000000, 0.8660254037844387076, 1.000000000000000000, 0.8660254037844387076, 1.000000000000000000, 0.8660254037844387076, 1.000000000000000000, 0.8660254037844387076, 1.000000000000000000, 0.8660254037844387076, 1.000000000000000000, 0.8660254037844387076, 1.000000000000000000, 0.8660254037844387076, 1.000000000000000000, 0.8660254037844387076, 1.000000000000000000, 0.8660254037844387076, 1.000000000000000000, 0.8660254037844387076, 1.000000000000000000, 0.8660254037844387076, 1.000000000000000000, 0.8660254037844387076, 1.000000000000000000, 0.8660254037844387076, 1.000000000000000000, 0.8660254037844387076, 1.000000000000000000, 0.8660254037844387076, 1.000000000000000000, 0.8660254037844387076, 1.000000000000000000, 0.8660254037844387076, 1.000000000000000000, 0.8660254037844387076, 1.000000000000000000, 0.8660254037844387076, 1.000000000000000000, 0.8660254037844387076, 1.000000000000000000, 0.8660254037844387076, 1.000000000000000000, 0.8660254037844387076, 1.000000000000000000, 0.8660254037844387076, 1.000000000000000000, 0.8660254037844387076, 1.000000000000000000, 0.8660254037844387076, 1.000000000000000000, 0.8660254037844387076, 1.000000000000000000, 0.8660254037844387076, 1.000000000000000000, 0.8660254037844387076, 1.000000000000000000, 0.8660254037844387076, 1.000000000000000000, 0.8660254037844387076, 1.000000000000000000, 0.8660254037844387076, 1.000000000000000000, 0.8660254037844387076, 1.000000000000000000, 0.8660254037844387076, 1.000000000000000000, 0.8660254037844387076, 1.000000000000000000, 0.8660254037844387076, 1.000000000000000000, 0.8660254037844387076, 1.000000000000000000, 0.8660254037844387076, 1.000000000000000000, 0.8660254037844387076, 1.000000000000000000, 0.8660254037844387076, 1.000000000000000000, 0.8660254037844387076, 1.000000000000000000, 0.8660254037844387076, 1.000000000000000000, 0.8660254037844387076, 1.000000000000000000, 0.8660254037844387076, 1.000000000000000000, 0.8660254037844387076, 1.000000000000000000, 0.8660254037844387076, 1.000000000000000000, 0.8660254037844387076, 1.000000000000000000, 0.8660254037844387076, 1.000000000000000000, 0.8660254037844387076, 1.000000000000000000, 0.8660254037844387076, 1.000000000000000000, 0.8660254037844387076, 1.000000000000000000, 0.8660254037844387076, 1.000000000000000000, 0.8660254037844387076, 1.000000000000000000, 0.8660254037844387076, 1.000000000000000000, 0.8660254037844387076, 1.000000000000000000, 0.8660254037844387076, 1.000000000000000000, 0.8660254037844387076, 1.000000000000000000, 0.8660254037844387076, 1.000000000000000000, 0.8660254037844387076, 1.000000000000000000, 0.8660254037844387076, 1.000000000000000000, 0.8660254037844387076, 1.000000000000000000, 0.8660254037844387076, 1.000000000000000000, 0.8660254037844387076, 1.000000000000000000, 0.8660254037844387076, 1.000000000000000000, 0.8660254037844387076, 1.000000000000000000, 0.8660254037844387076, 1.000000000000000000, 0.8660254037844387076, 1.000000000000000000, 0.8660254037844387076, 1.000000000000000000, 0.8660254037844387076, 1.000000000000000000, 0.8660254037844387076, 1.000000000000000000, 0.8660254037844387076, 1.000000000000000000, 0.8660254037844387076, 1.000000000000000000, 0.8660254037844387076, 1.000000000000000000, 0.8660254037844387076, 1.000000000000000000, 0.8660254037844387076, 1.000000000000000000, 0.8660254037844387076, 1.000000000000000000, 0.8660254037844387076, 1.000000000000000000, 0.8660254037844387076, 1.000000000000000000, 0.8660254037844387076, 1.000000000000000000, 0.8660254037844387076, 1.000000000000000000, 0.8660254037844387076, 1.000000000000000000, 0.8660254037844387076, 1.000000000000000000, 0.8660254037844387076, 1.000000000000000000, 0.8660254037844387076, 1.000000000000000000, 0.8660254037844387076, 1.000000000000000000, 0.8660254037844387076, 1.000000000000000000, 0.8660254037844387076, 1.000000000000000000, 0.8660254037844387076, 1.000000000000000000, 0.8660254037844387076, 1.000000000000000000, 0.8660254037844387076, 1.000000000000000000, 0.8660254037844387076, 1.000000000000000000, 0.8660254037844387076, 1.000000000000000000, 0.8660254037844387076, 1.000000000000000000, 0.8660254037844387076, 1.000000000000000000, 0.8660254037844387076, 1.000000000000000000, 0.8660254037844387076, 1.000000000000000000, 0.8660254037844387076, 1.000000000000000000, 0.8660254037844387076, 1.000000000000000000, 0.8660254037844387076, 1.000000000000000000, 0.8660254037844387076, 1.000000000000000000) ) ) 
 REPRESENTATION_ITEM ( '' )  SURFACE ( )  );
#48014 = ADVANCED_FACE ( 'NONE', ( #44124 ), #16751, .T. ) ;
#48015 = CARTESIAN_POINT ( 'NONE',  ( 23.87812500061451715, 4.541064518000418104, 2.621784821874999949 ) ) ;
#48016 = CARTESIAN_POINT ( 'NONE',  ( 18.87187500061451573, 3.027376345333613106, -5.243569643749998122 ) ) ;
#48017 = CARTESIAN_POINT ( 'NONE',  ( 13.86562500061451431, 3.027376345333613106, -5.243569643749998122 ) ) ;
#48018 = CARTESIAN_POINT ( 'NONE',  ( -3.000416591977282496E-16, 15.24687500061451928, 25.09994784771203058 ) ) ;
#48019 = CARTESIAN_POINT ( 'NONE',  ( 19.67812500061451786, 6.421520780324663323E-16, -5.243569643749999010 ) ) ;
#48020 = CARTESIAN_POINT ( 'NONE',  ( 65.00000000000000000, 0.000000000000000000, 0.000000000000000000 ) ) ;
#48021 = VERTEX_POINT ( 'NONE', #39308 ) ;
#48022 = ORIENTED_EDGE ( 'NONE', *, *, #1743, .F. ) ;
#48023 = CARTESIAN_POINT ( 'NONE',  ( 23.06250000000000355, 2.886751345948129099, -4.999999999999998224 ) ) ;
#48024 = CARTESIAN_POINT ( 'NONE',  ( -2.121784821874999949, 19.78437500061451715, -33.67503911421598417 ) ) ;
#48025 = CARTESIAN_POINT ( 'NONE',  ( 3.749583905066019796, -3.307735353520828259, -3.782304699281895832 ) ) ;
#48026 = CARTESIAN_POINT ( 'NONE',  ( 27.92812500061451431, 4.541064518000418104, 2.621784821874999949 ) ) ;
#48027 = CARTESIAN_POINT ( 'NONE',  ( 8.653125000614515727, 0.000000000000000000, 5.243569643749999010 ) ) ;
#48028 = CARTESIAN_POINT ( 'NONE',  ( 19.42500000122903714, -5.773502691896255534, -1.060575238724906372E-15 ) ) ;
#48029 = CARTESIAN_POINT ( 'NONE',  ( 25.86562500061451431, -6.054752690667223547, -1.112240025338166033E-15 ) ) ;
#48030 = CARTESIAN_POINT ( 'NONE',  ( 25.42500000000000071, 4.330127018922191873, 2.499999999999999556 ) ) ;
#48031 = ADVANCED_FACE ( 'NONE', ( #56646 ), #21940, .T. ) ;
#48032 = CARTESIAN_POINT ( 'NONE',  ( 28.94062500061452070, -3.027376345333614438, 5.243569643749998122 ) ) ;
#48033 = CARTESIAN_POINT ( 'NONE',  ( 7.715625000614515727, 3.027376345333611329, 5.243569643749999010 ) ) ;
#48034 = ORIENTED_EDGE ( 'NONE', *, *, #54762, .T. ) ;
#48035 = CARTESIAN_POINT ( 'NONE',  ( 22.94062500061451715, 6.054752690667223547, 3.707466751127219781E-16 ) ) ;
#48036 = CARTESIAN_POINT ( 'NONE',  ( 6.478125000614516793, -4.541064518000419881, 2.621784821874995952 ) ) ;
#48037 = CARTESIAN_POINT ( 'NONE',  ( 14.59687500061452070, -2.746126346562646425, 4.756430356249996549 ) ) ;
#48038 = CARTESIAN_POINT ( 'NONE',  ( 3.242103837493086330E-14, 13.13749999999999929, 26.00000000000000711 ) ) ;
#48039 = CARTESIAN_POINT ( 'NONE',  ( -1.071796769724491005, 10.45759618943233527, -34.00000000000000000 ) ) ;
#48040 = VECTOR ( 'NONE', #28030, 1000.000000000000000 ) ;
#48041 = CARTESIAN_POINT ( 'NONE',  ( 13.53749999999999964, -2.886751345948125991, -5.000000000000000000 ) ) ;
#48042 = CARTESIAN_POINT ( 'NONE',  ( 14.44687500061451679, 6.054752690667223547, 3.707466751127219781E-16 ) ) ;
#48043 = CARTESIAN_POINT ( 'NONE',  ( 9.037500001229034297, -4.330127018922194537, 2.499999999999995559 ) ) ;
#48044 = CARTESIAN_POINT ( 'NONE',  ( 15.57187500061451679, -6.054752690667223547, -1.112240025338166033E-15 ) ) ;
#48045 = CARTESIAN_POINT ( 'NONE',  ( 15.00000000000000000, 4.330127018922192761, -2.499999999999997780 ) ) ;
#48046 = CARTESIAN_POINT ( 'NONE',  ( 9.159375000614515372, 0.000000000000000000, 5.243569643749999010 ) ) ;
#48047 = CARTESIAN_POINT ( 'NONE',  ( -4.243569643749999898, 11.25312500061451892, -30.00000000000000000 ) ) ;
#48048 = CARTESIAN_POINT ( 'NONE',  ( 45.00000000000000000, 6.123233995736764310E-16, -4.999999999999998224 ) ) ;
#48049 = CARTESIAN_POINT ( 'NONE',  ( 12.79687500061451821, -3.027376345333614438, 5.243569643749998122 ) ) ;
#48050 = ORIENTED_EDGE ( 'NONE', *, *, #2473, .T. ) ;
#48051 = CARTESIAN_POINT ( 'NONE',  ( 21.10312500061451502, 4.541064518000418104, -2.621784821874998173 ) ) ;
#48052 = CARTESIAN_POINT ( 'NONE',  ( 2.121784821874999061, 11.15937500061451715, 26.32496088578401583 ) ) ;
#48053 = LINE ( 'NONE', #41058, #10878 ) ;
#48054 = CARTESIAN_POINT ( 'NONE',  ( 25.77187500061451075, 3.027376345333611329, 5.243569643749999010 ) ) ;
#48055 = CARTESIAN_POINT ( 'NONE',  ( 5.390625000614518214, 6.054752690667223547, 3.707466751127219781E-16 ) ) ;
#48056 = CARTESIAN_POINT ( 'NONE',  ( 23.29687500061451644, 4.119189519843966529, -2.378215178124998275 ) ) ;
#48057 = CARTESIAN_POINT ( 'NONE',  ( 16.43437500061451573, -4.541064518000419881, 2.621784821874995952 ) ) ;
#48058 = CARTESIAN_POINT ( 'NONE',  ( 9.609375000614514661, -5.492252693125287522, -1.008910452111647106E-15 ) ) ;
#48059 = CARTESIAN_POINT ( 'NONE',  ( 27.30000000122903359, 5.773502691896255534, 3.535250795749688894E-16 ) ) ;
#48060 = CARTESIAN_POINT ( 'NONE',  ( 6.684375000614518392, 6.421520780324663323E-16, -5.243569643749999010 ) ) ;
#48061 = CARTESIAN_POINT ( 'NONE',  ( 16.69687500061451502, 6.054752690667223547, 3.707466751127219781E-16 ) ) ;
#48062 = CARTESIAN_POINT ( 'NONE',  ( -3.471230998791755784, 25.13294848862673803, 27.99513312867361492 ) ) ;
#48063 = CARTESIAN_POINT ( 'NONE',  ( 24.33749999999999858, -2.886751345948125991, -5.000000000000000000 ) ) ;
#48064 = CARTESIAN_POINT ( 'NONE',  ( 26.33437500061451431, -4.541064518000419881, 2.621784821874995952 ) ) ;
#48065 = DIRECTION ( 'NONE',  ( -1.000000000000000000, -0.000000000000000000, -0.000000000000000000 ) ) ;
#48066 = CARTESIAN_POINT ( 'NONE',  ( 8.324999999999999289, 4.330127018922191873, 2.499999999999999556 ) ) ;
#48067 = CARTESIAN_POINT ( 'NONE',  ( 9.796875000614514661, 4.119189519843966529, -2.378215178124998275 ) ) ;
#48068 = CARTESIAN_POINT ( 'NONE',  ( 21.66562500061451502, 3.027376345333611329, 5.243569643749999010 ) ) ;
#48069 = CARTESIAN_POINT ( 'NONE',  ( 10.72500000000000142, -4.330127018922194537, 2.499999999999995559 ) ) ;
#48070 = CARTESIAN_POINT ( 'NONE',  ( 6.778125000614518392, 4.541064518000418104, 2.621784821874999949 ) ) ;
#48071 = CARTESIAN_POINT ( 'NONE',  ( 19.01249999999999929, 2.886751345948129099, -4.999999999999998224 ) ) ;
#48072 = CARTESIAN_POINT ( 'NONE',  ( 18.96562500061451573, 3.027376345333611329, 5.243569643749999010 ) ) ;
#48073 = CARTESIAN_POINT ( 'NONE',  ( 12.07499999999999929, -4.330127018922194537, 2.499999999999995559 ) ) ;
#48074 = CARTESIAN_POINT ( 'NONE',  ( 23.73750000122903359, 4.330127018922191873, 2.499999999999999556 ) ) ;
#48075 = CARTESIAN_POINT ( 'NONE',  ( 3.756430356250000546, 19.87812499938548427, 27.83122392262697886 ) ) ;
#48076 = CARTESIAN_POINT ( 'NONE',  ( 4.349999999999999645, 0.000000000000000000, 4.999999999999998224 ) ) ;
#48077 = ORIENTED_EDGE ( 'NONE', *, *, #61414, .F. ) ;
#48078 = CARTESIAN_POINT ( 'NONE',  ( 19.90312500061451573, 0.000000000000000000, 5.243569643749999010 ) ) ;
#48079 = CARTESIAN_POINT ( 'NONE',  ( 26.50312500061451360, 4.541064518000418104, -2.621784821874998173 ) ) ;
#48080 = CARTESIAN_POINT ( 'NONE',  ( 24.87187500061451573, 3.027376345333611329, 5.243569643749999010 ) ) ;
#48081 = EDGE_CURVE ( 'NONE', #1783, #48298, #35935, .T. ) ;
#48082 = CARTESIAN_POINT ( 'NONE',  ( 9.899999999999998579, -4.330127018922190985, -2.500000000000001332 ) ) ;
#48083 = EDGE_CURVE ( 'NONE', #50673, #64487, #55564, .T. ) ;
#48084 = CARTESIAN_POINT ( 'NONE',  ( 12.02812500061451573, 6.421520780324663323E-16, -5.243569643749999010 ) ) ;
#48085 = CARTESIAN_POINT ( 'NONE',  ( 26.80312500061451431, -4.541064518000417216, -2.621784821875001281 ) ) ;
#48086 = CARTESIAN_POINT ( 'NONE',  ( 16.05937500061451573, -4.541064518000417216, -2.621784821875001281 ) ) ;
#48087 = CARTESIAN_POINT ( 'NONE',  ( 9.778125000614517504, 6.421520780324663323E-16, -5.243569643749999010 ) ) ;
#48088 = DIRECTION ( 'NONE',  ( 0.000000000000000000, 0.000000000000000000, -1.000000000000000000 ) ) ;
#48089 = CARTESIAN_POINT ( 'NONE',  ( 2.121784821874999061, 11.60937500061451821, 26.32496088578401583 ) ) ;
#48090 = VECTOR ( 'NONE', #63803, 1000.000000000000000 ) ;
#48091 = CARTESIAN_POINT ( 'NONE',  ( 23.73750000122903359, 4.330127018922191873, 2.499999999999999556 ) ) ;
#48092 = CARTESIAN_POINT ( 'NONE',  ( 19.65937500061451360, -4.119189519843965641, -2.378215178125001383 ) ) ;
#48093 = CARTESIAN_POINT ( 'NONE',  ( 14.69062500061451537, -3.027376345333610441, -5.243569643749999898 ) ) ;
#48094 = CARTESIAN_POINT ( 'NONE',  ( 11.14687500061451608, -3.027376345333610441, -5.243569643749999898 ) ) ;
#48095 = CARTESIAN_POINT ( 'NONE',  ( 9.159375000614515372, 0.000000000000000000, 5.243569643749999010 ) ) ;
#48096 = VERTEX_POINT ( 'NONE', #38576 ) ;
#48097 = CARTESIAN_POINT ( 'NONE',  ( -3.968938398713111937, 9.180052406904112061, 34.50384684723260875 ) ) ;
#48098 = CARTESIAN_POINT ( 'NONE',  ( 21.62812500061451360, 4.541064518000418104, 2.621784821874999949 ) ) ;
#48099 = CARTESIAN_POINT ( 'NONE',  ( 17.10937500061451999, 4.541064518000418104, -2.621784821874998173 ) ) ;
#48100 = CARTESIAN_POINT ( 'NONE',  ( 23.05312500061451431, 0.000000000000000000, 5.243569643749999010 ) ) ;
#48101 = CARTESIAN_POINT ( 'NONE',  ( -3.999999999999999112, 11.45000000000000107, 30.00000000000000000 ) ) ;
#48102 = CARTESIAN_POINT ( 'NONE',  ( 28.04062500061451502, -3.027376345333614438, 5.243569643749998122 ) ) ;
#48103 = CARTESIAN_POINT ( 'NONE',  ( 7.912500001229033408, 4.330127018922192761, -2.499999999999997780 ) ) ;
#48104 = VERTEX_POINT ( 'NONE', #5321 ) ;
#48105 = CARTESIAN_POINT ( 'NONE',  ( 29.81250000000000000, 2.886751345948129099, -4.999999999999998224 ) ) ;
#48106 = CARTESIAN_POINT ( 'NONE',  ( 3.999999999999998668, 18.46249999999999858, -32.30940107675850470 ) ) ;
#48107 = CARTESIAN_POINT ( 'NONE',  ( 23.96250000122903145, -4.330127018922190985, -2.500000000000001332 ) ) ;
#48108 = CARTESIAN_POINT ( 'NONE',  ( -3.756430356250000102, 16.12812499938548427, 30.00000000000000000 ) ) ;
#48109 = CARTESIAN_POINT ( 'NONE',  ( 6.571875000614517681, -6.054752690667223547, -1.112240025338166033E-15 ) ) ;
#48110 = DIRECTION ( 'NONE',  ( -0.000000000000000000, -1.000000000000000000, -0.000000000000000000 ) ) ;
#48111 = CARTESIAN_POINT ( 'NONE',  ( 14.35312500061451679, 4.541064518000418104, -2.621784821874998173 ) ) ;
#48112 = CARTESIAN_POINT ( 'NONE',  ( 8.034375000614518925, 6.421520780324663323E-16, -5.243569643749999010 ) ) ;
#48113 = CARTESIAN_POINT ( 'NONE',  ( 26.36250000122903003, 4.330127018922192761, -2.499999999999997780 ) ) ;
#48114 = CARTESIAN_POINT ( 'NONE',  ( 16.58437500061451786, 6.421520780324663323E-16, -5.243569643749999010 ) ) ;
#48115 = CARTESIAN_POINT ( 'NONE',  ( 5.596875000614516260, -3.027376345333614438, 5.243569643749998122 ) ) ;
#48116 = CARTESIAN_POINT ( 'NONE',  ( 1.071796769724497445, 16.37990381179669797, 26.00000000000000355 ) ) ;
#48117 = CARTESIAN_POINT ( 'NONE',  ( 4.678125000614516971, -4.541064518000419881, 2.621784821874995952 ) ) ;
#48118 = CARTESIAN_POINT ( 'NONE',  ( 14.24062500061451608, -3.027376345333610441, -5.243569643749999898 ) ) ;
#48119 = ORIENTED_EDGE ( 'NONE', *, *, #18934, .T. ) ;
#48120 = CARTESIAN_POINT ( 'NONE',  ( 12.02812500061451573, 6.421520780324663323E-16, -5.243569643749999010 ) ) ;
#48121 = CARTESIAN_POINT ( 'NONE',  ( 5.400000001229032343, -2.886751345948129988, 4.999999999999997335 ) ) ;
#48122 = CARTESIAN_POINT ( 'NONE',  ( 10.90312500061451928, 0.000000000000000000, 5.243569643749999010 ) ) ;
#48123 = CARTESIAN_POINT ( 'NONE',  ( 20.55937500061451573, -4.119189519843965641, -2.378215178125001383 ) ) ;
#48124 = CARTESIAN_POINT ( 'NONE',  ( 10.57500000000000107, 4.330127018922191873, 2.499999999999999556 ) ) ;
#48125 = CARTESIAN_POINT ( 'NONE',  ( 4.912500001229034297, 0.000000000000000000, 4.999999999999998224 ) ) ;
#48126 = CARTESIAN_POINT ( 'NONE',  ( 20.77500000000000213, 6.123233995736764310E-16, -4.999999999999998224 ) ) ;
#48127 = CARTESIAN_POINT ( 'NONE',  ( 15.38437500061451679, 4.541064518000418104, 2.621784821874999949 ) ) ;
#48128 = CARTESIAN_POINT ( 'NONE',  ( 15.26250000122903216, 0.000000000000000000, 4.999999999999998224 ) ) ;
#48129 = CARTESIAN_POINT ( 'NONE',  ( 21.56250000000000000, -5.773502691896255534, -1.060575238724906372E-15 ) ) ;
#48130 = CARTESIAN_POINT ( 'NONE',  ( 2.121784821875001281, 18.15312500061451928, -26.32496088578401938 ) ) ;
#48131 = CARTESIAN_POINT ( 'NONE',  ( 0.000000000000000000, 20.00000000000000000, 26.00000000000000000 ) ) ;
#48132 = CARTESIAN_POINT ( 'NONE',  ( 2.000000000000000444, 16.11874999877096570, 26.53589838486224650 ) ) ;
#48133 = CARTESIAN_POINT ( 'NONE',  ( 28.82812500061451644, 4.541064518000418104, 2.621784821874999949 ) ) ;
#48134 = CARTESIAN_POINT ( 'NONE',  ( -5.810221930991193690E-16, 14.60000000122903252, 26.00000000000000355 ) ) ;
#48135 = CARTESIAN_POINT ( 'NONE',  ( 16.09687500061452070, -3.027376345333610441, -5.243569643749999898 ) ) ;
#48136 = CARTESIAN_POINT ( 'NONE',  ( 18.20625000122903003, 4.330127018922192761, -2.499999999999997780 ) ) ;
#48137 = EDGE_CURVE ( 'NONE', #50673, #24022, #68967, .T. ) ;
#48138 = CARTESIAN_POINT ( 'NONE',  ( 11.61562500061451608, 3.027376345333613106, -5.243569643749998122 ) ) ;
#48139 = CARTESIAN_POINT ( 'NONE',  ( 29.74687500061451573, 0.000000000000000000, 4.756430356249998326 ) ) ;
#48140 = CARTESIAN_POINT ( 'NONE',  ( 24.38437500061451502, 4.541064518000418104, 2.621784821874999949 ) ) ;
#48141 = CARTESIAN_POINT ( 'NONE',  ( 16.65937500061451715, 2.746126346562643317, 4.756430356249998326 ) ) ;
#48142 = CARTESIAN_POINT ( 'NONE',  ( 9.065625000614517148, 3.027376345333611329, 5.243569643749999010 ) ) ;
#48143 = CARTESIAN_POINT ( 'NONE',  ( 14.14687500061451786, -3.027376345333614438, 5.243569643749998122 ) ) ;
#48144 = VERTEX_POINT ( 'NONE', #72552 ) ;
#48145 = CARTESIAN_POINT ( 'NONE',  ( 24.15937500061451715, -4.541064518000417216, -2.621784821875001281 ) ) ;
#48146 = CARTESIAN_POINT ( 'NONE',  ( 28.45312500061451289, 0.000000000000000000, 5.243569643749999010 ) ) ;
#48147 = CARTESIAN_POINT ( 'NONE',  ( 2.000000000000001332, 12.61250000122903536, -26.53589838486224650 ) ) ;
#48148 = CARTESIAN_POINT ( 'NONE',  ( 6.299999999999999822, -4.330127018922190985, -2.500000000000001332 ) ) ;
#48149 = CARTESIAN_POINT ( 'NONE',  ( 16.76250000122903216, -4.330127018922190985, -2.500000000000001332 ) ) ;
#48150 = CARTESIAN_POINT ( 'NONE',  ( 7.321875000614517681, -4.119189519843968306, 2.378215178124996054 ) ) ;
#48151 = EDGE_LOOP ( 'NONE', ( #58386, #11280, #25743, #46298 ) ) ;
#48152 = CARTESIAN_POINT ( 'NONE',  ( 14.36249999999999893, -5.773502691896255534, -1.060575238724906372E-15 ) ) ;
#48153 =( BOUNDED_CURVE ( )  B_SPLINE_CURVE ( 2, ( #17001, #44388, #56183, #67634, #61711, #10020, #396 ),
 .UNSPECIFIED., .F., .F. ) 
 B_SPLINE_CURVE_WITH_KNOTS ( ( 3, 2, 2, 3 ),
 ( 0.3916666666666667740, 0.3944444444444444864, 0.3972222222222221433, 0.3999999999999999112 ),
 .UNSPECIFIED. ) 
 CURVE ( )  GEOMETRIC_REPRESENTATION_ITEM ( )  RATIONAL_B_SPLINE_CURVE ( ( 0.9999999999999946709, 0.8660254037844440367, 1.000000000000000000, 0.8660254037844387076, 1.000000000000000000, 0.8660254037844440367, 0.9999999999999946709 ) ) 
 REPRESENTATION_ITEM ( '' )  );
#48154 = CARTESIAN_POINT ( 'NONE',  ( 19.61249999999999716, 2.886751345948126879, 4.999999999999999112 ) ) ;
#48155 = CARTESIAN_POINT ( 'NONE',  ( 13.79062500061451502, -3.027376345333610441, -5.243569643749999898 ) ) ;
#48156 = VERTEX_POINT ( 'NONE', #4599 ) ;
#48157 = DIRECTION ( 'NONE',  ( -0.000000000000000000, -1.000000000000000000, -0.000000000000000000 ) ) ;
#48158 = CARTESIAN_POINT ( 'NONE',  ( -4.243569643749999898, 15.80937500061451573, -30.00000000000000000 ) ) ;
#48159 = CARTESIAN_POINT ( 'NONE',  ( 5.278125000614516615, 6.421520780324663323E-16, -5.243569643749999010 ) ) ;
#48160 = CARTESIAN_POINT ( 'NONE',  ( -1.878215178124999163, 13.24062499938548321, 26.74683588394047007 ) ) ;
#48161 = CARTESIAN_POINT ( 'NONE',  ( 12.22499999999999964, 6.123233995736764310E-16, -4.999999999999998224 ) ) ;
#48162 = CARTESIAN_POINT ( 'NONE',  ( 29.44687500061451146, -4.119189519843965641, -2.378215178125001383 ) ) ;
#48163 = ORIENTED_EDGE ( 'NONE', *, *, #47241, .T. ) ;
#48164 = CARTESIAN_POINT ( 'NONE',  ( 2.121784821874999061, 16.05312500061451786, 26.32496088578401583 ) ) ;
#48165 = CARTESIAN_POINT ( 'NONE',  ( 27.62812500061451360, -4.541064518000419881, 2.621784821874995952 ) ) ;
#48166 = CARTESIAN_POINT ( 'NONE',  ( 7.837499999999999467, 5.773502691896255534, 3.535250795749688894E-16 ) ) ;
#48167 = CARTESIAN_POINT ( 'NONE',  ( 1.878215178124997609, 20.21562499938548285, 33.25316411605952993 ) ) ;
#48168 = CARTESIAN_POINT ( 'NONE',  ( 22.92187500061451644, 3.027376345333613106, -5.243569643749998122 ) ) ;
#48169 = ADVANCED_FACE ( 'NONE', ( #28575 ), #39674, .F. ) ;
#48170 = CARTESIAN_POINT ( 'NONE',  ( 19.79062500061451502, 6.054752690667223547, 3.707466751127219781E-16 ) ) ;
#48171 = CARTESIAN_POINT ( 'NONE',  ( -3.000416591977282496E-16, 13.39062500061459460, -34.90005215228797653 ) ) ;
#48172 = CARTESIAN_POINT ( 'NONE',  ( 23.70000000122903216, 5.773502691896255534, 3.535250795749688894E-16 ) ) ;
#48173 = CARTESIAN_POINT ( 'NONE',  ( 2.990625000614519191, -3.027376345333610441, -5.243569643749999898 ) ) ;
#48174 = CARTESIAN_POINT ( 'NONE',  ( 26.33437500061451431, -4.119189519843968306, 2.378215178124996054 ) ) ;
#48175 = CARTESIAN_POINT ( 'NONE',  ( 22.37812500061451360, 6.421520780324663323E-16, -5.243569643749999010 ) ) ;
#48176 = CARTESIAN_POINT ( 'NONE',  ( 10.77187500061451786, 2.746126346562645981, -4.756430356249997438 ) ) ;
#48177 = CARTESIAN_POINT ( 'NONE',  ( -7.967954043666661671E-16, 16.12812499938548427, 34.33755215474603517 ) ) ;
#48178 = CARTESIAN_POINT ( 'NONE',  ( 17.25937500061451502, 0.000000000000000000, 5.243569643749999010 ) ) ;
#48179 = CARTESIAN_POINT ( 'NONE',  ( 15.87187500061451573, 3.027376345333611329, 5.243569643749999010 ) ) ;
#48180 = CARTESIAN_POINT ( 'NONE',  ( 23.78437500061451360, 6.421520780324663323E-16, -5.243569643749999010 ) ) ;
#48181 = CARTESIAN_POINT ( 'NONE',  ( 4.243569643749999010, 13.37187500061451750, 27.54997392385601174 ) ) ;
#48182 = CARTESIAN_POINT ( 'NONE',  ( 4.603125000614518569, 0.000000000000000000, 5.243569643749999010 ) ) ;
#48183 = CARTESIAN_POINT ( 'NONE',  ( 28.60312500061451502, -4.541064518000417216, -2.621784821875001281 ) ) ;
#48184 = CARTESIAN_POINT ( 'NONE',  ( 28.49062500061451431, -3.027376345333614438, 5.243569643749998122 ) ) ;
#48185 = CARTESIAN_POINT ( 'NONE',  ( -1.999999999999999112, 14.90000000000000036, 26.53589838486224650 ) ) ;
#48186 = LINE ( 'NONE', #57164, #20560 ) ;
#48187 = CARTESIAN_POINT ( 'NONE',  ( 3.328125000614516438, -4.541064518000419881, 2.621784821874995952 ) ) ;
#48188 = CARTESIAN_POINT ( 'NONE',  ( 8.296875000614516438, -3.027376345333614438, 5.243569643749998122 ) ) ;
#48189 = CARTESIAN_POINT ( 'NONE',  ( 13.61250000122903359, -4.330127018922190985, -2.500000000000001332 ) ) ;
#48190 = CARTESIAN_POINT ( 'NONE',  ( 29.42812500061451431, -4.541064518000419881, 2.621784821874995952 ) ) ;
#48191 = CARTESIAN_POINT ( 'NONE',  ( 11.28750000122903252, -4.330127018922194537, 2.499999999999995559 ) ) ;
#48192 = CARTESIAN_POINT ( 'NONE',  ( 4.003125000614518925, 4.541064518000418104, -2.621784821874998173 ) ) ;
#48193 = CARTESIAN_POINT ( 'NONE',  ( -4.000000000000000888, 14.95624999877096606, 32.30940107675850470 ) ) ;
#48194 = CARTESIAN_POINT ( 'NONE',  ( 21.88125000122903074, 4.330127018922191873, 2.499999999999999556 ) ) ;
#48195 = CARTESIAN_POINT ( 'NONE',  ( 15.12187500061451750, -6.054752690667223547, -1.112240025338166033E-15 ) ) ;
#48196 = CARTESIAN_POINT ( 'NONE',  ( 21.46875000122903288, 2.886751345948126879, 4.999999999999998224 ) ) ;
#48197 = ORIENTED_EDGE ( 'NONE', *, *, #52646, .T. ) ;
#48198 = CARTESIAN_POINT ( 'NONE',  ( 21.81562500061451004, -6.054752690667223547, -1.112240025338166033E-15 ) ) ;
#48199 = CARTESIAN_POINT ( 'NONE',  ( 7.265625000614516438, 3.027376345333611329, 5.243569643749999010 ) ) ;
#48200 = EDGE_CURVE ( 'NONE', #9005, #58713, #58581, .T. ) ;
#48201 = CARTESIAN_POINT ( 'NONE',  ( 23.85937500061451644, 4.541064518000418104, -2.621784821874998173 ) ) ;
#48202 = CARTESIAN_POINT ( 'NONE',  ( 6.928125000614516082, -4.541064518000419881, 2.621784821874995952 ) ) ;
#48203 = CARTESIAN_POINT ( 'NONE',  ( 3.487500001229035362, 4.330127018922191873, 2.499999999999999556 ) ) ;
#48204 = CARTESIAN_POINT ( 'NONE',  ( 8.325000001229033941, 2.886751345948129099, -4.999999999999998224 ) ) ;
#48205 = CARTESIAN_POINT ( 'NONE',  ( 22.94062500061451715, 6.054752690667223547, 3.707466751127219781E-16 ) ) ;
#48206 = CARTESIAN_POINT ( 'NONE',  ( 4.243569643749999898, 11.47812500061451679, -30.00000000000000000 ) ) ;
#48207 = CARTESIAN_POINT ( 'NONE',  ( 10.95000000122903394, -2.886751345948125991, -5.000000000000000000 ) ) ;
#48208 = CARTESIAN_POINT ( 'NONE',  ( 19.90312500061451573, 0.000000000000000000, 5.243569643749999010 ) ) ;
#48209 = CARTESIAN_POINT ( 'NONE',  ( 17.09062500061451573, 6.054752690667223547, 3.707466751127219781E-16 ) ) ;
#48210 = CARTESIAN_POINT ( 'NONE',  ( 29.14687500061451075, -2.746126346562642428, -4.756430356249999214 ) ) ;
#48211 = CARTESIAN_POINT ( 'NONE',  ( 17.84999999999999787, 0.000000000000000000, 4.999999999999998224 ) ) ;
#48212 = CARTESIAN_POINT ( 'NONE',  ( 14.96250000122903323, -4.330127018922190985, -2.500000000000001332 ) ) ;
#48213 =( BOUNDED_CURVE ( )  B_SPLINE_CURVE ( 2, ( #10922, #10562, #21268, #5386, #56359, #49365, #61524 ),
 .UNSPECIFIED., .F., .F. ) 
 B_SPLINE_CURVE_WITH_KNOTS ( ( 3, 2, 2, 3 ),
 ( 0.5700000000000000622, 0.5733333333333334725, 0.5766666666666667718, 0.5800000000000000711 ),
 .UNSPECIFIED. ) 
 CURVE ( )  GEOMETRIC_REPRESENTATION_ITEM ( )  RATIONAL_B_SPLINE_CURVE ( ( 0.9999999999999955591, 0.8660254037844431485, 1.000000000000000000, 0.8660254037844387076, 1.000000000000000000, 0.8660254037844342667, 1.000000000000004441 ) ) 
 REPRESENTATION_ITEM ( '' )  );
#48214 = CARTESIAN_POINT ( 'NONE',  ( 9.553125000614517859, 0.000000000000000000, 5.243569643749999010 ) ) ;
#48215 = CARTESIAN_POINT ( 'NONE',  ( 14.35312500061451679, 4.541064518000418104, -2.621784821874998173 ) ) ;
#48216 = CARTESIAN_POINT ( 'NONE',  ( 24.00000000122902932, -2.886751345948125991, -5.000000000000000000 ) ) ;
#48217 = CARTESIAN_POINT ( 'NONE',  ( 21.30937500061451573, 0.000000000000000000, 5.243569643749999010 ) ) ;
#48218 = CARTESIAN_POINT ( 'NONE',  ( 21.64687500061451786, 6.054752690667223547, 3.707466751127219781E-16 ) ) ;
#48219 = CARTESIAN_POINT ( 'NONE',  ( 28.42499999999999716, 6.123233995736764310E-16, -4.999999999999998224 ) ) ;
#48220 = CARTESIAN_POINT ( 'NONE',  ( 7.500000001229034652, 5.773502691896255534, 3.535250795749688894E-16 ) ) ;
#48221 = CARTESIAN_POINT ( 'NONE',  ( 6.796875000614516438, 6.054752690667223547, 3.707466751127219781E-16 ) ) ;
#48222 = CARTESIAN_POINT ( 'NONE',  ( 22.77187500061451786, -6.054752690667223547, -1.112240025338166033E-15 ) ) ;
#48223 =( BOUNDED_SURFACE ( )  B_SPLINE_SURFACE ( 1, 2, ( 
 ( #35551, #63986, #17469, #23377, #46648, #12294, #69188, #34829, #56992, #23014, #58070, #7480, #30008, #52551, #1957, #47012, #69547, #18906, #34102, #56641, #68103, #40029, #6399, #28931, #51467, #870, #25565, #53271, #47371, #54380, #36286, #13368, #20374, #3414, #42557, #13744, #47729, #7845, #58435, #71368, #25934, #48106, #30382, #65449, #19268, #48474, #26300, #59166, #42925, #43300, #69902, #2669, #37009, #25186, #31102, #70268, #58800, #2309, #14841, #19639, #53642, #70629, #65084, #3775, #36644, #48837, #3034, #20004, #8944, #42196, #20743, #14475, #70998, #35910, #59532, #64720, #37381, #30739, #52911, #31475, #54018, #59905, #9310, #31844, #24824, #41822, #64354, #8210, #14104, #8574, #4144, #27404, #21112, #22213, #27042, #55476, #66554, #72830, #10041, #61007, #4513, #38856, #28133, #61371, #10768, #54742, #55839, #66187, #32208, #38483, #5226, #65, #49573, #72459, #4868, #72095, #60629, #10406, #32575, #44407, #21844, #60261, #32938, #66933, #21479, #16302, #33301, #27768, #15934, #50308, #9675, #38108, #5596, #44032, #49934, #44767, #37741, #49208, #67302, #55113, #16660, #39218, #61730, #11131, #33658, #15565, #56203, #50661, #22571, #65821, #15203, #26676, #71742, #43665, #11496, #40296, #62818, #12210, #40658, #6312, #52465, #34739, #29566, #35465, #57268, #11855, #57631, #62457, #29925, #63179, #12573, #6680, #35107, #52103, #51744, #39579, #7037, #34018, #22924, #56907, #56555, #29208, #415, #1508, #28841, #1143, #45839, #24012, #34374, #23654, #51380, #18097, #7397, #46561, #69103, #5949, #18465, #45482, #28482, #17737, #41028, #1872, #782, #46198, #68739, #23291, #39944, #63544, #68376, #12930, #57987, #62102, #45119, #67654, #17020, #51019, #68014, #17386, #47646, #31019, #18822, #69819, #37296, #58715, #19555, #2583, #69464, #7758, #8486, #13654, #53553, #14390, #36197, #70178, #64266, #24741, #25478, #30654, #36927, #3326, #25852, #46926, #65002, #42113, #63897, #64636, #58347, #65363, #47285, #24378, #31392, #59448, #2950, #19185, #8127, #41385, #13287, #9224, #8855, #59082, #35824, #48389, #30294, #53931, #59819, #14022, #70917, #54298, #52826 ),
 ( #53186, #36562, #48024, #70550, #14753, #19925, #31761, #42479, #20288, #2228, #41738, #42842, #25102, #66099, #43578, #9950, #15477, #4426, #65734, #60179, #38021, #37656, #48754, #60544, #43944, #49123, #21025, #20655, #4057, #26954, #32487, #55022, #49481, #26583, #71652, #3690, #71278, #54654, #26215, #43214, #21388, #72013, #15119, #9588, #32120, #54072, #26728, #10099, #36698, #42614, #3833, #65138, #71054, #14529, #3092, #42250, #9727, #37063, #20429, #14896, #31898, #43718, #3468, #66241, #42978, #65509, #48893, #59588, #60684, #37437, #37797, #15619, #59958, #20058, #65878, #70683, #38161, #71423, #20800, #9365, #43355, #60317, #54434, #47791, #15259, #19697, #31157, #9000, #64774, #26354, #8628, #32261, #31532, #54793, #25988, #4200, #48527, #49263, #71796, #21165, #53329, #2727, #25242, #14164, #70321, #53699, #59220, #25621, #48158, #40993, #44459, #39272, #44819, #16352, #27459, #27827, #49990, #11188, #61784, #27094, #72886, #33715, #38907, #56260, #5651, #118, #55892, #28186, #49626, #4924, #46526, #66990, #50359, #10819, #51074, #1472, #67354, #50715, #22623, #44087, #23978, #6004, #72153, #67705, #61426, #5281, #69068, #33354, #16717, #72514, #21532, #18427, #32990, #63509, #66614, #22267, #45174, #17077, #39638, #32628, #21903, #55168, #62156, #11553, #34069, #56609, #28539, #4564, #15990, #38539, #61063, #10460, #55530, #42803, #19149, #58679, #36161, #53149, #70140, #42442, #2548, #25067, #7361, #13251, #31354, #2191, #64598, #19518, #47985, #42076, #14355, #63861, #52790, #8448, #7723, #29890, #13985, #20251, #47610, #36524, #46891, #8089, #36890, #59044, #64964, #30984, #30619, #53517, #35429, #52429, #69782, #70877, #12896, #70513, #41351, #2911, #24705, #25442, #57953, #41703, #59409, #19889, #8817, #53895, #3286, #47249, #64227, #13616, #25814, #18786, #48352, #1835, #35789, #24343, #69429, #58312, #30257, #44278, #72707, #32085, #65325, #38353, #59780, #54986, #27643, #15083, #66433, #61252, #4392, #10646, #60507, #54616, #31721, #21719, #71980, #21353, #55353, #71616, #37985, #49088, #22090, #16181, #43542, #26921, #4022, #54257, #55714, #65696, #5109 ) ),
 .UNSPECIFIED., .F., .F., .F. ) 
 B_SPLINE_SURFACE_WITH_KNOTS ( ( 2, 2 ),
 ( 3, 2, 2, 2, 2, 2, 2, 2, 2, 2, 2, 2, 2, 2, 2, 2, 2, 2, 2, 2, 2, 2, 2, 2, 2, 2, 2, 2, 2, 2, 2, 2, 2, 2, 2, 2, 2, 2, 2, 2, 2, 2, 2, 2, 2, 2, 2, 2, 2, 2, 2, 2, 2, 2, 2, 2, 2, 2, 2, 2, 2, 2, 2, 2, 2, 2, 2, 2, 2, 2, 2, 2, 2, 2, 2, 2, 2, 2, 2, 2, 2, 2, 2, 2, 2, 2, 2, 2, 2, 2, 2, 2, 2, 2, 2, 2, 2, 2, 2, 2, 2, 2, 2, 2, 2, 2, 2, 2, 2, 2, 2, 2, 2, 2, 2, 2, 2, 2, 2, 2, 2, 2, 2, 2, 2, 2, 2, 2, 2, 2, 2, 2, 2, 2, 3 ),
 ( 0.000000000000000000, 1.000000000000000000 ),
 ( 0.000000000000000000, 0.007246376811594202987, 0.01449275362318840597, 0.02173913043478260809, 0.02898550724637681195, 0.03623188405797101580, 0.04347826086956521618, 0.05072463768115942351, 0.05797101449275362389, 0.06521739130434782428, 0.07246376811594203160, 0.07971014492753622505, 0.08695652173913043237, 0.09420289855072463969, 0.1014492753623188470, 0.1086956521739130405, 0.1159420289855072478, 0.1231884057971014551, 0.1304347826086956486, 0.1376811594202898559, 0.1449275362318840632, 0.1521739130434782705, 0.1594202898550724501, 0.1666666666666666574, 0.1739130434782608647, 0.1811594202898550721, 0.1884057971014492794, 0.1956521739130434867, 0.2028985507246376940, 0.2101449275362318736, 0.2173913043478260809, 0.2246376811594202882, 0.2318840579710144956, 0.2391304347826087029, 0.2463768115942029102, 0.2536231884057971175, 0.2608695652173912971, 0.2681159420289855322, 0.2753623188405797118, 0.2826086956521738913, 0.2898550724637681264, 0.2971014492753623060, 0.3043478260869565410, 0.3115942028985507206, 0.3188405797101449002, 0.3260869565217391353, 0.3333333333333333148, 0.3405797101449275499, 0.3478260869565217295, 0.3550724637681159646, 0.3623188405797101441, 0.3695652173913043237, 0.3768115942028985588, 0.3840579710144927383, 0.3913043478260869734, 0.3985507246376811530, 0.4057971014492753881, 0.4130434782608695676, 0.4202898550724637472, 0.4275362318840579823, 0.4347826086956521618, 0.4420289855072463969, 0.4492753623188405765, 0.4565217391304347561, 0.4637681159420289911, 0.4710144927536231707, 0.4782608695652174058, 0.4855072463768115854, 0.4927536231884058204, 0.5000000000000000000, 0.5072463768115942351, 0.5144927536231883591, 0.5217391304347825942, 0.5289855072463768293, 0.5362318840579710644, 0.5434782608695651884, 0.5507246376811594235, 0.5579710144927536586, 0.5652173913043477826, 0.5724637681159420177, 0.5797101449275362528, 0.5869565217391304879, 0.5942028985507246119, 0.6014492753623188470, 0.6086956521739130821, 0.6159420289855072062, 0.6231884057971014412, 0.6304347826086956763, 0.6376811594202898004, 0.6449275362318840354, 0.6521739130434782705, 0.6594202898550725056, 0.6666666666666666297, 0.6739130434782608647, 0.6811594202898550998, 0.6884057971014492239, 0.6956521739130434590, 0.7028985507246376940, 0.7101449275362319291, 0.7173913043478260532, 0.7246376811594202882, 0.7318840579710145233, 0.7391304347826086474, 0.7463768115942028825, 0.7536231884057971175, 0.7608695652173913526, 0.7681159420289854767, 0.7753623188405797118, 0.7826086956521739468, 0.7898550724637680709, 0.7971014492753623060, 0.8043478260869565410, 0.8115942028985507761, 0.8188405797101449002, 0.8260869565217391353, 0.8333333333333333703, 0.8405797101449274944, 0.8478260869565217295, 0.8550724637681159646, 0.8623188405797101996, 0.8695652173913043237, 0.8768115942028985588, 0.8840579710144927938, 0.8913043478260869179, 0.8985507246376811530, 0.9057971014492753881, 0.9130434782608695121, 0.9202898550724637472, 0.9275362318840579823, 0.9347826086956522174, 0.9420289855072463414, 0.9492753623188405765, 0.9565217391304348116, 0.9637681159420289356, 0.9662083017040261623 ),
 .UNSPECIFIED. ) 
 GEOMETRIC_REPRESENTATION_ITEM ( )  RATIONAL_B_SPLINE_SURFACE ( (
 ( 1.000000000000000000, 0.8660254037844387076, 1.000000000000000000, 0.8660254037844387076, 1.000000000000000000, 0.8660254037844387076, 1.000000000000000000, 0.8660254037844387076, 1.000000000000000000, 0.8660254037844387076, 1.000000000000000000, 0.8660254037844387076, 1.000000000000000000, 0.8660254037844387076, 1.000000000000000000, 0.8660254037844387076, 1.000000000000000000, 0.8660254037844387076, 1.000000000000000000, 0.8660254037844387076, 1.000000000000000000, 0.8660254037844387076, 1.000000000000000000, 0.8660254037844387076, 1.000000000000000000, 0.8660254037844387076, 1.000000000000000000, 0.8660254037844387076, 1.000000000000000000, 0.8660254037844387076, 1.000000000000000000, 0.8660254037844387076, 1.000000000000000000, 0.8660254037844387076, 1.000000000000000000, 0.8660254037844387076, 1.000000000000000000, 0.8660254037844387076, 1.000000000000000000, 0.8660254037844387076, 1.000000000000000000, 0.8660254037844387076, 1.000000000000000000, 0.8660254037844387076, 1.000000000000000000, 0.8660254037844387076, 1.000000000000000000, 0.8660254037844387076, 1.000000000000000000, 0.8660254037844387076, 1.000000000000000000, 0.8660254037844387076, 1.000000000000000000, 0.8660254037844387076, 1.000000000000000000, 0.8660254037844387076, 1.000000000000000000, 0.8660254037844387076, 1.000000000000000000, 0.8660254037844387076, 1.000000000000000000, 0.8660254037844387076, 1.000000000000000000, 0.8660254037844387076, 1.000000000000000000, 0.8660254037844387076, 1.000000000000000000, 0.8660254037844387076, 1.000000000000000000, 0.8660254037844387076, 1.000000000000000000, 0.8660254037844387076, 1.000000000000000000, 0.8660254037844387076, 1.000000000000000000, 0.8660254037844387076, 1.000000000000000000, 0.8660254037844387076, 1.000000000000000000, 0.8660254037844387076, 1.000000000000000000, 0.8660254037844387076, 1.000000000000000000, 0.8660254037844387076, 1.000000000000000000, 0.8660254037844387076, 1.000000000000000000, 0.8660254037844387076, 1.000000000000000000, 0.8660254037844387076, 1.000000000000000000, 0.8660254037844387076, 1.000000000000000000, 0.8660254037844387076, 1.000000000000000000, 0.8660254037844387076, 1.000000000000000000, 0.8660254037844387076, 1.000000000000000000, 0.8660254037844387076, 1.000000000000000000, 0.8660254037844387076, 1.000000000000000000, 0.8660254037844387076, 1.000000000000000000, 0.8660254037844387076, 1.000000000000000000, 0.8660254037844387076, 1.000000000000000000, 0.8660254037844387076, 1.000000000000000000, 0.8660254037844387076, 1.000000000000000000, 0.8660254037844387076, 1.000000000000000000, 0.8660254037844387076, 1.000000000000000000, 0.8660254037844387076, 1.000000000000000000, 0.8660254037844387076, 1.000000000000000000, 0.8660254037844387076, 1.000000000000000000, 0.8660254037844387076, 1.000000000000000000, 0.8660254037844387076, 1.000000000000000000, 0.8660254037844387076, 1.000000000000000000, 0.8660254037844387076, 1.000000000000000000, 0.8660254037844387076, 1.000000000000000000, 0.8660254037844387076, 1.000000000000000000, 0.8660254037844387076, 1.000000000000000000, 0.8660254037844387076, 1.000000000000000000, 0.8660254037844387076, 1.000000000000000000, 0.8660254037844387076, 1.000000000000000000, 0.8660254037844387076, 1.000000000000000000, 0.8660254037844387076, 1.000000000000000000, 0.8660254037844387076, 1.000000000000000000, 0.8660254037844387076, 1.000000000000000000, 0.8660254037844387076, 1.000000000000000000, 0.8660254037844387076, 1.000000000000000000, 0.8660254037844387076, 1.000000000000000000, 0.8660254037844387076, 1.000000000000000000, 0.8660254037844387076, 1.000000000000000000, 0.8660254037844387076, 1.000000000000000000, 0.8660254037844387076, 1.000000000000000000, 0.8660254037844387076, 1.000000000000000000, 0.8660254037844387076, 1.000000000000000000, 0.8660254037844387076, 1.000000000000000000, 0.8660254037844387076, 1.000000000000000000, 0.8660254037844387076, 1.000000000000000000, 0.8660254037844387076, 1.000000000000000000, 0.8660254037844387076, 1.000000000000000000, 0.8660254037844387076, 1.000000000000000000, 0.8660254037844387076, 1.000000000000000000, 0.8660254037844387076, 1.000000000000000000, 0.8660254037844387076, 1.000000000000000000, 0.8660254037844387076, 1.000000000000000000, 0.8660254037844387076, 1.000000000000000000, 0.8660254037844387076, 1.000000000000000000, 0.8660254037844387076, 1.000000000000000000, 0.8660254037844387076, 1.000000000000000000, 0.8660254037844387076, 1.000000000000000000, 0.8660254037844387076, 1.000000000000000000, 0.8660254037844387076, 1.000000000000000000, 0.8660254037844387076, 1.000000000000000000, 0.8660254037844387076, 1.000000000000000000, 0.8660254037844387076, 1.000000000000000000, 0.8660254037844387076, 1.000000000000000000, 0.8660254037844387076, 1.000000000000000000, 0.8660254037844387076, 1.000000000000000000, 0.8660254037844387076, 1.000000000000000000, 0.8660254037844387076, 1.000000000000000000, 0.8660254037844387076, 1.000000000000000000, 0.8660254037844387076, 1.000000000000000000, 0.8660254037844387076, 1.000000000000000000, 0.8660254037844387076, 1.000000000000000000, 0.8660254037844387076, 1.000000000000000000, 0.8660254037844387076, 1.000000000000000000, 0.8660254037844387076, 1.000000000000000000, 0.8660254037844387076, 1.000000000000000000, 0.8660254037844387076, 1.000000000000000000, 0.8660254037844387076, 1.000000000000000000, 0.8660254037844387076, 1.000000000000000000, 0.8660254037844387076, 1.000000000000000000, 0.8660254037844387076, 1.000000000000000000, 0.8660254037844387076, 1.000000000000000000, 0.8660254037844387076, 1.000000000000000000, 0.8660254037844387076, 1.000000000000000000, 0.8660254037844387076, 1.000000000000000000, 0.8660254037844387076, 1.000000000000000000, 0.8660254037844387076, 1.000000000000000000, 0.8660254037844387076, 1.000000000000000000, 0.8660254037844387076, 1.000000000000000000, 0.8660254037844387076, 1.000000000000000000, 0.8660254037844387076, 1.000000000000000000, 0.8660254037844387076, 1.000000000000000000, 0.9548846395026737710, 0.9401540804572410259),
 ( 1.000000000000000000, 0.8660254037844387076, 1.000000000000000000, 0.8660254037844387076, 1.000000000000000000, 0.8660254037844387076, 1.000000000000000000, 0.8660254037844387076, 1.000000000000000000, 0.8660254037844387076, 1.000000000000000000, 0.8660254037844387076, 1.000000000000000000, 0.8660254037844387076, 1.000000000000000000, 0.8660254037844387076, 1.000000000000000000, 0.8660254037844387076, 1.000000000000000000, 0.8660254037844387076, 1.000000000000000000, 0.8660254037844387076, 1.000000000000000000, 0.8660254037844387076, 1.000000000000000000, 0.8660254037844387076, 1.000000000000000000, 0.8660254037844387076, 1.000000000000000000, 0.8660254037844387076, 1.000000000000000000, 0.8660254037844387076, 1.000000000000000000, 0.8660254037844387076, 1.000000000000000000, 0.8660254037844387076, 1.000000000000000000, 0.8660254037844387076, 1.000000000000000000, 0.8660254037844387076, 1.000000000000000000, 0.8660254037844387076, 1.000000000000000000, 0.8660254037844387076, 1.000000000000000000, 0.8660254037844387076, 1.000000000000000000, 0.8660254037844387076, 1.000000000000000000, 0.8660254037844387076, 1.000000000000000000, 0.8660254037844387076, 1.000000000000000000, 0.8660254037844387076, 1.000000000000000000, 0.8660254037844387076, 1.000000000000000000, 0.8660254037844387076, 1.000000000000000000, 0.8660254037844387076, 1.000000000000000000, 0.8660254037844387076, 1.000000000000000000, 0.8660254037844387076, 1.000000000000000000, 0.8660254037844387076, 1.000000000000000000, 0.8660254037844387076, 1.000000000000000000, 0.8660254037844387076, 1.000000000000000000, 0.8660254037844387076, 1.000000000000000000, 0.8660254037844387076, 1.000000000000000000, 0.8660254037844387076, 1.000000000000000000, 0.8660254037844387076, 1.000000000000000000, 0.8660254037844387076, 1.000000000000000000, 0.8660254037844387076, 1.000000000000000000, 0.8660254037844387076, 1.000000000000000000, 0.8660254037844387076, 1.000000000000000000, 0.8660254037844387076, 1.000000000000000000, 0.8660254037844387076, 1.000000000000000000, 0.8660254037844387076, 1.000000000000000000, 0.8660254037844387076, 1.000000000000000000, 0.8660254037844387076, 1.000000000000000000, 0.8660254037844387076, 1.000000000000000000, 0.8660254037844387076, 1.000000000000000000, 0.8660254037844387076, 1.000000000000000000, 0.8660254037844387076, 1.000000000000000000, 0.8660254037844387076, 1.000000000000000000, 0.8660254037844387076, 1.000000000000000000, 0.8660254037844387076, 1.000000000000000000, 0.8660254037844387076, 1.000000000000000000, 0.8660254037844387076, 1.000000000000000000, 0.8660254037844387076, 1.000000000000000000, 0.8660254037844387076, 1.000000000000000000, 0.8660254037844387076, 1.000000000000000000, 0.8660254037844387076, 1.000000000000000000, 0.8660254037844387076, 1.000000000000000000, 0.8660254037844387076, 1.000000000000000000, 0.8660254037844387076, 1.000000000000000000, 0.8660254037844387076, 1.000000000000000000, 0.8660254037844387076, 1.000000000000000000, 0.8660254037844387076, 1.000000000000000000, 0.8660254037844387076, 1.000000000000000000, 0.8660254037844387076, 1.000000000000000000, 0.8660254037844387076, 1.000000000000000000, 0.8660254037844387076, 1.000000000000000000, 0.8660254037844387076, 1.000000000000000000, 0.8660254037844387076, 1.000000000000000000, 0.8660254037844387076, 1.000000000000000000, 0.8660254037844387076, 1.000000000000000000, 0.8660254037844387076, 1.000000000000000000, 0.8660254037844387076, 1.000000000000000000, 0.8660254037844387076, 1.000000000000000000, 0.8660254037844387076, 1.000000000000000000, 0.8660254037844387076, 1.000000000000000000, 0.8660254037844387076, 1.000000000000000000, 0.8660254037844387076, 1.000000000000000000, 0.8660254037844387076, 1.000000000000000000, 0.8660254037844387076, 1.000000000000000000, 0.8660254037844387076, 1.000000000000000000, 0.8660254037844387076, 1.000000000000000000, 0.8660254037844387076, 1.000000000000000000, 0.8660254037844387076, 1.000000000000000000, 0.8660254037844387076, 1.000000000000000000, 0.8660254037844387076, 1.000000000000000000, 0.8660254037844387076, 1.000000000000000000, 0.8660254037844387076, 1.000000000000000000, 0.8660254037844387076, 1.000000000000000000, 0.8660254037844387076, 1.000000000000000000, 0.8660254037844387076, 1.000000000000000000, 0.8660254037844387076, 1.000000000000000000, 0.8660254037844387076, 1.000000000000000000, 0.8660254037844387076, 1.000000000000000000, 0.8660254037844387076, 1.000000000000000000, 0.8660254037844387076, 1.000000000000000000, 0.8660254037844387076, 1.000000000000000000, 0.8660254037844387076, 1.000000000000000000, 0.8660254037844387076, 1.000000000000000000, 0.8660254037844387076, 1.000000000000000000, 0.8660254037844387076, 1.000000000000000000, 0.8660254037844387076, 1.000000000000000000, 0.8660254037844387076, 1.000000000000000000, 0.8660254037844387076, 1.000000000000000000, 0.8660254037844387076, 1.000000000000000000, 0.8660254037844387076, 1.000000000000000000, 0.8660254037844387076, 1.000000000000000000, 0.8660254037844387076, 1.000000000000000000, 0.8660254037844387076, 1.000000000000000000, 0.8660254037844387076, 1.000000000000000000, 0.8660254037844387076, 1.000000000000000000, 0.8660254037844387076, 1.000000000000000000, 0.8660254037844387076, 1.000000000000000000, 0.8660254037844387076, 1.000000000000000000, 0.8660254037844387076, 1.000000000000000000, 0.8660254037844387076, 1.000000000000000000, 0.8660254037844387076, 1.000000000000000000, 0.8660254037844387076, 1.000000000000000000, 0.8660254037844387076, 1.000000000000000000, 0.8660254037844387076, 1.000000000000000000, 0.8660254037844387076, 1.000000000000000000, 0.8660254037844387076, 1.000000000000000000, 0.8660254037844387076, 1.000000000000000000, 0.8660254037844387076, 1.000000000000000000, 0.8660254037844387076, 1.000000000000000000, 0.8660254037844387076, 1.000000000000000000, 0.8660254037844387076, 1.000000000000000000, 0.8660254037844387076, 1.000000000000000000, 0.8660254037844387076, 1.000000000000000000, 0.9548846395026737710, 0.9401540804572410259) ) ) 
 REPRESENTATION_ITEM ( '' )  SURFACE ( )  );
#48224 = CARTESIAN_POINT ( 'NONE',  ( 4.505505391250587799, 2.168045472173443233, -4.697296768249695553 ) ) ;
#48225 = CARTESIAN_POINT ( 'NONE',  ( 18.17812500061451786, -4.541064518000419881, 2.621784821874995952 ) ) ;
#48226 = CARTESIAN_POINT ( 'NONE',  ( 24.83437500061451431, 4.541064518000418104, 2.621784821874999949 ) ) ;
#48227 = CARTESIAN_POINT ( 'NONE',  ( -1.878215178125001827, 20.70312499938548001, 33.25316411605952283 ) ) ;
#48228 = CARTESIAN_POINT ( 'NONE',  ( -1.071796769724475906, 11.02009619066136636, -34.00000000000000711 ) ) ;
#48229 = FACE_OUTER_BOUND ( 'NONE', #55691, .T. ) ;
#48230 = CARTESIAN_POINT ( 'NONE',  ( 5.821875000614519458, 3.027376345333613106, -5.243569643749998122 ) ) ;
#48231 = CARTESIAN_POINT ( 'NONE',  ( 16.79062500061451857, -3.027376345333614438, 5.243569643749998122 ) ) ;
#48232 = EDGE_LOOP ( 'NONE', ( #27292, #6551, #35022, #66552, #68975, #46842, #60912, #10780, #66987, #26083, #41958, #44311, #24294, #64352, #35676, #31092, #34966, #68431, #15453, #20423, #72093, #68054, #16345, #70605, #37739, #20056, #4501, #55252, #4299, #46778, #32926, #1506, #57805, #24295, #18271, #202, #15434, #11748, #29463, #43118 ) ) ;
#48233 = FACE_OUTER_BOUND ( 'NONE', #6572, .T. ) ;
#48234 = CARTESIAN_POINT ( 'NONE',  ( 24.29062500061451502, 6.054752690667223547, 3.707466751127219781E-16 ) ) ;
#48235 = CARTESIAN_POINT ( 'NONE',  ( -5.810221930991193690E-16, 10.55000000122903359, -34.00000000000000000 ) ) ;
#48236 = CARTESIAN_POINT ( 'NONE',  ( 27.97500000000000142, 6.123233995736764310E-16, -4.999999999999998224 ) ) ;
#48237 = CARTESIAN_POINT ( 'NONE',  ( 15.78749999999999964, -2.886751345948125991, -5.000000000000000000 ) ) ;
#48238 = CARTESIAN_POINT ( 'NONE',  ( 24.15000000122903145, 5.773502691896255534, 3.535250795749688894E-16 ) ) ;
#48239 = CARTESIAN_POINT ( 'NONE',  ( 19.60312500061451502, -4.541064518000417216, -2.621784821875001281 ) ) ;
#48240 = VERTEX_POINT ( 'NONE', #17115 ) ;
#48241 = CARTESIAN_POINT ( 'NONE',  ( 22.61250000000000071, 2.886751345948129099, -4.999999999999998224 ) ) ;
#48242 = EDGE_CURVE ( 'NONE', #27263, #65514, #12859, .T. ) ;
#48243 = CARTESIAN_POINT ( 'NONE',  ( 24.30937500061451573, 4.541064518000418104, -2.621784821874998173 ) ) ;
#48244 = ORIENTED_EDGE ( 'NONE', *, *, #20472, .F. ) ;
#48245 = CARTESIAN_POINT ( 'NONE',  ( 11.70000000000000284, -4.330127018922190985, -2.500000000000001332 ) ) ;
#48246 = CARTESIAN_POINT ( 'NONE',  ( 12.17812500061451608, 4.541064518000418104, 2.621784821874999949 ) ) ;
#48247 = CARTESIAN_POINT ( 'NONE',  ( 3.590625000614518836, 6.054752690667223547, 3.707466751127219781E-16 ) ) ;
#48248 = CARTESIAN_POINT ( 'NONE',  ( 16.32187500061451502, -4.119189519843968306, 2.378215178124996054 ) ) ;
#48249 = CARTESIAN_POINT ( 'NONE',  ( 25.79062500061451502, -3.027376345333614438, 5.243569643749998122 ) ) ;
#48250 =( BOUNDED_CURVE ( )  B_SPLINE_CURVE ( 2, ( #35941, #30038, #10974, #1985, #7151, #69574, #52217 ),
 .UNSPECIFIED., .F., .F. ) 
 B_SPLINE_CURVE_WITH_KNOTS ( ( 3, 2, 2, 3 ),
 ( 0.9343140676420280677, 0.9361111111111111160, 0.9388888888888888840, 0.9404862704844845211 ),
 .UNSPECIFIED. ) 
 CURVE ( )  GEOMETRIC_REPRESENTATION_ITEM ( )  RATIONAL_B_SPLINE_CURVE ( ( 0.9387977477080564626, 0.9133270576652030570, 1.000000000000000000, 0.8660254037844387076, 1.000000000000000000, 0.9229569204620456935, 0.9345222229958878302 ) ) 
 REPRESENTATION_ITEM ( '' )  );
#48251 = CARTESIAN_POINT ( 'NONE',  ( 13.23750000122903359, 6.123233995736764310E-16, -4.999999999999998224 ) ) ;
#48252 = CARTESIAN_POINT ( 'NONE',  ( 19.72499999999999787, -4.330127018922194537, 2.499999999999995559 ) ) ;
#48253 = CARTESIAN_POINT ( 'NONE',  ( 27.03750000000000142, -2.886751345948125991, -5.000000000000000000 ) ) ;
#48254 = CARTESIAN_POINT ( 'NONE',  ( 2.859375000614519546, 0.000000000000000000, 5.243569643749999010 ) ) ;
#48255 = CARTESIAN_POINT ( 'NONE',  ( 6.384375000614516793, 4.541064518000418104, 2.621784821874999949 ) ) ;
#48256 = CARTESIAN_POINT ( 'NONE',  ( 16.17187500061451644, 3.027376345333613106, -5.243569643749998122 ) ) ;
#48257 = CARTESIAN_POINT ( 'NONE',  ( 29.82187500061451502, 3.027376345333611329, 5.243569643749999010 ) ) ;
#48258 = VERTEX_POINT ( 'NONE', #5685 ) ;
#48259 = CARTESIAN_POINT ( 'NONE',  ( 26.61562500061451786, 3.027376345333611329, 5.243569643749999010 ) ) ;
#48260 = CARTESIAN_POINT ( 'NONE',  ( 28.84687500061452070, 6.054752690667223547, 3.707466751127219781E-16 ) ) ;
#48261 = CARTESIAN_POINT ( 'NONE',  ( -1.071796769724490339, 14.82634618820330097, 26.00000000000000000 ) ) ;
#48262 = CARTESIAN_POINT ( 'NONE',  ( 17.17500000000000071, 6.123233995736764310E-16, -4.999999999999998224 ) ) ;
#48263 = CARTESIAN_POINT ( 'NONE',  ( 14.39062500061451821, 6.054752690667223547, 3.707466751127219781E-16 ) ) ;
#48264 = CARTESIAN_POINT ( 'NONE',  ( -1.626862140677534273E-15, 19.58750000000000213, 34.00000000000000000 ) ) ;
#48265 = CARTESIAN_POINT ( 'NONE',  ( 14.10000000000000142, 4.330127018922192761, -2.499999999999997780 ) ) ;
#48266 = CARTESIAN_POINT ( 'NONE',  ( 29.01562500061451644, -6.054752690667223547, -1.112240025338166033E-15 ) ) ;
#48267 = CARTESIAN_POINT ( 'NONE',  ( 18.86250000122903359, 0.000000000000000000, 4.999999999999998224 ) ) ;
#48268 = CARTESIAN_POINT ( 'NONE',  ( 0.000000000000000000, 20.00000000000000000, 26.00000000000000000 ) ) ;
#48269 = CARTESIAN_POINT ( 'NONE',  ( 18.42187500061451644, 2.746126346562645981, -4.756430356249997438 ) ) ;
#48270 = CARTESIAN_POINT ( 'NONE',  ( 5.315625000614516260, 3.027376345333613106, -5.243569643749998122 ) ) ;
#48271 = CARTESIAN_POINT ( 'NONE',  ( 25.20937500061451431, 4.541064518000418104, -2.621784821874998173 ) ) ;
#48272 = CARTESIAN_POINT ( 'NONE',  ( 2.121784821875001281, 16.40937500061452070, 33.67503911421598417 ) ) ;
#48273 = CARTESIAN_POINT ( 'NONE',  ( 24.94687500061451502, -3.027376345333614438, 5.243569643749998122 ) ) ;
#48274 = CARTESIAN_POINT ( 'NONE',  ( 5.924999999999999822, 6.123233995736764310E-16, -4.999999999999998224 ) ) ;
#48275 = CARTESIAN_POINT ( 'NONE',  ( 3.999999999999999112, 11.78750000122903430, 30.00000000000000000 ) ) ;
#48276 = CARTESIAN_POINT ( 'NONE',  ( 13.34062500061451750, -3.027376345333610441, -5.243569643749999898 ) ) ;
#48277 = CARTESIAN_POINT ( 'NONE',  ( 5.062500001229035540, -4.330127018922190985, -2.500000000000001332 ) ) ;
#48278 = CARTESIAN_POINT ( 'NONE',  ( 9.046875000614518214, 6.054752690667223547, 3.707466751127219781E-16 ) ) ;
#48279 = CARTESIAN_POINT ( 'NONE',  ( -0.2761983717765570945, 4.994289515549795055, -26.00713100841934633 ) ) ;
#48280 = ORIENTED_EDGE ( 'NONE', *, *, #47837, .F. ) ;
#48281 = CARTESIAN_POINT ( 'NONE',  ( 11.12812500061451715, 6.421520780324663323E-16, -5.243569643749999010 ) ) ;
#48282 = CARTESIAN_POINT ( 'NONE',  ( 13.54687500061451999, 6.054752690667223547, 3.707466751127219781E-16 ) ) ;
#48283 = CARTESIAN_POINT ( 'NONE',  ( 3.999999999999999112, 12.23750000122903359, -30.00000000000000000 ) ) ;
#48284 = CARTESIAN_POINT ( 'NONE',  ( 21.71250000122903501, -4.330127018922190985, -2.500000000000001332 ) ) ;
#48285 = CARTESIAN_POINT ( 'NONE',  ( 10.65937500061451715, -4.541064518000417216, -2.621784821875001281 ) ) ;
#48286 = CARTESIAN_POINT ( 'NONE',  ( 13.30312500061451786, -4.541064518000417216, -2.621784821875001281 ) ) ;
#48287 = CARTESIAN_POINT ( 'NONE',  ( 28.63125000122903074, 4.330127018922191873, 2.499999999999999556 ) ) ;
#48288 = CARTESIAN_POINT ( 'NONE',  ( 21.19687500061451502, 6.054752690667223547, 3.707466751127219781E-16 ) ) ;
#48289 = CARTESIAN_POINT ( 'NONE',  ( 15.59999999999999964, 0.000000000000000000, 4.999999999999998224 ) ) ;
#48290 = CARTESIAN_POINT ( 'NONE',  ( -3.462385672708550910, 3.612013013662438432, 27.98145868590390606 ) ) ;
#48291 = CARTESIAN_POINT ( 'NONE',  ( -3.000416591977282496E-16, 13.44687500061451679, -34.90005215228797653 ) ) ;
#48292 = CARTESIAN_POINT ( 'NONE',  ( 16.54687500061451644, -3.027376345333610441, -5.243569643749999898 ) ) ;
#48293 = CARTESIAN_POINT ( 'NONE',  ( 14.73750000122903359, 4.330127018922191873, 2.499999999999999556 ) ) ;
#48294 = CARTESIAN_POINT ( 'NONE',  ( 12.72187500061451537, 3.027376345333611329, 5.243569643749999010 ) ) ;
#48295 = CARTESIAN_POINT ( 'NONE',  ( -2.121784821874996840, 17.17812500061451786, -26.32496088578401583 ) ) ;
#48296 = CARTESIAN_POINT ( 'NONE',  ( 17.32500000122903216, 2.886751345948129099, -4.999999999999998224 ) ) ;
#48297 = CARTESIAN_POINT ( 'NONE',  ( 12.62812500061451537, 4.541064518000418104, 2.621784821874999949 ) ) ;
#48298 = VERTEX_POINT ( 'NONE', #23382 ) ;
#48299 = CARTESIAN_POINT ( 'NONE',  ( 16.94999999999999929, 0.000000000000000000, 4.999999999999998224 ) ) ;
#48300 = CARTESIAN_POINT ( 'NONE',  ( -2.000000000000000000, 17.33750000122903145, -33.46410161513775705 ) ) ;
#48301 = CARTESIAN_POINT ( 'NONE',  ( 10.69687500061451679, -3.027376345333610441, -5.243569643749999898 ) ) ;
#48302 = CARTESIAN_POINT ( 'NONE',  ( 4.648177544792955741E-15, 13.73749999999999716, 33.99999999999999289 ) ) ;
#48303 = EDGE_CURVE ( 'NONE', #59817, #18738, #593, .T. ) ;
#48304 = CARTESIAN_POINT ( 'NONE',  ( 13.23750000122903359, 6.123233995736764310E-16, -4.999999999999998224 ) ) ;
#48305 = CARTESIAN_POINT ( 'NONE',  ( 21.97500000122903074, 2.886751345948126879, 4.999999999999999112 ) ) ;
#48306 = EDGE_CURVE ( 'NONE', #27766, #829, #18910, .T. ) ;
#48307 = CARTESIAN_POINT ( 'NONE',  ( 18.59062500061451573, -3.027376345333614438, 5.243569643749998122 ) ) ;
#48308 = CARTESIAN_POINT ( 'NONE',  ( 20.61562500061451431, 3.027376345333613106, -5.243569643749998122 ) ) ;
#48309 = CARTESIAN_POINT ( 'NONE',  ( 26.77500000122903145, 2.886751345948129099, -4.999999999999998224 ) ) ;
#48310 = CARTESIAN_POINT ( 'NONE',  ( 3.890625000614517326, -3.027376345333610441, -5.243569643749999898 ) ) ;
#48311 = CARTESIAN_POINT ( 'NONE',  ( 25.91250000000000142, 2.886751345948126879, 4.999999999999999112 ) ) ;
#48312 = DIRECTION ( 'NONE',  ( 0.000000000000000000, 0.000000000000000000, 1.000000000000000000 ) ) ;
#48313 = CARTESIAN_POINT ( 'NONE',  ( 29.47499999999999787, 4.330127018922191873, 2.499999999999999556 ) ) ;
#48314 = CARTESIAN_POINT ( 'NONE',  ( 27.30937500061451573, -4.541064518000417216, -2.621784821875001281 ) ) ;
#48315 = CARTESIAN_POINT ( 'NONE',  ( 26.60625000122903216, -4.330127018922190985, -2.500000000000001332 ) ) ;
#48316 = CARTESIAN_POINT ( 'NONE',  ( 2.121784821874999061, 14.30937500061451750, -33.67503911421598417 ) ) ;
#48317 = CARTESIAN_POINT ( 'NONE',  ( 3.937500001229034208, 4.330127018922191873, 2.499999999999999556 ) ) ;
#48318 = CARTESIAN_POINT ( 'NONE',  ( 29.82187500061451502, 3.027376345333611329, 5.243569643749999010 ) ) ;
#48319 = CARTESIAN_POINT ( 'NONE',  ( 16.35000000000000142, 4.330127018922192761, -2.499999999999997780 ) ) ;
#48320 = CARTESIAN_POINT ( 'NONE',  ( 7.921875000614517326, -6.054752690667223547, -1.112240025338166033E-15 ) ) ;
#48321 = CARTESIAN_POINT ( 'NONE',  ( 26.16562500061451502, 3.027376345333611329, 5.243569643749999010 ) ) ;
#48322 = CARTESIAN_POINT ( 'NONE',  ( 9.131250001229034297, 6.123233995736764310E-16, -4.999999999999998224 ) ) ;
#48323 = CARTESIAN_POINT ( 'NONE',  ( 14.32500000000000107, -4.330127018922194537, 2.499999999999995559 ) ) ;
#48324 = CARTESIAN_POINT ( 'NONE',  ( 4.000000000000000000, 17.60000000122903430, -27.69059892324149885 ) ) ;
#48325 = CARTESIAN_POINT ( 'NONE',  ( 6.346875000614517148, 6.054752690667223547, 3.707466751127219781E-16 ) ) ;
#48326 = CARTESIAN_POINT ( 'NONE',  ( 9.196875000614518569, -3.027376345333614438, 5.243569643749998122 ) ) ;
#48327 = CARTESIAN_POINT ( 'NONE',  ( 3.300000000000000711, 4.330127018922192761, -2.499999999999997780 ) ) ;
#48328 = ADVANCED_FACE ( 'NONE', ( #45931 ), #52555, .F. ) ;
#48329 = CARTESIAN_POINT ( 'NONE',  ( 4.243569643749999898, 12.79062500061459495, 32.45002607614398471 ) ) ;
#48330 = CARTESIAN_POINT ( 'NONE',  ( 28.53749999999999787, 5.773502691896255534, 3.535250795749688894E-16 ) ) ;
#48331 = CARTESIAN_POINT ( 'NONE',  ( 3.075000000000001510, -4.330127018922194537, 2.499999999999995559 ) ) ;
#48332 = CARTESIAN_POINT ( 'NONE',  ( 15.60937500061451644, 2.746126346562645981, -4.756430356249997438 ) ) ;
#48333 = VERTEX_POINT ( 'NONE', #41117 ) ;
#48334 = CARTESIAN_POINT ( 'NONE',  ( 19.60312500061451502, -4.541064518000417216, -2.621784821875001281 ) ) ;
#48335 = CARTESIAN_POINT ( 'NONE',  ( 11.12812500061451715, 6.421520780324663323E-16, -5.243569643749999010 ) ) ;
#48336 = CARTESIAN_POINT ( 'NONE',  ( 23.89687500061451431, 0.000000000000000000, 4.756430356249998326 ) ) ;
#48337 = CARTESIAN_POINT ( 'NONE',  ( 7.846875000614518036, -3.027376345333614438, 5.243569643749998122 ) ) ;
#48338 = CARTESIAN_POINT ( 'NONE',  ( 25.50000000000000000, 0.000000000000000000, 4.999999999999998224 ) ) ;
#48339 = CARTESIAN_POINT ( 'NONE',  ( 20.28750000122903074, -4.330127018922194537, 2.499999999999995559 ) ) ;
#48340 = CARTESIAN_POINT ( 'NONE',  ( 27.25312500061451360, -4.541064518000417216, -2.621784821875001281 ) ) ;
#48341 = DIRECTION ( 'NONE',  ( 0.000000000000000000, 0.000000000000000000, 1.000000000000000000 ) ) ;
#48342 = CARTESIAN_POINT ( 'NONE',  ( 9.084375000614517859, 4.541064518000418104, 2.621784821874999949 ) ) ;
#48343 = CARTESIAN_POINT ( 'NONE',  ( 13.80937500061451750, -4.541064518000417216, -2.621784821875001281 ) ) ;
#48344 = CARTESIAN_POINT ( 'NONE',  ( 25.17187500061451644, 3.027376345333613106, -5.243569643749998122 ) ) ;
#48345 = CARTESIAN_POINT ( 'NONE',  ( 8.550000001229030033, -2.886751345948063374, 5.000000000000112799 ) ) ;
#48346 = CARTESIAN_POINT ( 'NONE',  ( 14.21249999999999858, 2.886751345948126879, 4.999999999999999112 ) ) ;
#48347 = CARTESIAN_POINT ( 'NONE',  ( 20.48437500061451289, -4.541064518000419881, 2.621784821874995952 ) ) ;
#48348 = CARTESIAN_POINT ( 'NONE',  ( 9.196875000614518569, -3.027376345333614438, 5.243569643749998122 ) ) ;
#48349 = CARTESIAN_POINT ( 'NONE',  ( -3.756430356250000102, 12.86562499938548321, 30.00000000000000000 ) ) ;
#48350 = CARTESIAN_POINT ( 'NONE',  ( 24.18750000000000355, -2.886751345948129988, 4.999999999999997335 ) ) ;
#48351 = CARTESIAN_POINT ( 'NONE',  ( -3.999999999999999556, 15.83750000000000036, 27.69059892324149175 ) ) ;
#48352 = CARTESIAN_POINT ( 'NONE',  ( -2.121784821874999949, 11.23437500061451821, -33.67503911421598417 ) ) ;
#48353 = CARTESIAN_POINT ( 'NONE',  ( 25.02187500061451431, -5.492252693125287522, -1.008910452111647106E-15 ) ) ;
#48354 = CARTESIAN_POINT ( 'NONE',  ( 13.82812500061451466, 6.421520780324663323E-16, -5.243569643749999010 ) ) ;
#48355 = CARTESIAN_POINT ( 'NONE',  ( 4.162499999999999645, 2.886751345948129099, -4.999999999999998224 ) ) ;
#48356 = CARTESIAN_POINT ( 'NONE',  ( 1.510657702057710734E-15, 19.10000000122903430, -33.99999999999999289 ) ) ;
#48357 = CYLINDRICAL_SURFACE ( 'NONE', #68029, 4.999999999999998224 ) ;
#48358 = CARTESIAN_POINT ( 'NONE',  ( 13.19999999999999929, 4.330127018922192761, -2.499999999999997780 ) ) ;
#48359 = CARTESIAN_POINT ( 'NONE',  ( 4.000000000000000000, 17.60000000122903785, 32.30940107675849049 ) ) ;
#48360 = CARTESIAN_POINT ( 'NONE',  ( 10.61250000122903536, 4.330127018922192761, -2.499999999999997780 ) ) ;
#48361 = CARTESIAN_POINT ( 'NONE',  ( 23.10937500061451644, 0.000000000000000000, 5.243569643749999010 ) ) ;
#48362 = CARTESIAN_POINT ( 'NONE',  ( 16.39687500061451786, -3.027376345333614438, 5.243569643749998122 ) ) ;
#48363 = CARTESIAN_POINT ( 'NONE',  ( 20.36250000122903359, -4.330127018922190985, -2.500000000000001332 ) ) ;
#48364 = ORIENTED_EDGE ( 'NONE', *, *, #26290, .F. ) ;
#48365 = CARTESIAN_POINT ( 'NONE',  ( 18.32812500061451644, 6.421520780324663323E-16, -5.243569643749999010 ) ) ;
#48366 = CARTESIAN_POINT ( 'NONE',  ( 5.390625000614518214, 6.054752690667223547, 3.707466751127219781E-16 ) ) ;
#48367 = CARTESIAN_POINT ( 'NONE',  ( 17.03437500061451715, 6.421520780324663323E-16, -5.243569643749999010 ) ) ;
#48368 = CARTESIAN_POINT ( 'NONE',  ( 28.84687500061452070, 6.054752690667223547, 3.707466751127219781E-16 ) ) ;
#48369 = CARTESIAN_POINT ( 'NONE',  ( 5.465625000614517504, 3.027376345333611329, 5.243569643749999010 ) ) ;
#48370 = CARTESIAN_POINT ( 'NONE',  ( 18.92812500061451431, 4.541064518000418104, 2.621784821874999949 ) ) ;
#48371 = CARTESIAN_POINT ( 'NONE',  ( -2.121784821874999949, 13.87812500061451715, 26.32496088578401938 ) ) ;
#48372 = CARTESIAN_POINT ( 'NONE',  ( 17.66250000122903430, -4.330127018922190985, -2.500000000000001332 ) ) ;
#48373 = CARTESIAN_POINT ( 'NONE',  ( 11.37187500061451928, 2.746126346562643317, 4.756430356249998326 ) ) ;
#48374 = CARTESIAN_POINT ( 'NONE',  ( 7.828125000614517326, -4.541064518000419881, 2.621784821874995952 ) ) ;
#48375 = CARTESIAN_POINT ( 'NONE',  ( 28.07812500061451289, -4.541064518000419881, 2.621784821874995952 ) ) ;
#48376 = CARTESIAN_POINT ( 'NONE',  ( 9.862500001229033586, 0.000000000000000000, 4.999999999999998224 ) ) ;
#48377 = CARTESIAN_POINT ( 'NONE',  ( 23.78437500061451360, 6.421520780324663323E-16, -5.243569643749999010 ) ) ;
#48378 = CARTESIAN_POINT ( 'NONE',  ( 14.20312500061451644, -4.541064518000417216, -2.621784821875001281 ) ) ;
#48379 = CARTESIAN_POINT ( 'NONE',  ( 24.22500000122903430, 2.886751345948126879, 4.999999999999999112 ) ) ;
#48380 = CARTESIAN_POINT ( 'NONE',  ( 22.64062500061451644, -3.027376345333614438, 5.243569643749998122 ) ) ;
#48381 = CARTESIAN_POINT ( 'NONE',  ( 19.58437500061451786, -4.541064518000419881, 2.621784821874995952 ) ) ;
#48382 = CARTESIAN_POINT ( 'NONE',  ( 15.21562500061451750, 3.027376345333613106, -5.243569643749998122 ) ) ;
#48383 = CARTESIAN_POINT ( 'NONE',  ( -4.243569643749999898, 13.97187500061451715, 27.54997392385601529 ) ) ;
#48384 = CARTESIAN_POINT ( 'NONE',  ( 19.94062500061451715, -3.027376345333614438, 5.243569643749998122 ) ) ;
#48385 = CARTESIAN_POINT ( 'NONE',  ( -1.999999999999999112, 17.60000000000000142, 26.53589838486224650 ) ) ;
#48386 = ORIENTED_EDGE ( 'NONE', *, *, #38051, .T. ) ;
#48387 = ORIENTED_EDGE ( 'NONE', *, *, #3037, .F. ) ;
#48388 = CARTESIAN_POINT ( 'NONE',  ( 22.57499999999999929, 6.123233995736764310E-16, -4.999999999999998224 ) ) ;
#48389 = CARTESIAN_POINT ( 'NONE',  ( 8.484601909799253346E-16, 10.21250000000000213, -25.38119784648299770 ) ) ;
#48390 = CARTESIAN_POINT ( 'NONE',  ( 12.59999999999999964, -4.330127018922190985, -2.500000000000001332 ) ) ;
#48391 = CARTESIAN_POINT ( 'NONE',  ( 26.54062500061451146, 6.054752690667223547, 3.707466751127219781E-16 ) ) ;
#48392 = CARTESIAN_POINT ( 'NONE',  ( 7.115625000614516082, 3.027376345333613106, -5.243569643749998122 ) ) ;
#48393 = CARTESIAN_POINT ( 'NONE',  ( 19.05000000122903359, -2.886751345948125991, -5.000000000000000000 ) ) ;
#48394 = CARTESIAN_POINT ( 'NONE',  ( 24.40312500061451573, 0.000000000000000000, 5.243569643749999010 ) ) ;
#48395 = CARTESIAN_POINT ( 'NONE',  ( 22.98749999999999716, -2.886751345948125991, -5.000000000000000000 ) ) ;
#48396 =( BOUNDED_CURVE ( )  B_SPLINE_CURVE ( 2, ( #55236, #16781, #33416, #61851, #5713, #62223, #55595 ),
 .UNSPECIFIED., .F., .F. ) 
 B_SPLINE_CURVE_WITH_KNOTS ( ( 3, 2, 2, 3 ),
 ( 0.1166666666666666824, 0.1194444444444444642, 0.1222222222222222182, 0.1250000000000000000 ),
 .UNSPECIFIED. ) 
 CURVE ( )  GEOMETRIC_REPRESENTATION_ITEM ( )  RATIONAL_B_SPLINE_CURVE ( ( 0.9999999999999993339, 0.8660254037844393737, 1.000000000000000000, 0.8660254037844387076, 1.000000000000000000, 0.8660254037844387076, 1.000000000000000000 ) ) 
 REPRESENTATION_ITEM ( '' )  );
#48397 = EDGE_CURVE ( 'NONE', #3838, #38197, #60977, .T. ) ;
#48398 = CARTESIAN_POINT ( 'NONE',  ( 27.70312500061451289, -4.541064518000417216, -2.621784821875001281 ) ) ;
#48399 = CARTESIAN_POINT ( 'NONE',  ( 8.840625000614515727, -3.027376345333610441, -5.243569643749999898 ) ) ;
#48400 = ORIENTED_EDGE ( 'NONE', *, *, #45339, .F. ) ;
#48401 = CARTESIAN_POINT ( 'NONE',  ( 22.41562500061451502, 3.027376345333613106, -5.243569643749998122 ) ) ;
#48402 = CARTESIAN_POINT ( 'NONE',  ( 6.215625000614517504, 3.027376345333613106, -5.243569643749998122 ) ) ;
#48403 = CARTESIAN_POINT ( 'NONE',  ( 12.98437500061451821, 5.824947211148865298E-16, -4.756430356249998326 ) ) ;
#48404 = CARTESIAN_POINT ( 'NONE',  ( 3.853125000614517681, -4.541064518000417216, -2.621784821875001281 ) ) ;
#48405 = VECTOR ( 'NONE', #5712, 1000.000000000000000 ) ;
#48406 = CARTESIAN_POINT ( 'NONE',  ( 8.484601909799253346E-16, 13.02500000122903501, -25.38119784648299770 ) ) ;
#48407 = CARTESIAN_POINT ( 'NONE',  ( -1.999999999999997113, 13.77500000000000036, -26.53589838486224295 ) ) ;
#48408 = CARTESIAN_POINT ( 'NONE',  ( 11.70000000000000284, -4.330127018922190985, -2.500000000000001332 ) ) ;
#48409 = CARTESIAN_POINT ( 'NONE',  ( 10.20937500061451786, -4.541064518000417216, -2.621784821875001281 ) ) ;
#48410 = CARTESIAN_POINT ( 'NONE',  ( 7.987500001229032698, 4.330127018922191873, 2.499999999999999556 ) ) ;
#48411 = CARTESIAN_POINT ( 'NONE',  ( 14.44687500061451679, 6.054752690667223547, 3.707466751127219781E-16 ) ) ;
#48412 = CARTESIAN_POINT ( 'NONE',  ( 14.40000000000000036, -4.330127018922190985, -2.500000000000001332 ) ) ;
#48413 = CARTESIAN_POINT ( 'NONE',  ( 5.709375000614517859, -4.541064518000417216, -2.621784821875001281 ) ) ;
#48414 = CARTESIAN_POINT ( 'NONE',  ( 1.071796769724488119, 18.33259618943233704, 33.99999999999999289 ) ) ;
#48415 = CARTESIAN_POINT ( 'NONE',  ( 12.15937500061451892, 4.541064518000418104, -2.621784821874998173 ) ) ;
#48416 = DIRECTION ( 'NONE',  ( 0.000000000000000000, 1.000000000000000000, -8.673617379884036705E-17 ) ) ;
#48417 = CARTESIAN_POINT ( 'NONE',  ( 21.74062500061451431, -3.027376345333614438, 5.243569643749998122 ) ) ;
#48418 = CARTESIAN_POINT ( 'NONE',  ( -4.243569643749999898, 9.921875000614516438, 27.54997392385601529 ) ) ;
#48419 = FACE_OUTER_BOUND ( 'NONE', #51155, .T. ) ;
#48420 = CARTESIAN_POINT ( 'NONE',  ( 25.80937500061451928, 0.000000000000000000, 5.243569643749999010 ) ) ;
#48421 = CARTESIAN_POINT ( 'NONE',  ( 4.129838550988103485, 2.818587153659042777, -4.208548528382372034 ) ) ;
#48422 = EDGE_CURVE ( 'NONE', #43273, #69475, #68462, .T. ) ;
#48423 = CARTESIAN_POINT ( 'NONE',  ( 5.503125000614516260, 0.000000000000000000, 5.243569643749999010 ) ) ;
#48424 = CARTESIAN_POINT ( 'NONE',  ( 22.77187500061451431, 5.824947211148865298E-16, -4.756430356249998326 ) ) ;
#48425 = CARTESIAN_POINT ( 'NONE',  ( 17.40937500061451715, -4.541064518000417216, -2.621784821875001281 ) ) ;
#48426 = CARTESIAN_POINT ( 'NONE',  ( 9.084375000614516082, -2.746126346562646425, 4.756430356249996549 ) ) ;
#48427 = CARTESIAN_POINT ( 'NONE',  ( 27.97500000122903074, -5.773502691896255534, -1.060575238724906372E-15 ) ) ;
#48428 = CARTESIAN_POINT ( 'NONE',  ( 5.859375000614519102, 4.541064518000418104, -2.621784821874998173 ) ) ;
#48429 = CARTESIAN_POINT ( 'NONE',  ( 16.43437500061451573, -4.541064518000419881, 2.621784821874995952 ) ) ;
#48430 = CARTESIAN_POINT ( 'NONE',  ( 10.03125000122903288, 6.123233995736764310E-16, -4.999999999999998224 ) ) ;
#48431 = CARTESIAN_POINT ( 'NONE',  ( 24.86250000000000071, 2.886751345948129099, -4.999999999999998224 ) ) ;
#48432 = CARTESIAN_POINT ( 'NONE',  ( 3.075000001229035718, 2.886751345948126879, 4.999999999999999112 ) ) ;
#48433 = CARTESIAN_POINT ( 'NONE',  ( 26.18437500061451573, 4.541064518000418104, 2.621784821874999949 ) ) ;
#48434 = CARTESIAN_POINT ( 'NONE',  ( -3.756430356249999214, 14.29062499938548214, 27.83122392262697531 ) ) ;
#48435 = CARTESIAN_POINT ( 'NONE',  ( 21.75000000000000000, 4.330127018922192761, -2.499999999999997780 ) ) ;
#48436 = CARTESIAN_POINT ( 'NONE',  ( 7.575000000000001954, -4.330127018922194537, 2.499999999999995559 ) ) ;
#48437 = CARTESIAN_POINT ( 'NONE',  ( 10.54687500061451644, -4.119189519843965641, -2.378215178125001383 ) ) ;
#48438 = CARTESIAN_POINT ( 'NONE',  ( 21.70312500061451644, 0.000000000000000000, 5.243569643749999010 ) ) ;
#48439 = CARTESIAN_POINT ( 'NONE',  ( 12.86250000000000071, 2.886751345948126879, 4.999999999999999112 ) ) ;
#48440 = CARTESIAN_POINT ( 'NONE',  ( 5.240625000614516971, -3.027376345333610441, -5.243569643749999898 ) ) ;
#48441 =( BOUNDED_CURVE ( )  B_SPLINE_CURVE ( 2, ( #20060, #69958, #42616, #8630, #9367, #53701, #20431 ),
 .UNSPECIFIED., .F., .F. ) 
 B_SPLINE_CURVE_WITH_KNOTS ( ( 3, 2, 2, 3 ),
 ( 0.4300000000000001044, 0.4333333333333334036, 0.4366666666666667029, 0.4400000000000000022 ),
 .UNSPECIFIED. ) 
 CURVE ( )  GEOMETRIC_REPRESENTATION_ITEM ( )  RATIONAL_B_SPLINE_CURVE ( ( 0.9999999999999955591, 0.8660254037844431485, 1.000000000000000000, 0.8660254037844387076, 1.000000000000000000, 0.8660254037844387076, 1.000000000000000000 ) ) 
 REPRESENTATION_ITEM ( '' )  );
#48442 = CARTESIAN_POINT ( 'NONE',  ( 19.91250000000000142, 2.886751345948129099, -4.999999999999998224 ) ) ;
#48443 = CARTESIAN_POINT ( 'NONE',  ( 17.87812500061451715, 6.421520780324663323E-16, -5.243569643749999010 ) ) ;
#48444 = CARTESIAN_POINT ( 'NONE',  ( 2.817472997146174052, -4.130598735093008678, -2.817472997146206026 ) ) ;
#48445 = CARTESIAN_POINT ( 'NONE',  ( 23.13750000122903216, 6.123233995736764310E-16, -4.999999999999998224 ) ) ;
#48446 = CARTESIAN_POINT ( 'NONE',  ( -3.756430356250000102, 19.61562499938548143, 30.00000000000000000 ) ) ;
#48447 = CARTESIAN_POINT ( 'NONE',  ( 3.149999999999999911, -4.330127018922190985, -2.500000000000001332 ) ) ;
#48448 = VERTEX_POINT ( 'NONE', #6766 ) ;
#48449 = CARTESIAN_POINT ( 'NONE',  ( 18.85312500061451502, 4.541064518000418104, -2.621784821874998173 ) ) ;
#48450 = CARTESIAN_POINT ( 'NONE',  ( 25.56562500061452070, 3.027376345333613106, -5.243569643749998122 ) ) ;
#48451 = CARTESIAN_POINT ( 'NONE',  ( 24.53437500061451715, -4.541064518000419881, 2.621784821874995952 ) ) ;
#48452 = CARTESIAN_POINT ( 'NONE',  ( 10.12500000000000178, 4.330127018922191873, 2.499999999999999556 ) ) ;
#48453 = CARTESIAN_POINT ( 'NONE',  ( 12.21562500061451573, 3.027376345333611329, 5.243569643749999010 ) ) ;
#48454 = CARTESIAN_POINT ( 'NONE',  ( 27.32812500061451644, 6.421520780324663323E-16, -5.243569643749999010 ) ) ;
#48455 = CARTESIAN_POINT ( 'NONE',  ( 17.25937500061451502, 0.000000000000000000, 5.243569643749999010 ) ) ;
#48456 = CARTESIAN_POINT ( 'NONE',  ( 8.765625000614518214, -6.054752690667223547, -1.112240025338166033E-15 ) ) ;
#48457 = FACE_OUTER_BOUND ( 'NONE', #55301, .T. ) ;
#48458 = CARTESIAN_POINT ( 'NONE',  ( 2.121784821874999061, 12.05937500061451750, 26.32496088578401583 ) ) ;
#48459 = CARTESIAN_POINT ( 'NONE',  ( 23.13750000122903216, 6.123233995736764310E-16, -4.999999999999998224 ) ) ;
#48460 = CARTESIAN_POINT ( 'NONE',  ( 18.79687500061451644, -2.746126346562641984, -4.756430356249999214 ) ) ;
#48461 = CARTESIAN_POINT ( 'NONE',  ( 15.36562500061451608, 3.027376345333611329, 5.243569643749999010 ) ) ;
#48462 = CARTESIAN_POINT ( 'NONE',  ( 8.746875000614515727, -3.027376345333614438, 5.243569643749998122 ) ) ;
#48463 = CARTESIAN_POINT ( 'NONE',  ( 8.784375000614518925, -4.541064518000419881, 2.621784821874995952 ) ) ;
#48464 = VERTEX_POINT ( 'NONE', #64358 ) ;
#48465 = CARTESIAN_POINT ( 'NONE',  ( 29.55937500061451573, -4.541064518000417216, -2.621784821875001281 ) ) ;
#48466 = CARTESIAN_POINT ( 'NONE',  ( 20.76562500061451644, 3.027376345333611329, 5.243569643749999010 ) ) ;
#48467 = CARTESIAN_POINT ( 'NONE',  ( 16.17187500061451644, 3.027376345333613106, -5.243569643749998122 ) ) ;
#48468 = CARTESIAN_POINT ( 'NONE',  ( 22.41562500061451502, 3.027376345333613106, -5.243569643749998122 ) ) ;
#48469 = CARTESIAN_POINT ( 'NONE',  ( 8.484601909799253346E-16, 12.46250000000000213, 34.61880215351700230 ) ) ;
#48470 = CARTESIAN_POINT ( 'NONE',  ( 26.65312500061451573, 0.000000000000000000, 5.243569643749999010 ) ) ;
#48471 = CARTESIAN_POINT ( 'NONE',  ( 7.950000001229033053, 5.773502691896255534, 3.535250795749688894E-16 ) ) ;
#48472 = VERTEX_POINT ( 'NONE', #30386 ) ;
#48473 = LINE ( 'NONE', #70997, #53373 ) ;
#48474 = CARTESIAN_POINT ( 'NONE',  ( 8.484601909799253346E-16, 18.31250000000000355, -25.38119784648299770 ) ) ;
#48475 = CARTESIAN_POINT ( 'NONE',  ( 25.83750000122903501, 6.123233995736764310E-16, -4.999999999999998224 ) ) ;
#48476 = CARTESIAN_POINT ( 'NONE',  ( 3.756430356250000102, 15.00312499938548427, 30.00000000000000000 ) ) ;
#48477 = CARTESIAN_POINT ( 'NONE',  ( 6.346875000614517148, 6.054752690667223547, 3.707466751127219781E-16 ) ) ;
#48478 = CARTESIAN_POINT ( 'NONE',  ( 20.53125000122903288, 4.330127018922191873, 2.499999999999999556 ) ) ;
#48479 = CARTESIAN_POINT ( 'NONE',  ( 14.65312500061451573, -4.541064518000417216, -2.621784821875001281 ) ) ;
#48480 = CARTESIAN_POINT ( 'NONE',  ( 8.746875000614515727, -3.027376345333614438, 5.243569643749998122 ) ) ;
#48481 = CARTESIAN_POINT ( 'NONE',  ( 28.08750000122903145, 6.123233995736764310E-16, -4.999999999999998224 ) ) ;
#48482 = CARTESIAN_POINT ( 'NONE',  ( 17.22187500061451715, 3.027376345333611329, 5.243569643749999010 ) ) ;
#48483 = CARTESIAN_POINT ( 'NONE',  ( 5.296875000614518214, -3.027376345333610441, -5.243569643749999898 ) ) ;
#48484 = CARTESIAN_POINT ( 'NONE',  ( 29.81250000000000000, 2.886751345948129099, -4.999999999999998224 ) ) ;
#48485 = CARTESIAN_POINT ( 'NONE',  ( 5.128125000614516260, -4.541064518000419881, 2.621784821874995952 ) ) ;
#48486 = CARTESIAN_POINT ( 'NONE',  ( 15.62812500061451537, 6.421520780324663323E-16, -5.243569643749999010 ) ) ;
#48487 = ORIENTED_EDGE ( 'NONE', *, *, #8538, .F. ) ;
#48488 = CARTESIAN_POINT ( 'NONE',  ( 11.65312500061451573, 4.541064518000418104, -2.621784821874998173 ) ) ;
#48489 = CARTESIAN_POINT ( 'NONE',  ( 5.025000001229035895, -5.773502691896255534, -1.060575238724906372E-15 ) ) ;
#48490 = CARTESIAN_POINT ( 'NONE',  ( 11.54062500061451857, -3.027376345333610441, -5.243569643749999898 ) ) ;
#48491 = CARTESIAN_POINT ( 'NONE',  ( 20.03437500061451715, -4.119189519843968306, 2.378215178124996054 ) ) ;
#48492 = CARTESIAN_POINT ( 'NONE',  ( 11.25000000000000000, -4.330127018922190985, -2.500000000000001332 ) ) ;
#48493 = CARTESIAN_POINT ( 'NONE',  ( 3.300000001229034918, -2.886751345948125991, -5.000000000000000000 ) ) ;
#48494 = CARTESIAN_POINT ( 'NONE',  ( 17.55000000000000071, -4.330127018922190985, -2.500000000000001332 ) ) ;
#48495 = CARTESIAN_POINT ( 'NONE',  ( 19.58437500061451786, -4.541064518000419881, 2.621784821874995952 ) ) ;
#48496 = CARTESIAN_POINT ( 'NONE',  ( 16.87500000122903288, 2.886751345948129099, -4.999999999999998224 ) ) ;
#48497 = CARTESIAN_POINT ( 'NONE',  ( 21.30000000000000071, 4.330127018922192761, -2.499999999999997780 ) ) ;
#48498 = CARTESIAN_POINT ( 'NONE',  ( 2.121784821875001281, 16.35312500061451857, -26.32496088578401938 ) ) ;
#48499 = LINE ( 'NONE', #48131, #5286 ) ;
#48500 = CARTESIAN_POINT ( 'NONE',  ( 7.320879633048903241E-15, 18.53750000000000142, 26.00000000000000355 ) ) ;
#48501 = CYLINDRICAL_SURFACE ( 'NONE', #6504, 4.000000000000000000 ) ;
#48502 = CARTESIAN_POINT ( 'NONE',  ( 11.94375000122903430, 5.773502691896255534, 3.535250795749688401E-16 ) ) ;
#48503 = CARTESIAN_POINT ( 'NONE',  ( 18.58125000122903003, 6.123233995736764310E-16, -4.999999999999998224 ) ) ;
#48504 = CARTESIAN_POINT ( 'NONE',  ( 15.49687500061451750, -3.027376345333614438, 5.243569643749998122 ) ) ;
#48505 = CARTESIAN_POINT ( 'NONE',  ( 18.24375000122903501, 5.773502691896255534, 3.535250795749688401E-16 ) ) ;
#48506 = EDGE_CURVE ( 'NONE', #13629, #55912, #8122, .T. ) ;
#48507 = CARTESIAN_POINT ( 'NONE',  ( 10.97812500061451679, -4.541064518000419881, 2.621784821874995952 ) ) ;
#48508 = CARTESIAN_POINT ( 'NONE',  ( 7.143750001229034474, -2.886751345948129988, 4.999999999999997335 ) ) ;
#48509 = CARTESIAN_POINT ( 'NONE',  ( 22.69687500061451857, -3.027376345333614438, 5.243569643749998122 ) ) ;
#48510 = CARTESIAN_POINT ( 'NONE',  ( 15.75937500061451502, 2.746126346562643317, 4.756430356249998326 ) ) ;
#48511 = CARTESIAN_POINT ( 'NONE',  ( 7.715625000614515727, 3.027376345333611329, 5.243569643749999010 ) ) ;
#48512 = CARTESIAN_POINT ( 'NONE',  ( 12.49687500061451573, -3.027376345333610441, -5.243569643749999898 ) ) ;
#48513 = ORIENTED_EDGE ( 'NONE', *, *, #34066, .F. ) ;
#48514 = CARTESIAN_POINT ( 'NONE',  ( 23.25937500061451857, -4.541064518000417216, -2.621784821875001281 ) ) ;
#48515 = CARTESIAN_POINT ( 'NONE',  ( 28.79062500061451502, 6.054752690667223547, 3.707466751127219781E-16 ) ) ;
#48516 = CYLINDRICAL_SURFACE ( 'NONE', #43155, 4.999999999999998224 ) ;
#48517 = CARTESIAN_POINT ( 'NONE',  ( 7.162500000000001421, -5.773502691896255534, -1.060575238724906372E-15 ) ) ;
#48518 = CARTESIAN_POINT ( 'NONE',  ( 16.38750000122903216, 6.123233995736764310E-16, -4.999999999999998224 ) ) ;
#48519 = CARTESIAN_POINT ( 'NONE',  ( 27.37500000122903998, 2.886751345948102454, 5.000000000000042633 ) ) ;
#48520 = CARTESIAN_POINT ( 'NONE',  ( 7.584375000614516971, 5.492252693125287522, 3.363034840372157021E-16 ) ) ;
#48521 = ORIENTED_EDGE ( 'NONE', *, *, #67203, .T. ) ;
#48522 = CARTESIAN_POINT ( 'NONE',  ( 15.33750000000000036, -2.886751345948125991, -5.000000000000000000 ) ) ;
#48523 = CARTESIAN_POINT ( 'NONE',  ( 18.22499999999999787, 4.330127018922191873, 2.499999999999999556 ) ) ;
#48524 = CARTESIAN_POINT ( 'NONE',  ( 14.20312500061451644, -4.541064518000417216, -2.621784821875001281 ) ) ;
#48525 = ORIENTED_EDGE ( 'NONE', *, *, #24878, .F. ) ;
#48526 = CARTESIAN_POINT ( 'NONE',  ( 3.712500001229034563, -4.330127018922190985, -2.500000000000001332 ) ) ;
#48527 = CARTESIAN_POINT ( 'NONE',  ( -4.243569643749999898, 16.25937500061451857, -30.00000000000000000 ) ) ;
#48528 = CARTESIAN_POINT ( 'NONE',  ( 3.478125000614517237, 6.421520780324663323E-16, -5.243569643749999010 ) ) ;
#48529 = CARTESIAN_POINT ( 'NONE',  ( 1.626862140677534273E-15, 12.01250000000000284, 34.00000000000000000 ) ) ;
#48530 = CARTESIAN_POINT ( 'NONE',  ( 9.375000000000001776, -4.330127018922194537, 2.499999999999995559 ) ) ;
#48531 = CARTESIAN_POINT ( 'NONE',  ( 29.67187500061451644, 4.119189519843966529, 2.378215178124999607 ) ) ;
#48532 = EDGE_LOOP ( 'NONE', ( #57998, #47201, #71522, #6951 ) ) ;
#48533 = CARTESIAN_POINT ( 'NONE',  ( -4.243569643749997233, 14.44062500061451715, 32.45002607614398471 ) ) ;
#48534 = CARTESIAN_POINT ( 'NONE',  ( 26.61562500061451786, 3.027376345333611329, 5.243569643749999010 ) ) ;
#48535 = CARTESIAN_POINT ( 'NONE',  ( 9.187500000000001776, 5.773502691896255534, 3.535250795749688894E-16 ) ) ;
#48536 = CARTESIAN_POINT ( 'NONE',  ( -7.967954043666661671E-16, 18.82812499938548356, 34.33755215474603517 ) ) ;
#48537 = CARTESIAN_POINT ( 'NONE',  ( 23.07187500061451857, 3.027376345333611329, 5.243569643749999010 ) ) ;
#48538 = CARTESIAN_POINT ( 'NONE',  ( 18.44062500061451715, 6.054752690667223547, 3.707466751127219781E-16 ) ) ;
#48539 = CARTESIAN_POINT ( 'NONE',  ( -2.121784821874999949, 12.97812500061459318, -33.67503911421598417 ) ) ;
#48540 = CARTESIAN_POINT ( 'NONE',  ( 23.17500000122903359, 2.886751345948129099, -4.999999999999998224 ) ) ;
#48541 = CARTESIAN_POINT ( 'NONE',  ( 4.378125000614518925, 6.421520780324663323E-16, -5.243569643749999010 ) ) ;
#48542 = CARTESIAN_POINT ( 'NONE',  ( 27.19687500061451857, -2.746126346562646425, 4.756430356249996549 ) ) ;
#48543 = CARTESIAN_POINT ( 'NONE',  ( 21.25312500061451715, 0.000000000000000000, 5.243569643749999010 ) ) ;
#48544 = CARTESIAN_POINT ( 'NONE',  ( 10.02187500061451964, 2.746126346562643317, 4.756430356249998326 ) ) ;
#48545 = CARTESIAN_POINT ( 'NONE',  ( -1.878215178125001827, 15.64062499938548356, 33.25316411605952283 ) ) ;
#48546 = CARTESIAN_POINT ( 'NONE',  ( 17.82187500061451502, -6.054752690667223547, -1.112240025338166033E-15 ) ) ;
#48547 = CARTESIAN_POINT ( 'NONE',  ( 16.54687500061451644, -3.027376345333610441, -5.243569643749999898 ) ) ;
#48548 = CARTESIAN_POINT ( 'NONE',  ( 24.83437500061451431, 4.541064518000418104, 2.621784821874999949 ) ) ;
#48549 = CARTESIAN_POINT ( 'NONE',  ( 2.121784821874999061, 15.20937500061451786, 26.32496088578401583 ) ) ;
#48550 = CARTESIAN_POINT ( 'NONE',  ( 5.465625000614517504, 3.027376345333611329, 5.243569643749999010 ) ) ;
#48551 = CARTESIAN_POINT ( 'NONE',  ( 29.01562500061451644, -6.054752690667223547, -1.112240025338166033E-15 ) ) ;
#48552 = CARTESIAN_POINT ( 'NONE',  ( 28.19062500061451715, -3.027376345333610441, -5.243569643749999898 ) ) ;
#48553 = CARTESIAN_POINT ( 'NONE',  ( 1.071796769724490783, 19.34509619066136565, -26.00000000000000000 ) ) ;
#48554 = CARTESIAN_POINT ( 'NONE',  ( -3.999999999999999556, 19.06249999999999645, 27.69059892324149530 ) ) ;
#48555 = CARTESIAN_POINT ( 'NONE',  ( 6.909375000614518036, 0.000000000000000000, 5.243569643749999010 ) ) ;
#48556 =( NAMED_UNIT ( * ) PLANE_ANGLE_UNIT ( ) SI_UNIT ( $, .RADIAN. ) );
#48557 = CARTESIAN_POINT ( 'NONE',  ( 13.16250000122903430, -4.330127018922190985, -2.500000000000001332 ) ) ;
#48558 = CARTESIAN_POINT ( 'NONE',  ( 10.53750000122903252, 6.123233995736764310E-16, -4.999999999999998224 ) ) ;
#48559 = CARTESIAN_POINT ( 'NONE',  ( 5.953125000614519102, 0.000000000000000000, 5.243569643749999010 ) ) ;
#48560 = CARTESIAN_POINT ( 'NONE',  ( 4.000000000000000000, 16.49374999877096570, 30.00000000000000000 ) ) ;
#48561 = CARTESIAN_POINT ( 'NONE',  ( 21.84375000122903288, 5.773502691896255534, 3.535250795749688894E-16 ) ) ;
#48562 = CARTESIAN_POINT ( 'NONE',  ( 15.27187500061451786, 3.027376345333613106, -5.243569643749998122 ) ) ;
#48563 = CARTESIAN_POINT ( 'NONE',  ( 4.711411573247316298, 1.674097066322985938, -4.711411573247316298 ) ) ;
#48564 = VERTEX_POINT ( 'NONE', #29300 ) ;
#48565 = CARTESIAN_POINT ( 'NONE',  ( 22.04062500061451502, 6.054752690667223547, 3.707466751127219781E-16 ) ) ;
#48566 = CARTESIAN_POINT ( 'NONE',  ( 8.240625000614516082, -3.027376345333614438, 5.243569643749998122 ) ) ;
#48567 = CARTESIAN_POINT ( 'NONE',  ( 23.70937500061451786, -4.541064518000417216, -2.621784821875001281 ) ) ;
#48568 = CARTESIAN_POINT ( 'NONE',  ( 7.715625000614515727, 3.027376345333611329, 5.243569643749999010 ) ) ;
#48569 = CARTESIAN_POINT ( 'NONE',  ( 9.000000001229034652, -2.886751345948129988, 4.999999999999997335 ) ) ;
#48570 = ADVANCED_FACE ( 'NONE', ( #34469 ), #52192, .T. ) ;
#48571 = CARTESIAN_POINT ( 'NONE',  ( 22.30312500061451431, -4.541064518000417216, -2.621784821875001281 ) ) ;
#48572 = CARTESIAN_POINT ( 'NONE',  ( -3.000416591977282496E-16, 11.14062500061451644, -34.90005215228797653 ) ) ;
#48573 = CARTESIAN_POINT ( 'NONE',  ( 9.487500001229033586, -4.330127018922194537, 2.499999999999995559 ) ) ;
#48574 = CARTESIAN_POINT ( 'NONE',  ( 20.16562500061451146, 3.027376345333613106, -5.243569643749998122 ) ) ;
#48575 = EDGE_CURVE ( 'NONE', #28191, #22800, #6177, .T. ) ;
#48576 = CARTESIAN_POINT ( 'NONE',  ( 17.01562500061451644, 3.027376345333613106, -5.243569643749998122 ) ) ;
#48577 = CARTESIAN_POINT ( 'NONE',  ( 29.18437500061451573, 5.824947211148865298E-16, -4.756430356249998326 ) ) ;
#48578 = CARTESIAN_POINT ( 'NONE',  ( 18.97499999999999787, 6.123233995736764310E-16, -4.999999999999998224 ) ) ;
#48579 = CARTESIAN_POINT ( 'NONE',  ( 10.38750000122903572, -4.330127018922194537, 2.499999999999995559 ) ) ;
#48580 = CARTESIAN_POINT ( 'NONE',  ( 7.190625000614518036, 6.054752690667223547, 3.707466751127219781E-16 ) ) ;
#48581 = CARTESIAN_POINT ( 'NONE',  ( 11.48437500061451644, -4.541064518000419881, 2.621784821874995952 ) ) ;
#48582 = CARTESIAN_POINT ( 'NONE',  ( 12.25312500061451537, 0.000000000000000000, 5.243569643749999010 ) ) ;
#48583 = EDGE_CURVE ( 'NONE', #13160, #30208, #40695, .T. ) ;
#48584 = CARTESIAN_POINT ( 'NONE',  ( 24.22500000122903430, 2.886751345948126879, 4.999999999999999112 ) ) ;
#48585 = CARTESIAN_POINT ( 'NONE',  ( 22.13437500061451502, 4.541064518000418104, 2.621784821874999949 ) ) ;
#48586 = ADVANCED_FACE ( 'NONE', ( #59170 ), #31848, .F. ) ;
#48587 = CARTESIAN_POINT ( 'NONE',  ( 5.662500001229035185, 4.330127018922192761, -2.499999999999997780 ) ) ;
#48588 = CARTESIAN_POINT ( 'NONE',  ( 7.621875000614519280, 3.027376345333613106, -5.243569643749998122 ) ) ;
#48589 = CARTESIAN_POINT ( 'NONE',  ( 23.03437500061451715, 4.541064518000418104, 2.621784821874999949 ) ) ;
#48590 =( BOUNDED_SURFACE ( )  B_SPLINE_SURFACE ( 1, 2, ( 
 ( #18950, #7889, #13408, #52953, #7522, #64397, #46694, #24142, #52593, #34871, #41157, #69231, #12336, #57399, #6805, #29339, #63666, #18221, #63308, #35236, #18592, #13056, #30053, #2000, #36329, #25230, #70311, #48515, #60304, #47776, #19684, #3080, #59575, #31520, #15247, #58844, #48146, #65494, #8254, #42237, #37423, #8616, #71411, #25974, #31886, #8988, #64762, #54061, #30784, #53315, #20417, #14152, #42965, #14884, #9353, #25608, #48881, #2714, #70670, #54420, #20046, #3456, #59946, #3821, #42601, #71042, #65127, #36687, #59208, #31144, #53685, #14517, #37050, #26342, #20786, #43343, #65865, #37784, #14032, #46210, #69476, #29936, #59093, #46572, #68750, #58000, #42122, #18108, #51756, #29220, #24023, #30665, #41041, #25114, #12585, #53198, #69116, #7049, #58358, #70189, #40670, #30306, #52476, #12942, #1156, #19567, #7408, #24753, #57643, #24390, #35119, #52839, #1884, #36573, #1519, #47296, #36210, #58727, #63190, #69833, #7771, #29579, #23665, #18476, #52116, #2238, #63555, #35478, #41397, #46940, #18833, #47656, #63911, #19196, #13298, #35835, #41751, #64278, #13666, #8139, #2594, #64648, #43225, #71288, #54308, #8866, #43955, #9599, #66477, #21399, #20667, #3700, #15855, #26964, #36938, #26593, #65013, #71662, #65374, #9236, #54664, #14400, #38400, #65745, #15129, #8498, #59458, #31029, #26227, #42852, #49134, #19936, #66110, #37667, #60189, #48765, #31402, #53565, #32131, #2960, #25490, #4068, #21037, #48035, #49492, #53942, #43588, #3338, #15489, #14762, #31772, #38032, #25862, #70560, #60554, #9961, #42489, #48401, #70927, #32498, #37307, #55033, #4436, #72022, #20298, #59829, #18518, #52156, #18876, #63233, #24432, #36253, #12264, #46981, #1198, #30351, #13711, #69517, #1560, #68793, #58768, #34794, #41791, #17789, #18149, #40348, #57327, #62868, #7450, #46253, #2277, #12985, #41438, #63596, #69159, #28896, #51435, #52879, #6731, #837, #41083, #52518, #29265, #23704, #35521, #63955, #51795, #58041, #58402, #12627, #13340, #35877, #29977, #23346, #19236, #24794, #40716, #7815, #68426, #35162, #47337, #57686, #69870, #64320, #45895, #7091, #1927, #29621, #24070, #46615, #37708, #42163, #59134, #59499, #65418, #8542, #44646, #14806, #53609, #70600, #25530, #3001, #8912, #70967, #26268, #25903, #9277, #64689, #60229, #48072, #16537, #14074, #15170, #31443, #53984, #71334, #19973, #54710, #39090, #42526, #25156, #36977, #22088, #70233, #30705, #8177, #65052, #9643, #14442, #5107, #36613, #32176, #3381, #31070, #37350, #50177, #47696, #31811, #48443, #20340, #53238, #72705, #42893, #3743, #59872, #54350, #48805, #20710, #43268, #2635, #65789, #27641, #67176, #19606, #5470, #57145, #40179, #28010, #18337, #56437, #61972, #17619, #46442, #67533, #660, #16896, #50895, #6917, #56079, #51625, #11734, #68257, #12094, #45356, #11374, #29089, #73066, #46081, #23168, #51258, #34251, #33893, #23894, #62699, #68980, #1384, #45722, #56783, #61607, #29447, #39451, #6557, #44996, #1025, #67890, #62338, #34615, #5828, #11008, #23531, #68616, #33529, #28359, #50538, #6189, #22804, #17979, #40538, #63054, #28718, #12456, #34987, #57516, #295, #51985, #22447, #17262, #39824, #58955, #58228, #25352, #31261, #52342, #47526, #1745, #2108, #58595, #2458, #69343, #24619, #63777, #48263, #19801, #3198, #70787, #42354, #2824, #69698, #53803, #41265, #24981, #40910, #25726, #57868, #8002, #41621, #41989, #64876, #30537, #36074, #36441, #18701, #70055, #53064, #8363, #47898, #24258, #46806, #19428, #30171, #13165, #70426, #7277, #64140, #14264, #19063, #63423, #29807, #35706, #64509, #12810, #7633, #52702, #47166, #36803, #13902, #13527, #30892, #53434, #59318, #35345, #8727, #38261, #65609, #21631, #5023, #60789, #43456, #60056, #27558, #3566, #33088, #9099, #9467, #31637, #26089, #54169, #71893, #37534, #66720, #4304, #10195, #54897, #60418, #50089, #20162, #44189, #48627, #42716, #9829, #43820, #71152, #14997, #26829, #32730, #20524, #49363, #49727, #3934, #15722, #55267, #21266, #65237, #10560, #16093, #43083, #27192, #59692, #54532, #4662, #31997, #72254, #38641, #14627, #61165, #66344, #55627, #37166, #26457, #48997, #71527, #20902, #65978, #15358, #37900, #32359, #6105, #44916, #61888, #16815, #67453, #50813, #62256, #17536, #17180, #578, #33447, #51540, #39371, #6831, #55991, #6468, #215, #45273, #62612, #11293, #45994, #29366, #57061, #16450, #12008, #23448, #34531, #40098, #29003, #23083, #28636, #68531, #45641, #941, #5384, #50456, #22720, #56704, #72982, #34899, #51174, #33814, #56357, #5747, #28281, #67806, #11653, #17892, #39739, #68173, #27922, #40452, #34168, #72620, #22364, #62968, #12364, #57427, #22004, #44560, #67091, #39007, #61522, #10920, #64423, #2740, #13815, #19341, #52980, #30809, #41537, #47080, #47439, #29719, #35985, #69615, #41896, #36355, #12724, #63338, #58504, #41183, #35260, #58869, #18248, #2025, #8279, #7547, #51898, #40821, #57782, #30451, #59234, #7191, #52257, #63692, #53342, #64055, #24536, #25259, #13083, #69971, #8642, #1660, #47806, #24169, #70335, #36712, #19712, #18976, #18618, #1296, #46721, #64787, #69256, #35621, #58141, #30081, #52619, #2376, #13435, #42264, #7914, #14178, #24894, #23806, #46357, #68891, #32641, #59602, #53714, #20814, #54809, #9016, #3484, #15273, #71809, #37078, #37812, #60698, #14910, #26743, #66255, #65893, #31171, #21546, #27107, #14542, #38174, #70697, #65524, #21179, #48541, #49276, #10111, #25635, #43731, #4215, #60332, #55182, #32275, #4577, #65152, #31546, #9380, #9741, #54086, #66627, #15633, #26002, #20443, #71068, #42993, #31912, #43369, #49640, #48908, #72167, #37452, #44101, #59971, #38553, #54448, #16004, #3847, #26368, #61076, #71439, #3106, #48173, #20072, #42628, #22994, #34446, #45554 ),
 ( #39285, #10474, #72529, #67004, #62171, #17801, #21917, #16365, #22280, #62524, #132, #33729, #484, #44832, #6018, #40361, #38920, #28553, #55904, #11921, #68438, #51088, #56275, #50373, #33003, #61439, #23359, #44473, #72898, #10832, #33368, #5296, #11568, #27842, #56974, #67719, #68085, #45187, #50729, #55542, #4938, #6378, #67367, #27472, #22637, #34083, #16730, #61799, #17092, #17452, #11202, #39652, #40010, #5664, #28911, #51449, #56624, #50004, #852, #45907, #28200, #69884, #29277, #24081, #30364, #7103, #7828, #41804, #57339, #2652, #52530, #58053, #70250, #8193, #18161, #52893, #46266, #2290, #46628, #63606, #35891, #68805, #47711, #24444, #69528, #62880, #40730, #12276, #7462, #69170, #24806, #46992, #47351, #29988, #18887, #58415, #19249, #29632, #41449, #6744, #63967, #13350, #64335, #52170, #13727, #53253, #1210, #36269, #23716, #18530, #1938, #58783, #63245, #41095, #12639, #19622, #30721, #25170, #34808, #51807, #35174, #12996, #57698, #1572, #35532, #72077, #27025, #59149, #9294, #42910, #42179, #59516, #8558, #70983, #55096, #31086, #64704, #14088, #36993, #43647, #54002, #38090, #25548, #66171, #8929, #19989, #71352, #10022, #53625, #43285, #65433, #25919, #36628, #32558, #20359, #37725, #70615, #37366, #48091, #65805, #14824, #49556, #14460, #60245, #49193, #71726, #3017, #9659, #20726, #42542, #65068, #31459, #3398, #15187, #48459, #59889, #54365, #31827, #3760, #60613, #26284, #32193, #48821, #54726, #4129, #26659, #21096, #15547, #4496, #5931, #56185, #11112, #67284, #21825, #56889, #22553, #6294, #5578, #38464, #28115, #45101, #39560, #38839, #28465, #11838, #32921, #50644, #55459, #55821, #39199, #48, #49917, #5209, #44390, #28823, #398, #51362, #21459, #22906, #56538, #50289, #34357, #66915, #67637, #44014, #66536, #60990, #61713, #22196, #15916, #61354, #10389, #72813, #4851, #27385, #72441, #16284, #10751, #45464, #33282, #17369, #27750, #67996, #44750, #16643, #17003, #62440, #33641, #62085, #11478, #34001, #51000, #39926, #29550, #69448, #29192, #69086, #6664, #24362, #46545, #8109, #46182, #18805, #7741, #30277, #17719, #41369, #52449, #40279, #30637, #68721, #1127, #29909, #58699, #51726, #12914, #23636, #63161, #19168, #68358, #63879, #23997, #7378, #46909, #57616, #18081, #13270, #12193, #58330, #35447, #63527, #18447, #40642, #36181, #1855, #764, #13637, #57971, #41012, #23272, #41722, #12556, #35808, #57250, #52809, #7019, #1491, #2210, #35091, #45822, #24725, #47268, #62800, #52086, #34720, #69802, #64249, #71260, #37279, #65718, #48372, #9207, #48737, #60163, #19909, #43563, #8838, #20640, #8469, #70899, #59064, #3674, #25835, #60530, #25462, #43198, #9573, #32105, #70162, #15104, #31742, #19539, #9937, #48006, #53537, #54280, #38008, #31004, #65347, #2933, #42462, #71638, #47629, #37640, #3308, #59801, #26198, #36910, #70534, #54638, #64619, #4043, #14737, #42823, #20271, #64984, #15463, #26568, #53169, #66085, #49109, #21011, #2566, #25086, #14375, #42097, #36544, #14006, #59430, #53915, #31374, #15833, #17287, #67200, #39113, #32475, #38378, #55008, #50204, #66831, #50563, #16562, #45022, #27665, #61629, #28034, #39475, #72360, #11031, #49468, #33554, #56104, #73090, #49836, #16921, #22828, #43930, #5495, #66456, #16203, #72729, #22471, #60902, #38754, #55375, #39849, #11399, #67916, #62362, #33918, #67557, #61275, #45380, #32838, #61998, #4414, #26943, #72001, #22113, #33198, #21376, #21741, #10305, #10668, #4769, #27302, #44302, #55737, #5131, #56461, #44670, #28383, #5852, #50921, #319, #62724, #40936, #53733, #28742, #12836, #35010, #68641, #42646, #6941, #17642, #35370, #57540, #20089, #57170, #7301, #19731, #42281, #51282, #29832, #63450, #684, #11759, #6583, #12117, #57893, #70714, #40202, #23918, #34641, #1048, #31191, #6214, #1772, #29472, #18366, #52367, #18004, #29113, #25278, #23191, #70354, #46467, #1410, #52009, #51647, #48191, #47824, #34276, #25655, #69004, #64805, #56808, #3126, #23557, #14195, #68281, #36730, #40562, #12483, #59252, #46104, #45745, #8660, #63081, #65170, #48558, #14561, #9758, #26386, #10128, #49293, #4594, #60349, #21197, #60718, #72186, #31928, #71826, #9033, #43749, #66274, #32660, #9398, #49658, #55559, #3500, #15652, #26019, #48928, #32292, #26761, #20458, #71457, #14928, #72547, #44119, #27488, #21934, #66646, #27124, #20833, #4955, #65541, #38191, #37094, #50022, #31563, #54827, #65910, #59619, #54465, #54102, #43386, #71084, #43012, #37468, #59988, #3863, #16023, #15290, #61095, #37829, #38571, #4234, #55201, #21565, #33021, #10493, #45571, #67736, #28216, #1227, #34828, #148, #40028, #72914, #67023, #62188, #5680, #62541, #28570, #56991, #39668, #503, #11938, #51466, #11221, #51106, #61456, #23013, #68102, #34463, #61816, #28930, #57355, #55920, #17468, #5316, #50745, #11584, #6036, #22296, #22654, #67384, #51824, #23376, #6760, #44490, #45924, #6398, #45203, #29294, #44848, #869, #16383, #38938, #10850, #34101, #17109, #33384, #33745, #27858, #56640, #50389, #16746, #39303, #56290, #68456, #17818, #40379, #62898, #12293, #47728, #18547, #1589, #52910, #64719, #40748, #24823, #47011, #7479, #53641, #14103, #52550, #19267, #52187, #18905, #29649, #47370, #69546, #31101, #69187, #41821, #30738, #53270, #63263, #64353, #2308, #12655, #23733, #41112, #24099, #69901, #8573, #46647, #35909, #63622, #13012, #42195, #18179, #13743, #41466, #30381, #36285, #30007, #35550, #58799, #35190, #8209, #58434, #13367, #63985, #58069, #59165, #2668, #46282, #36643, #7844, #25185, #68822, #57715, #1956, #70267, #7120, #19638, #24463, #3774, #49207, #59531, #61006, #37740, #9674, #3033, #8943, #27041, #15564, #43664, #4143, #55112, #65820, #71367, #71741, #54017, #60260, #20742, #66186 ) ),
 .UNSPECIFIED., .F., .F., .F. ) 
 B_SPLINE_SURFACE_WITH_KNOTS ( ( 2, 2 ),
 ( 3, 2, 2, 2, 2, 2, 2, 2, 2, 2, 2, 2, 2, 2, 2, 2, 2, 2, 2, 2, 2, 2, 2, 2, 2, 2, 2, 2, 2, 2, 2, 2, 2, 2, 2, 2, 2, 2, 2, 2, 2, 2, 2, 2, 2, 2, 2, 2, 2, 2, 2, 2, 2, 2, 2, 2, 2, 2, 2, 2, 2, 2, 2, 2, 2, 2, 2, 2, 2, 2, 2, 2, 2, 2, 2, 2, 2, 2, 2, 2, 2, 2, 2, 2, 2, 2, 2, 2, 2, 2, 2, 2, 2, 2, 2, 2, 2, 2, 2, 2, 2, 2, 2, 2, 2, 2, 2, 2, 2, 2, 2, 2, 2, 2, 2, 2, 2, 2, 2, 2, 2, 2, 2, 2, 2, 2, 2, 2, 2, 2, 2, 2, 2, 2, 2, 2, 2, 2, 2, 2, 2, 2, 2, 2, 2, 2, 2, 2, 2, 2, 2, 2, 2, 2, 2, 2, 2, 2, 2, 2, 2, 2, 2, 2, 2, 2, 2, 2, 2, 2, 2, 2, 2, 2, 2, 2, 2, 2, 2, 2, 2, 2, 2, 2, 2, 2, 2, 2, 2, 2, 2, 2, 2, 2, 2, 2, 2, 2, 2, 2, 2, 2, 2, 2, 2, 2, 2, 2, 2, 2, 2, 2, 2, 2, 2, 2, 2, 2, 2, 2, 2, 2, 2, 2, 2, 2, 2, 2, 2, 2, 2, 2, 2, 2, 2, 2, 2, 2, 2, 2, 2, 2, 2, 2, 2, 2, 2, 2, 2, 2, 2, 2, 2, 2, 2, 2, 2, 2, 2, 2, 2, 2, 2, 2, 2, 2, 2, 2, 2, 2, 2, 2, 2, 2, 2, 2, 2, 2, 2, 2, 2, 2, 2, 2, 2, 2, 2, 2, 2, 2, 2, 2, 2, 2, 2, 2, 2, 2, 2, 2, 2, 2, 2, 2, 2, 2, 2, 2, 2, 2, 2, 2, 2, 2, 2, 2, 2, 2, 2, 2, 2, 2, 2, 2, 2, 2, 2, 2, 2, 2, 2, 2, 2, 2, 2, 2, 2, 2, 2, 2, 2, 2, 2, 2, 2, 2, 2, 2, 2, 2, 2, 2, 2, 2, 2, 2, 2, 2, 2, 2, 3 ),
 ( 0.000000000000000000, 1.000000000000000000 ),
 ( 0.000000000000000000, 0.002777777777777777884, 0.005555555555555555768, 0.008333333333333333218, 0.01111111111111111154, 0.01388888888888888812, 0.01666666666666666644, 0.01944444444444444475, 0.02222222222222222307, 0.02500000000000000139, 0.02777777777777777624, 0.03055555555555555455, 0.03333333333333333287, 0.03611111111111110772, 0.03888888888888888951, 0.04166666666666666435, 0.04444444444444444614, 0.04722222222222222099, 0.05000000000000000278, 0.05277777777777777762, 0.05555555555555555247, 0.05833333333333333426, 0.06111111111111110911, 0.06388888888888888395, 0.06666666666666666574, 0.06944444444444444753, 0.07222222222222221544, 0.07499999999999999722, 0.07777777777777777901, 0.08055555555555556080, 0.08333333333333332871, 0.08611111111111111049, 0.08888888888888889228, 0.09166666666666666019, 0.09444444444444444198, 0.09722222222222222376, 0.1000000000000000056, 0.1027777777777777735, 0.1055555555555555552, 0.1083333333333333370, 0.1111111111111111049, 0.1138888888888888867, 0.1166666666666666685, 0.1194444444444444503, 0.1222222222222222182, 0.1250000000000000000, 0.1277777777777777679, 0.1305555555555555636, 0.1333333333333333315, 0.1361111111111110994, 0.1388888888888888951, 0.1416666666666666630, 0.1444444444444444309, 0.1472222222222222265, 0.1499999999999999944, 0.1527777777777777901, 0.1555555555555555580, 0.1583333333333333259, 0.1611111111111111216, 0.1638888888888888895, 0.1666666666666666574, 0.1694444444444444531, 0.1722222222222222210, 0.1749999999999999889, 0.1777777777777777846, 0.1805555555555555525, 0.1833333333333333204, 0.1861111111111111160, 0.1888888888888888840, 0.1916666666666666796, 0.1944444444444444475, 0.1972222222222222154, 0.2000000000000000111, 0.2027777777777777790, 0.2055555555555555469, 0.2083333333333333426, 0.2111111111111111105, 0.2138888888888888784, 0.2166666666666666741, 0.2194444444444444420, 0.2222222222222222099, 0.2250000000000000056, 0.2277777777777777735, 0.2305555555555555691, 0.2333333333333333370, 0.2361111111111111049, 0.2388888888888889006, 0.2416666666666666685, 0.2444444444444444364, 0.2472222222222222321, 0.2500000000000000000, 0.2527777777777777679, 0.2555555555555555358, 0.2583333333333333592, 0.2611111111111111271, 0.2638888888888888951, 0.2666666666666666630, 0.2694444444444444309, 0.2722222222222221988, 0.2750000000000000222, 0.2777777777777777901, 0.2805555555555555580, 0.2833333333333333259, 0.2861111111111110938, 0.2888888888888888618, 0.2916666666666666852, 0.2944444444444444531, 0.2972222222222222210, 0.2999999999999999889, 0.3027777777777777568, 0.3055555555555555802, 0.3083333333333333481, 0.3111111111111111160, 0.3138888888888888840, 0.3166666666666666519, 0.3194444444444444198, 0.3222222222222222432, 0.3250000000000000111, 0.3277777777777777790, 0.3305555555555555469, 0.3333333333333333148, 0.3361111111111111382, 0.3388888888888889062, 0.3416666666666666741, 0.3444444444444444420, 0.3472222222222222099, 0.3499999999999999778, 0.3527777777777778012, 0.3555555555555555691, 0.3583333333333333370, 0.3611111111111111049, 0.3638888888888888729, 0.3666666666666666408, 0.3694444444444444642, 0.3722222222222222321, 0.3750000000000000000, 0.3777777777777777679, 0.3805555555555555358, 0.3833333333333333592, 0.3861111111111111271, 0.3888888888888888951, 0.3916666666666666630, 0.3944444444444444309, 0.3972222222222221988, 0.4000000000000000222, 0.4027777777777777901, 0.4055555555555555580, 0.4083333333333333259, 0.4111111111111110938, 0.4138888888888888618, 0.4166666666666666852, 0.4194444444444444531, 0.4222222222222222210, 0.4249999999999999889, 0.4277777777777777568, 0.4305555555555555802, 0.4333333333333333481, 0.4361111111111111160, 0.4388888888888888840, 0.4416666666666666519, 0.4444444444444444198, 0.4472222222222222432, 0.4500000000000000111, 0.4527777777777777790, 0.4555555555555555469, 0.4583333333333333148, 0.4611111111111111382, 0.4638888888888889062, 0.4666666666666666741, 0.4694444444444444420, 0.4722222222222222099, 0.4749999999999999778, 0.4777777777777778012, 0.4805555555555555691, 0.4833333333333333370, 0.4861111111111111049, 0.4888888888888888729, 0.4916666666666666408, 0.4944444444444444642, 0.4972222222222222321, 0.5000000000000000000, 0.5027777777777777679, 0.5055555555555555358, 0.5083333333333333037, 0.5111111111111110716, 0.5138888888888888395, 0.5166666666666667185, 0.5194444444444444864, 0.5222222222222222543, 0.5250000000000000222, 0.5277777777777777901, 0.5305555555555555580, 0.5333333333333333259, 0.5361111111111110938, 0.5388888888888888618, 0.5416666666666666297, 0.5444444444444443976, 0.5472222222222222765, 0.5500000000000000444, 0.5527777777777778123, 0.5555555555555555802, 0.5583333333333333481, 0.5611111111111111160, 0.5638888888888888840, 0.5666666666666666519, 0.5694444444444444198, 0.5722222222222221877, 0.5749999999999999556, 0.5777777777777777235, 0.5805555555555556024, 0.5833333333333333703, 0.5861111111111111382, 0.5888888888888889062, 0.5916666666666666741, 0.5944444444444444420, 0.5972222222222222099, 0.5999999999999999778, 0.6027777777777777457, 0.6055555555555555136, 0.6083333333333332815, 0.6111111111111111605, 0.6138888888888889284, 0.6166666666666666963, 0.6194444444444444642, 0.6222222222222222321, 0.6250000000000000000, 0.6277777777777777679, 0.6305555555555555358, 0.6333333333333333037, 0.6361111111111110716, 0.6388888888888888395, 0.6416666666666667185, 0.6444444444444444864, 0.6472222222222222543, 0.6500000000000000222, 0.6527777777777777901, 0.6555555555555555580, 0.6583333333333333259, 0.6611111111111110938, 0.6638888888888888618, 0.6666666666666666297, 0.6694444444444443976, 0.6722222222222222765, 0.6750000000000000444, 0.6777777777777778123, 0.6805555555555555802, 0.6833333333333333481, 0.6861111111111111160, 0.6888888888888888840, 0.6916666666666666519, 0.6944444444444444198, 0.6972222222222221877, 0.6999999999999999556, 0.7027777777777777235, 0.7055555555555556024, 0.7083333333333333703, 0.7111111111111111382, 0.7138888888888889062, 0.7166666666666666741, 0.7194444444444444420, 0.7222222222222222099, 0.7249999999999999778, 0.7277777777777777457, 0.7305555555555555136, 0.7333333333333332815, 0.7361111111111111605, 0.7388888888888889284, 0.7416666666666666963, 0.7444444444444444642, 0.7472222222222222321, 0.7500000000000000000, 0.7527777777777777679, 0.7555555555555555358, 0.7583333333333333037, 0.7611111111111110716, 0.7638888888888888395, 0.7666666666666667185, 0.7694444444444444864, 0.7722222222222222543, 0.7750000000000000222, 0.7777777777777777901, 0.7805555555555555580, 0.7833333333333333259, 0.7861111111111110938, 0.7888888888888888618, 0.7916666666666666297, 0.7944444444444443976, 0.7972222222222222765, 0.8000000000000000444, 0.8027777777777778123, 0.8055555555555555802, 0.8083333333333333481, 0.8111111111111111160, 0.8138888888888888840, 0.8166666666666666519, 0.8194444444444444198, 0.8222222222222221877, 0.8249999999999999556, 0.8277777777777777235, 0.8305555555555556024, 0.8333333333333333703, 0.8361111111111111382, 0.8388888888888889062, 0.8416666666666666741, 0.8444444444444444420, 0.8472222222222222099, 0.8499999999999999778, 0.8527777777777777457, 0.8555555555555555136, 0.8583333333333332815, 0.8611111111111111605, 0.8638888888888889284, 0.8666666666666666963, 0.8694444444444444642, 0.8722222222222222321, 0.8750000000000000000, 0.8777777777777777679, 0.8805555555555555358, 0.8833333333333333037, 0.8861111111111110716, 0.8888888888888888395, 0.8916666666666667185, 0.8944444444444444864, 0.8972222222222222543, 0.9000000000000000222, 0.9027777777777777901, 0.9055555555555555580, 0.9083333333333333259, 0.9111111111111110938, 0.9138888888888888618, 0.9166666666666666297, 0.9194444444444443976, 0.9222222222222222765, 0.9250000000000000444, 0.9277777777777778123, 0.9305555555555555802, 0.9333333333333333481, 0.9361111111111111160, 0.9388888888888888840, 0.9416666666666666519, 0.9444444444444444198, 0.9472222222222221877, 0.9499999999999999556, 0.9527777777777777235, 0.9555555555555556024, 0.9583333333333333703, 0.9611111111111111382, 0.9638888888888889062, 0.9666666666666666741, 0.9694444444444444420, 0.9722222222222222099, 0.9749999999999999778, 0.9777777777777777457, 0.9805555555555555136, 0.9833333333333332815, 0.9861111111111111605, 0.9888888888888889284, 0.9916666666666666963, 0.9944444444444444642, 0.9972222222222222321, 1.000000000000000000 ),
 .UNSPECIFIED. ) 
 GEOMETRIC_REPRESENTATION_ITEM ( )  RATIONAL_B_SPLINE_SURFACE ( (
 ( 1.000000000000000000, 0.8660254037844387076, 1.000000000000000000, 0.8660254037844387076, 1.000000000000000000, 0.8660254037844387076, 1.000000000000000000, 0.8660254037844387076, 1.000000000000000000, 0.8660254037844387076, 1.000000000000000000, 0.8660254037844387076, 1.000000000000000000, 0.8660254037844387076, 1.000000000000000000, 0.8660254037844387076, 1.000000000000000000, 0.8660254037844387076, 1.000000000000000000, 0.8660254037844387076, 1.000000000000000000, 0.8660254037844387076, 1.000000000000000000, 0.8660254037844387076, 1.000000000000000000, 0.8660254037844387076, 1.000000000000000000, 0.8660254037844387076, 1.000000000000000000, 0.8660254037844387076, 1.000000000000000000, 0.8660254037844387076, 1.000000000000000000, 0.8660254037844387076, 1.000000000000000000, 0.8660254037844387076, 1.000000000000000000, 0.8660254037844387076, 1.000000000000000000, 0.8660254037844387076, 1.000000000000000000, 0.8660254037844387076, 1.000000000000000000, 0.8660254037844387076, 1.000000000000000000, 0.8660254037844387076, 1.000000000000000000, 0.8660254037844387076, 1.000000000000000000, 0.8660254037844387076, 1.000000000000000000, 0.8660254037844387076, 1.000000000000000000, 0.8660254037844387076, 1.000000000000000000, 0.8660254037844387076, 1.000000000000000000, 0.8660254037844387076, 1.000000000000000000, 0.8660254037844387076, 1.000000000000000000, 0.8660254037844387076, 1.000000000000000000, 0.8660254037844387076, 1.000000000000000000, 0.8660254037844387076, 1.000000000000000000, 0.8660254037844387076, 1.000000000000000000, 0.8660254037844387076, 1.000000000000000000, 0.8660254037844387076, 1.000000000000000000, 0.8660254037844387076, 1.000000000000000000, 0.8660254037844387076, 1.000000000000000000, 0.8660254037844387076, 1.000000000000000000, 0.8660254037844387076, 1.000000000000000000, 0.8660254037844387076, 1.000000000000000000, 0.8660254037844387076, 1.000000000000000000, 0.8660254037844387076, 1.000000000000000000, 0.8660254037844387076, 1.000000000000000000, 0.8660254037844387076, 1.000000000000000000, 0.8660254037844387076, 1.000000000000000000, 0.8660254037844387076, 1.000000000000000000, 0.8660254037844387076, 1.000000000000000000, 0.8660254037844387076, 1.000000000000000000, 0.8660254037844387076, 1.000000000000000000, 0.8660254037844387076, 1.000000000000000000, 0.8660254037844387076, 1.000000000000000000, 0.8660254037844387076, 1.000000000000000000, 0.8660254037844387076, 1.000000000000000000, 0.8660254037844387076, 1.000000000000000000, 0.8660254037844387076, 1.000000000000000000, 0.8660254037844387076, 1.000000000000000000, 0.8660254037844387076, 1.000000000000000000, 0.8660254037844387076, 1.000000000000000000, 0.8660254037844387076, 1.000000000000000000, 0.8660254037844387076, 1.000000000000000000, 0.8660254037844387076, 1.000000000000000000, 0.8660254037844387076, 1.000000000000000000, 0.8660254037844387076, 1.000000000000000000, 0.8660254037844387076, 1.000000000000000000, 0.8660254037844387076, 1.000000000000000000, 0.8660254037844387076, 1.000000000000000000, 0.8660254037844387076, 1.000000000000000000, 0.8660254037844387076, 1.000000000000000000, 0.8660254037844387076, 1.000000000000000000, 0.8660254037844387076, 1.000000000000000000, 0.8660254037844387076, 1.000000000000000000, 0.8660254037844387076, 1.000000000000000000, 0.8660254037844387076, 1.000000000000000000, 0.8660254037844387076, 1.000000000000000000, 0.8660254037844387076, 1.000000000000000000, 0.8660254037844387076, 1.000000000000000000, 0.8660254037844387076, 1.000000000000000000, 0.8660254037844387076, 1.000000000000000000, 0.8660254037844387076, 1.000000000000000000, 0.8660254037844387076, 1.000000000000000000, 0.8660254037844387076, 1.000000000000000000, 0.8660254037844387076, 1.000000000000000000, 0.8660254037844387076, 1.000000000000000000, 0.8660254037844387076, 1.000000000000000000, 0.8660254037844387076, 1.000000000000000000, 0.8660254037844387076, 1.000000000000000000, 0.8660254037844387076, 1.000000000000000000, 0.8660254037844387076, 1.000000000000000000, 0.8660254037844387076, 1.000000000000000000, 0.8660254037844387076, 1.000000000000000000, 0.8660254037844387076, 1.000000000000000000, 0.8660254037844387076, 1.000000000000000000, 0.8660254037844387076, 1.000000000000000000, 0.8660254037844387076, 1.000000000000000000, 0.8660254037844387076, 1.000000000000000000, 0.8660254037844387076, 1.000000000000000000, 0.8660254037844387076, 1.000000000000000000, 0.8660254037844387076, 1.000000000000000000, 0.8660254037844387076, 1.000000000000000000, 0.8660254037844387076, 1.000000000000000000, 0.8660254037844387076, 1.000000000000000000, 0.8660254037844387076, 1.000000000000000000, 0.8660254037844387076, 1.000000000000000000, 0.8660254037844387076, 1.000000000000000000, 0.8660254037844387076, 1.000000000000000000, 0.8660254037844387076, 1.000000000000000000, 0.8660254037844387076, 1.000000000000000000, 0.8660254037844387076, 1.000000000000000000, 0.8660254037844387076, 1.000000000000000000, 0.8660254037844387076, 1.000000000000000000, 0.8660254037844387076, 1.000000000000000000, 0.8660254037844387076, 1.000000000000000000, 0.8660254037844387076, 1.000000000000000000, 0.8660254037844387076, 1.000000000000000000, 0.8660254037844387076, 1.000000000000000000, 0.8660254037844387076, 1.000000000000000000, 0.8660254037844387076, 1.000000000000000000, 0.8660254037844387076, 1.000000000000000000, 0.8660254037844387076, 1.000000000000000000, 0.8660254037844387076, 1.000000000000000000, 0.8660254037844387076, 1.000000000000000000, 0.8660254037844387076, 1.000000000000000000, 0.8660254037844387076, 1.000000000000000000, 0.8660254037844387076, 1.000000000000000000, 0.8660254037844387076, 1.000000000000000000, 0.8660254037844387076, 1.000000000000000000, 0.8660254037844387076, 1.000000000000000000, 0.8660254037844387076, 1.000000000000000000, 0.8660254037844387076, 1.000000000000000000, 0.8660254037844387076, 1.000000000000000000, 0.8660254037844387076, 1.000000000000000000, 0.8660254037844387076, 1.000000000000000000, 0.8660254037844387076, 1.000000000000000000, 0.8660254037844387076, 1.000000000000000000, 0.8660254037844387076, 1.000000000000000000, 0.8660254037844387076, 1.000000000000000000, 0.8660254037844387076, 1.000000000000000000, 0.8660254037844387076, 1.000000000000000000, 0.8660254037844387076, 1.000000000000000000, 0.8660254037844387076, 1.000000000000000000, 0.8660254037844387076, 1.000000000000000000, 0.8660254037844387076, 1.000000000000000000, 0.8660254037844387076, 1.000000000000000000, 0.8660254037844387076, 1.000000000000000000, 0.8660254037844387076, 1.000000000000000000, 0.8660254037844387076, 1.000000000000000000, 0.8660254037844387076, 1.000000000000000000, 0.8660254037844387076, 1.000000000000000000, 0.8660254037844387076, 1.000000000000000000, 0.8660254037844387076, 1.000000000000000000, 0.8660254037844387076, 1.000000000000000000, 0.8660254037844387076, 1.000000000000000000, 0.8660254037844387076, 1.000000000000000000, 0.8660254037844387076, 1.000000000000000000, 0.8660254037844387076, 1.000000000000000000, 0.8660254037844387076, 1.000000000000000000, 0.8660254037844387076, 1.000000000000000000, 0.8660254037844387076, 1.000000000000000000, 0.8660254037844387076, 1.000000000000000000, 0.8660254037844387076, 1.000000000000000000, 0.8660254037844387076, 1.000000000000000000, 0.8660254037844387076, 1.000000000000000000, 0.8660254037844387076, 1.000000000000000000, 0.8660254037844387076, 1.000000000000000000, 0.8660254037844387076, 1.000000000000000000, 0.8660254037844387076, 1.000000000000000000, 0.8660254037844387076, 1.000000000000000000, 0.8660254037844387076, 1.000000000000000000, 0.8660254037844387076, 1.000000000000000000, 0.8660254037844387076, 1.000000000000000000, 0.8660254037844387076, 1.000000000000000000, 0.8660254037844387076, 1.000000000000000000, 0.8660254037844387076, 1.000000000000000000, 0.8660254037844387076, 1.000000000000000000, 0.8660254037844387076, 1.000000000000000000, 0.8660254037844387076, 1.000000000000000000, 0.8660254037844387076, 1.000000000000000000, 0.8660254037844387076, 1.000000000000000000, 0.8660254037844387076, 1.000000000000000000, 0.8660254037844387076, 1.000000000000000000, 0.8660254037844387076, 1.000000000000000000, 0.8660254037844387076, 1.000000000000000000, 0.8660254037844387076, 1.000000000000000000, 0.8660254037844387076, 1.000000000000000000, 0.8660254037844387076, 1.000000000000000000, 0.8660254037844387076, 1.000000000000000000, 0.8660254037844387076, 1.000000000000000000, 0.8660254037844387076, 1.000000000000000000, 0.8660254037844387076, 1.000000000000000000, 0.8660254037844387076, 1.000000000000000000, 0.8660254037844387076, 1.000000000000000000, 0.8660254037844387076, 1.000000000000000000, 0.8660254037844387076, 1.000000000000000000, 0.8660254037844387076, 1.000000000000000000, 0.8660254037844387076, 1.000000000000000000, 0.8660254037844387076, 1.000000000000000000, 0.8660254037844387076, 1.000000000000000000, 0.8660254037844387076, 1.000000000000000000, 0.8660254037844387076, 1.000000000000000000, 0.8660254037844387076, 1.000000000000000000, 0.8660254037844387076, 1.000000000000000000, 0.8660254037844387076, 1.000000000000000000, 0.8660254037844387076, 1.000000000000000000, 0.8660254037844387076, 1.000000000000000000, 0.8660254037844387076, 1.000000000000000000, 0.8660254037844387076, 1.000000000000000000, 0.8660254037844387076, 1.000000000000000000, 0.8660254037844387076, 1.000000000000000000, 0.8660254037844387076, 1.000000000000000000, 0.8660254037844387076, 1.000000000000000000, 0.8660254037844387076, 1.000000000000000000, 0.8660254037844387076, 1.000000000000000000, 0.8660254037844387076, 1.000000000000000000, 0.8660254037844387076, 1.000000000000000000, 0.8660254037844387076, 1.000000000000000000, 0.8660254037844387076, 1.000000000000000000, 0.8660254037844387076, 1.000000000000000000, 0.8660254037844387076, 1.000000000000000000, 0.8660254037844387076, 1.000000000000000000, 0.8660254037844387076, 1.000000000000000000, 0.8660254037844387076, 1.000000000000000000, 0.8660254037844387076, 1.000000000000000000, 0.8660254037844387076, 1.000000000000000000, 0.8660254037844387076, 1.000000000000000000, 0.8660254037844387076, 1.000000000000000000, 0.8660254037844387076, 1.000000000000000000, 0.8660254037844387076, 1.000000000000000000, 0.8660254037844387076, 1.000000000000000000, 0.8660254037844387076, 1.000000000000000000, 0.8660254037844387076, 1.000000000000000000, 0.8660254037844387076, 1.000000000000000000, 0.8660254037844387076, 1.000000000000000000, 0.8660254037844387076, 1.000000000000000000, 0.8660254037844387076, 1.000000000000000000, 0.8660254037844387076, 1.000000000000000000, 0.8660254037844387076, 1.000000000000000000, 0.8660254037844387076, 1.000000000000000000, 0.8660254037844387076, 1.000000000000000000, 0.8660254037844387076, 1.000000000000000000, 0.8660254037844387076, 1.000000000000000000, 0.8660254037844387076, 1.000000000000000000, 0.8660254037844387076, 1.000000000000000000, 0.8660254037844387076, 1.000000000000000000, 0.8660254037844387076, 1.000000000000000000, 0.8660254037844387076, 1.000000000000000000, 0.8660254037844387076, 1.000000000000000000, 0.8660254037844387076, 1.000000000000000000, 0.8660254037844387076, 1.000000000000000000, 0.8660254037844387076, 1.000000000000000000, 0.8660254037844387076, 1.000000000000000000, 0.8660254037844387076, 1.000000000000000000, 0.8660254037844387076, 1.000000000000000000, 0.8660254037844387076, 1.000000000000000000, 0.8660254037844387076, 1.000000000000000000, 0.8660254037844387076, 1.000000000000000000, 0.8660254037844387076, 1.000000000000000000, 0.8660254037844387076, 1.000000000000000000, 0.8660254037844387076, 1.000000000000000000, 0.8660254037844387076, 1.000000000000000000, 0.8660254037844387076, 1.000000000000000000, 0.8660254037844387076, 1.000000000000000000, 0.8660254037844387076, 1.000000000000000000, 0.8660254037844387076, 1.000000000000000000, 0.8660254037844387076, 1.000000000000000000, 0.8660254037844387076, 1.000000000000000000, 0.8660254037844387076, 1.000000000000000000, 0.8660254037844387076, 1.000000000000000000, 0.8660254037844387076, 1.000000000000000000, 0.8660254037844387076, 1.000000000000000000, 0.8660254037844387076, 1.000000000000000000, 0.8660254037844387076, 1.000000000000000000, 0.8660254037844387076, 1.000000000000000000, 0.8660254037844387076, 1.000000000000000000, 0.8660254037844387076, 1.000000000000000000, 0.8660254037844387076, 1.000000000000000000, 0.8660254037844387076, 1.000000000000000000, 0.8660254037844387076, 1.000000000000000000, 0.8660254037844387076, 1.000000000000000000, 0.8660254037844387076, 1.000000000000000000, 0.8660254037844387076, 1.000000000000000000, 0.8660254037844387076, 1.000000000000000000, 0.8660254037844387076, 1.000000000000000000, 0.8660254037844387076, 1.000000000000000000, 0.8660254037844387076, 1.000000000000000000, 0.8660254037844387076, 1.000000000000000000, 0.8660254037844387076, 1.000000000000000000, 0.8660254037844387076, 1.000000000000000000, 0.8660254037844387076, 1.000000000000000000, 0.8660254037844387076, 1.000000000000000000, 0.8660254037844387076, 1.000000000000000000, 0.8660254037844387076, 1.000000000000000000, 0.8660254037844387076, 1.000000000000000000, 0.8660254037844387076, 1.000000000000000000, 0.8660254037844387076, 1.000000000000000000, 0.8660254037844387076, 1.000000000000000000, 0.8660254037844387076, 1.000000000000000000, 0.8660254037844387076, 1.000000000000000000, 0.8660254037844387076, 1.000000000000000000, 0.8660254037844387076, 1.000000000000000000, 0.8660254037844387076, 1.000000000000000000, 0.8660254037844387076, 1.000000000000000000, 0.8660254037844387076, 1.000000000000000000, 0.8660254037844387076, 1.000000000000000000, 0.8660254037844387076, 1.000000000000000000, 0.8660254037844387076, 1.000000000000000000, 0.8660254037844387076, 1.000000000000000000, 0.8660254037844387076, 1.000000000000000000, 0.8660254037844387076, 1.000000000000000000, 0.8660254037844387076, 1.000000000000000000, 0.8660254037844387076, 1.000000000000000000, 0.8660254037844387076, 1.000000000000000000, 0.8660254037844387076, 1.000000000000000000, 0.8660254037844387076, 1.000000000000000000, 0.8660254037844387076, 1.000000000000000000, 0.8660254037844387076, 1.000000000000000000, 0.8660254037844387076, 1.000000000000000000, 0.8660254037844387076, 1.000000000000000000, 0.8660254037844387076, 1.000000000000000000, 0.8660254037844387076, 1.000000000000000000, 0.8660254037844387076, 1.000000000000000000, 0.8660254037844387076, 1.000000000000000000, 0.8660254037844387076, 1.000000000000000000, 0.8660254037844387076, 1.000000000000000000, 0.8660254037844387076, 1.000000000000000000, 0.8660254037844387076, 1.000000000000000000, 0.8660254037844387076, 1.000000000000000000, 0.8660254037844387076, 1.000000000000000000, 0.8660254037844387076, 1.000000000000000000, 0.8660254037844387076, 1.000000000000000000, 0.8660254037844387076, 1.000000000000000000, 0.8660254037844387076, 1.000000000000000000, 0.8660254037844387076, 1.000000000000000000, 0.8660254037844387076, 1.000000000000000000, 0.8660254037844387076, 1.000000000000000000, 0.8660254037844387076, 1.000000000000000000, 0.8660254037844387076, 1.000000000000000000, 0.8660254037844387076, 1.000000000000000000, 0.8660254037844387076, 1.000000000000000000, 0.8660254037844387076, 1.000000000000000000, 0.8660254037844387076, 1.000000000000000000, 0.8660254037844387076, 1.000000000000000000, 0.8660254037844387076, 1.000000000000000000, 0.8660254037844387076, 1.000000000000000000, 0.8660254037844387076, 1.000000000000000000, 0.8660254037844387076, 1.000000000000000000, 0.8660254037844387076, 1.000000000000000000, 0.8660254037844387076, 1.000000000000000000, 0.8660254037844387076, 1.000000000000000000, 0.8660254037844387076, 1.000000000000000000, 0.8660254037844387076, 1.000000000000000000, 0.8660254037844387076, 1.000000000000000000, 0.8660254037844387076, 1.000000000000000000, 0.8660254037844387076, 1.000000000000000000, 0.8660254037844387076, 1.000000000000000000, 0.8660254037844387076, 1.000000000000000000, 0.8660254037844387076, 1.000000000000000000, 0.8660254037844387076, 1.000000000000000000, 0.8660254037844387076, 1.000000000000000000, 0.8660254037844387076, 1.000000000000000000),
 ( 1.000000000000000000, 0.8660254037844387076, 1.000000000000000000, 0.8660254037844387076, 1.000000000000000000, 0.8660254037844387076, 1.000000000000000000, 0.8660254037844387076, 1.000000000000000000, 0.8660254037844387076, 1.000000000000000000, 0.8660254037844387076, 1.000000000000000000, 0.8660254037844387076, 1.000000000000000000, 0.8660254037844387076, 1.000000000000000000, 0.8660254037844387076, 1.000000000000000000, 0.8660254037844387076, 1.000000000000000000, 0.8660254037844387076, 1.000000000000000000, 0.8660254037844387076, 1.000000000000000000, 0.8660254037844387076, 1.000000000000000000, 0.8660254037844387076, 1.000000000000000000, 0.8660254037844387076, 1.000000000000000000, 0.8660254037844387076, 1.000000000000000000, 0.8660254037844387076, 1.000000000000000000, 0.8660254037844387076, 1.000000000000000000, 0.8660254037844387076, 1.000000000000000000, 0.8660254037844387076, 1.000000000000000000, 0.8660254037844387076, 1.000000000000000000, 0.8660254037844387076, 1.000000000000000000, 0.8660254037844387076, 1.000000000000000000, 0.8660254037844387076, 1.000000000000000000, 0.8660254037844387076, 1.000000000000000000, 0.8660254037844387076, 1.000000000000000000, 0.8660254037844387076, 1.000000000000000000, 0.8660254037844387076, 1.000000000000000000, 0.8660254037844387076, 1.000000000000000000, 0.8660254037844387076, 1.000000000000000000, 0.8660254037844387076, 1.000000000000000000, 0.8660254037844387076, 1.000000000000000000, 0.8660254037844387076, 1.000000000000000000, 0.8660254037844387076, 1.000000000000000000, 0.8660254037844387076, 1.000000000000000000, 0.8660254037844387076, 1.000000000000000000, 0.8660254037844387076, 1.000000000000000000, 0.8660254037844387076, 1.000000000000000000, 0.8660254037844387076, 1.000000000000000000, 0.8660254037844387076, 1.000000000000000000, 0.8660254037844387076, 1.000000000000000000, 0.8660254037844387076, 1.000000000000000000, 0.8660254037844387076, 1.000000000000000000, 0.8660254037844387076, 1.000000000000000000, 0.8660254037844387076, 1.000000000000000000, 0.8660254037844387076, 1.000000000000000000, 0.8660254037844387076, 1.000000000000000000, 0.8660254037844387076, 1.000000000000000000, 0.8660254037844387076, 1.000000000000000000, 0.8660254037844387076, 1.000000000000000000, 0.8660254037844387076, 1.000000000000000000, 0.8660254037844387076, 1.000000000000000000, 0.8660254037844387076, 1.000000000000000000, 0.8660254037844387076, 1.000000000000000000, 0.8660254037844387076, 1.000000000000000000, 0.8660254037844387076, 1.000000000000000000, 0.8660254037844387076, 1.000000000000000000, 0.8660254037844387076, 1.000000000000000000, 0.8660254037844387076, 1.000000000000000000, 0.8660254037844387076, 1.000000000000000000, 0.8660254037844387076, 1.000000000000000000, 0.8660254037844387076, 1.000000000000000000, 0.8660254037844387076, 1.000000000000000000, 0.8660254037844387076, 1.000000000000000000, 0.8660254037844387076, 1.000000000000000000, 0.8660254037844387076, 1.000000000000000000, 0.8660254037844387076, 1.000000000000000000, 0.8660254037844387076, 1.000000000000000000, 0.8660254037844387076, 1.000000000000000000, 0.8660254037844387076, 1.000000000000000000, 0.8660254037844387076, 1.000000000000000000, 0.8660254037844387076, 1.000000000000000000, 0.8660254037844387076, 1.000000000000000000, 0.8660254037844387076, 1.000000000000000000, 0.8660254037844387076, 1.000000000000000000, 0.8660254037844387076, 1.000000000000000000, 0.8660254037844387076, 1.000000000000000000, 0.8660254037844387076, 1.000000000000000000, 0.8660254037844387076, 1.000000000000000000, 0.8660254037844387076, 1.000000000000000000, 0.8660254037844387076, 1.000000000000000000, 0.8660254037844387076, 1.000000000000000000, 0.8660254037844387076, 1.000000000000000000, 0.8660254037844387076, 1.000000000000000000, 0.8660254037844387076, 1.000000000000000000, 0.8660254037844387076, 1.000000000000000000, 0.8660254037844387076, 1.000000000000000000, 0.8660254037844387076, 1.000000000000000000, 0.8660254037844387076, 1.000000000000000000, 0.8660254037844387076, 1.000000000000000000, 0.8660254037844387076, 1.000000000000000000, 0.8660254037844387076, 1.000000000000000000, 0.8660254037844387076, 1.000000000000000000, 0.8660254037844387076, 1.000000000000000000, 0.8660254037844387076, 1.000000000000000000, 0.8660254037844387076, 1.000000000000000000, 0.8660254037844387076, 1.000000000000000000, 0.8660254037844387076, 1.000000000000000000, 0.8660254037844387076, 1.000000000000000000, 0.8660254037844387076, 1.000000000000000000, 0.8660254037844387076, 1.000000000000000000, 0.8660254037844387076, 1.000000000000000000, 0.8660254037844387076, 1.000000000000000000, 0.8660254037844387076, 1.000000000000000000, 0.8660254037844387076, 1.000000000000000000, 0.8660254037844387076, 1.000000000000000000, 0.8660254037844387076, 1.000000000000000000, 0.8660254037844387076, 1.000000000000000000, 0.8660254037844387076, 1.000000000000000000, 0.8660254037844387076, 1.000000000000000000, 0.8660254037844387076, 1.000000000000000000, 0.8660254037844387076, 1.000000000000000000, 0.8660254037844387076, 1.000000000000000000, 0.8660254037844387076, 1.000000000000000000, 0.8660254037844387076, 1.000000000000000000, 0.8660254037844387076, 1.000000000000000000, 0.8660254037844387076, 1.000000000000000000, 0.8660254037844387076, 1.000000000000000000, 0.8660254037844387076, 1.000000000000000000, 0.8660254037844387076, 1.000000000000000000, 0.8660254037844387076, 1.000000000000000000, 0.8660254037844387076, 1.000000000000000000, 0.8660254037844387076, 1.000000000000000000, 0.8660254037844387076, 1.000000000000000000, 0.8660254037844387076, 1.000000000000000000, 0.8660254037844387076, 1.000000000000000000, 0.8660254037844387076, 1.000000000000000000, 0.8660254037844387076, 1.000000000000000000, 0.8660254037844387076, 1.000000000000000000, 0.8660254037844387076, 1.000000000000000000, 0.8660254037844387076, 1.000000000000000000, 0.8660254037844387076, 1.000000000000000000, 0.8660254037844387076, 1.000000000000000000, 0.8660254037844387076, 1.000000000000000000, 0.8660254037844387076, 1.000000000000000000, 0.8660254037844387076, 1.000000000000000000, 0.8660254037844387076, 1.000000000000000000, 0.8660254037844387076, 1.000000000000000000, 0.8660254037844387076, 1.000000000000000000, 0.8660254037844387076, 1.000000000000000000, 0.8660254037844387076, 1.000000000000000000, 0.8660254037844387076, 1.000000000000000000, 0.8660254037844387076, 1.000000000000000000, 0.8660254037844387076, 1.000000000000000000, 0.8660254037844387076, 1.000000000000000000, 0.8660254037844387076, 1.000000000000000000, 0.8660254037844387076, 1.000000000000000000, 0.8660254037844387076, 1.000000000000000000, 0.8660254037844387076, 1.000000000000000000, 0.8660254037844387076, 1.000000000000000000, 0.8660254037844387076, 1.000000000000000000, 0.8660254037844387076, 1.000000000000000000, 0.8660254037844387076, 1.000000000000000000, 0.8660254037844387076, 1.000000000000000000, 0.8660254037844387076, 1.000000000000000000, 0.8660254037844387076, 1.000000000000000000, 0.8660254037844387076, 1.000000000000000000, 0.8660254037844387076, 1.000000000000000000, 0.8660254037844387076, 1.000000000000000000, 0.8660254037844387076, 1.000000000000000000, 0.8660254037844387076, 1.000000000000000000, 0.8660254037844387076, 1.000000000000000000, 0.8660254037844387076, 1.000000000000000000, 0.8660254037844387076, 1.000000000000000000, 0.8660254037844387076, 1.000000000000000000, 0.8660254037844387076, 1.000000000000000000, 0.8660254037844387076, 1.000000000000000000, 0.8660254037844387076, 1.000000000000000000, 0.8660254037844387076, 1.000000000000000000, 0.8660254037844387076, 1.000000000000000000, 0.8660254037844387076, 1.000000000000000000, 0.8660254037844387076, 1.000000000000000000, 0.8660254037844387076, 1.000000000000000000, 0.8660254037844387076, 1.000000000000000000, 0.8660254037844387076, 1.000000000000000000, 0.8660254037844387076, 1.000000000000000000, 0.8660254037844387076, 1.000000000000000000, 0.8660254037844387076, 1.000000000000000000, 0.8660254037844387076, 1.000000000000000000, 0.8660254037844387076, 1.000000000000000000, 0.8660254037844387076, 1.000000000000000000, 0.8660254037844387076, 1.000000000000000000, 0.8660254037844387076, 1.000000000000000000, 0.8660254037844387076, 1.000000000000000000, 0.8660254037844387076, 1.000000000000000000, 0.8660254037844387076, 1.000000000000000000, 0.8660254037844387076, 1.000000000000000000, 0.8660254037844387076, 1.000000000000000000, 0.8660254037844387076, 1.000000000000000000, 0.8660254037844387076, 1.000000000000000000, 0.8660254037844387076, 1.000000000000000000, 0.8660254037844387076, 1.000000000000000000, 0.8660254037844387076, 1.000000000000000000, 0.8660254037844387076, 1.000000000000000000, 0.8660254037844387076, 1.000000000000000000, 0.8660254037844387076, 1.000000000000000000, 0.8660254037844387076, 1.000000000000000000, 0.8660254037844387076, 1.000000000000000000, 0.8660254037844387076, 1.000000000000000000, 0.8660254037844387076, 1.000000000000000000, 0.8660254037844387076, 1.000000000000000000, 0.8660254037844387076, 1.000000000000000000, 0.8660254037844387076, 1.000000000000000000, 0.8660254037844387076, 1.000000000000000000, 0.8660254037844387076, 1.000000000000000000, 0.8660254037844387076, 1.000000000000000000, 0.8660254037844387076, 1.000000000000000000, 0.8660254037844387076, 1.000000000000000000, 0.8660254037844387076, 1.000000000000000000, 0.8660254037844387076, 1.000000000000000000, 0.8660254037844387076, 1.000000000000000000, 0.8660254037844387076, 1.000000000000000000, 0.8660254037844387076, 1.000000000000000000, 0.8660254037844387076, 1.000000000000000000, 0.8660254037844387076, 1.000000000000000000, 0.8660254037844387076, 1.000000000000000000, 0.8660254037844387076, 1.000000000000000000, 0.8660254037844387076, 1.000000000000000000, 0.8660254037844387076, 1.000000000000000000, 0.8660254037844387076, 1.000000000000000000, 0.8660254037844387076, 1.000000000000000000, 0.8660254037844387076, 1.000000000000000000, 0.8660254037844387076, 1.000000000000000000, 0.8660254037844387076, 1.000000000000000000, 0.8660254037844387076, 1.000000000000000000, 0.8660254037844387076, 1.000000000000000000, 0.8660254037844387076, 1.000000000000000000, 0.8660254037844387076, 1.000000000000000000, 0.8660254037844387076, 1.000000000000000000, 0.8660254037844387076, 1.000000000000000000, 0.8660254037844387076, 1.000000000000000000, 0.8660254037844387076, 1.000000000000000000, 0.8660254037844387076, 1.000000000000000000, 0.8660254037844387076, 1.000000000000000000, 0.8660254037844387076, 1.000000000000000000, 0.8660254037844387076, 1.000000000000000000, 0.8660254037844387076, 1.000000000000000000, 0.8660254037844387076, 1.000000000000000000, 0.8660254037844387076, 1.000000000000000000, 0.8660254037844387076, 1.000000000000000000, 0.8660254037844387076, 1.000000000000000000, 0.8660254037844387076, 1.000000000000000000, 0.8660254037844387076, 1.000000000000000000, 0.8660254037844387076, 1.000000000000000000, 0.8660254037844387076, 1.000000000000000000, 0.8660254037844387076, 1.000000000000000000, 0.8660254037844387076, 1.000000000000000000, 0.8660254037844387076, 1.000000000000000000, 0.8660254037844387076, 1.000000000000000000, 0.8660254037844387076, 1.000000000000000000, 0.8660254037844387076, 1.000000000000000000, 0.8660254037844387076, 1.000000000000000000, 0.8660254037844387076, 1.000000000000000000, 0.8660254037844387076, 1.000000000000000000, 0.8660254037844387076, 1.000000000000000000, 0.8660254037844387076, 1.000000000000000000, 0.8660254037844387076, 1.000000000000000000, 0.8660254037844387076, 1.000000000000000000, 0.8660254037844387076, 1.000000000000000000, 0.8660254037844387076, 1.000000000000000000, 0.8660254037844387076, 1.000000000000000000, 0.8660254037844387076, 1.000000000000000000, 0.8660254037844387076, 1.000000000000000000, 0.8660254037844387076, 1.000000000000000000, 0.8660254037844387076, 1.000000000000000000, 0.8660254037844387076, 1.000000000000000000, 0.8660254037844387076, 1.000000000000000000, 0.8660254037844387076, 1.000000000000000000, 0.8660254037844387076, 1.000000000000000000, 0.8660254037844387076, 1.000000000000000000, 0.8660254037844387076, 1.000000000000000000, 0.8660254037844387076, 1.000000000000000000, 0.8660254037844387076, 1.000000000000000000, 0.8660254037844387076, 1.000000000000000000, 0.8660254037844387076, 1.000000000000000000, 0.8660254037844387076, 1.000000000000000000, 0.8660254037844387076, 1.000000000000000000, 0.8660254037844387076, 1.000000000000000000, 0.8660254037844387076, 1.000000000000000000, 0.8660254037844387076, 1.000000000000000000, 0.8660254037844387076, 1.000000000000000000, 0.8660254037844387076, 1.000000000000000000, 0.8660254037844387076, 1.000000000000000000, 0.8660254037844387076, 1.000000000000000000, 0.8660254037844387076, 1.000000000000000000, 0.8660254037844387076, 1.000000000000000000, 0.8660254037844387076, 1.000000000000000000, 0.8660254037844387076, 1.000000000000000000, 0.8660254037844387076, 1.000000000000000000, 0.8660254037844387076, 1.000000000000000000, 0.8660254037844387076, 1.000000000000000000, 0.8660254037844387076, 1.000000000000000000, 0.8660254037844387076, 1.000000000000000000, 0.8660254037844387076, 1.000000000000000000, 0.8660254037844387076, 1.000000000000000000, 0.8660254037844387076, 1.000000000000000000, 0.8660254037844387076, 1.000000000000000000, 0.8660254037844387076, 1.000000000000000000, 0.8660254037844387076, 1.000000000000000000, 0.8660254037844387076, 1.000000000000000000, 0.8660254037844387076, 1.000000000000000000, 0.8660254037844387076, 1.000000000000000000, 0.8660254037844387076, 1.000000000000000000, 0.8660254037844387076, 1.000000000000000000, 0.8660254037844387076, 1.000000000000000000, 0.8660254037844387076, 1.000000000000000000, 0.8660254037844387076, 1.000000000000000000, 0.8660254037844387076, 1.000000000000000000, 0.8660254037844387076, 1.000000000000000000, 0.8660254037844387076, 1.000000000000000000, 0.8660254037844387076, 1.000000000000000000, 0.8660254037844387076, 1.000000000000000000, 0.8660254037844387076, 1.000000000000000000, 0.8660254037844387076, 1.000000000000000000, 0.8660254037844387076, 1.000000000000000000, 0.8660254037844387076, 1.000000000000000000, 0.8660254037844387076, 1.000000000000000000, 0.8660254037844387076, 1.000000000000000000, 0.8660254037844387076, 1.000000000000000000, 0.8660254037844387076, 1.000000000000000000, 0.8660254037844387076, 1.000000000000000000, 0.8660254037844387076, 1.000000000000000000, 0.8660254037844387076, 1.000000000000000000, 0.8660254037844387076, 1.000000000000000000, 0.8660254037844387076, 1.000000000000000000, 0.8660254037844387076, 1.000000000000000000, 0.8660254037844387076, 1.000000000000000000, 0.8660254037844387076, 1.000000000000000000, 0.8660254037844387076, 1.000000000000000000, 0.8660254037844387076, 1.000000000000000000, 0.8660254037844387076, 1.000000000000000000, 0.8660254037844387076, 1.000000000000000000, 0.8660254037844387076, 1.000000000000000000, 0.8660254037844387076, 1.000000000000000000, 0.8660254037844387076, 1.000000000000000000, 0.8660254037844387076, 1.000000000000000000, 0.8660254037844387076, 1.000000000000000000, 0.8660254037844387076, 1.000000000000000000, 0.8660254037844387076, 1.000000000000000000, 0.8660254037844387076, 1.000000000000000000, 0.8660254037844387076, 1.000000000000000000, 0.8660254037844387076, 1.000000000000000000, 0.8660254037844387076, 1.000000000000000000, 0.8660254037844387076, 1.000000000000000000, 0.8660254037844387076, 1.000000000000000000, 0.8660254037844387076, 1.000000000000000000, 0.8660254037844387076, 1.000000000000000000, 0.8660254037844387076, 1.000000000000000000, 0.8660254037844387076, 1.000000000000000000, 0.8660254037844387076, 1.000000000000000000, 0.8660254037844387076, 1.000000000000000000, 0.8660254037844387076, 1.000000000000000000, 0.8660254037844387076, 1.000000000000000000, 0.8660254037844387076, 1.000000000000000000, 0.8660254037844387076, 1.000000000000000000, 0.8660254037844387076, 1.000000000000000000, 0.8660254037844387076, 1.000000000000000000, 0.8660254037844387076, 1.000000000000000000, 0.8660254037844387076, 1.000000000000000000, 0.8660254037844387076, 1.000000000000000000) ) ) 
 REPRESENTATION_ITEM ( '' )  SURFACE ( )  );
#48591 = CARTESIAN_POINT ( 'NONE',  ( 4.805076099715074989, -1.383418685542648907, 4.830700292553183672 ) ) ;
#48592 = CARTESIAN_POINT ( 'NONE',  ( 19.86562500061451786, 3.027376345333611329, 5.243569643749999010 ) ) ;
#48593 = CARTESIAN_POINT ( 'NONE',  ( 25.17187500061451644, 3.027376345333613106, -5.243569643749998122 ) ) ;
#48594 = CARTESIAN_POINT ( 'NONE',  ( 1.878215178125000495, 20.47812499938548569, 26.74683588394047007 ) ) ;
#48595 = CARTESIAN_POINT ( 'NONE',  ( 3.366080804335946919, -3.697228694398128290, 3.718268762498968094 ) ) ;
#48596 = FACE_OUTER_BOUND ( 'NONE', #26899, .T. ) ;
#48597 = CARTESIAN_POINT ( 'NONE',  ( 6.196875000614515905, -3.027376345333610441, -5.243569643749999898 ) ) ;
#48598 = CARTESIAN_POINT ( 'NONE',  ( 15.36562500061451608, 3.027376345333611329, 5.243569643749999010 ) ) ;
#48599 = CARTESIAN_POINT ( 'NONE',  ( 13.17187500061451999, 3.027376345333611329, 5.243569643749999010 ) ) ;
#48600 = EDGE_LOOP ( 'NONE', ( #1913, #1682, #43488, #63713 ) ) ;
#48601 = CARTESIAN_POINT ( 'NONE',  ( 24.74062500061451786, 6.054752690667223547, 3.707466751127219781E-16 ) ) ;
#48602 = DIRECTION ( 'NONE',  ( -1.000000000000000000, -0.000000000000000000, -0.000000000000000000 ) ) ;
#48603 = CARTESIAN_POINT ( 'NONE',  ( -2.000000000000000000, 11.48750000122903359, -33.46410161513775705 ) ) ;
#48604 = CARTESIAN_POINT ( 'NONE',  ( 13.83749999999999858, -2.886751345948129988, 4.999999999999997335 ) ) ;
#48605 = CARTESIAN_POINT ( 'NONE',  ( 23.58750000122903145, 6.123233995736764310E-16, -4.999999999999998224 ) ) ;
#48606 = CARTESIAN_POINT ( 'NONE',  ( 18.40312500061451573, 4.541064518000418104, -2.621784821874998173 ) ) ;
#48607 = VERTEX_POINT ( 'NONE', #49212 ) ;
#48608 = CARTESIAN_POINT ( 'NONE',  ( 22.12500000000000000, 6.123233995736764310E-16, -4.999999999999998224 ) ) ;
#48609 = CARTESIAN_POINT ( 'NONE',  ( 24.45937500061451786, 0.000000000000000000, 5.243569643749999010 ) ) ;
#48610 = ORIENTED_EDGE ( 'NONE', *, *, #54938, .T. ) ;
#48611 = CARTESIAN_POINT ( 'NONE',  ( 0.000000000000000000, 0.000000000000000000, 50.00000000000000000 ) ) ;
#48612 = CARTESIAN_POINT ( 'NONE',  ( 11.27812500061451573, 4.541064518000418104, 2.621784821874999949 ) ) ;
#48613 = CARTESIAN_POINT ( 'NONE',  ( 3.778125000614519280, -4.541064518000419881, 2.621784821874995952 ) ) ;
#48614 = CARTESIAN_POINT ( 'NONE',  ( 14.63437500061451502, -2.746126346562642428, -4.756430356249999214 ) ) ;
#48615 = CARTESIAN_POINT ( 'NONE',  ( 27.25312500061451360, -4.541064518000417216, -2.621784821875001281 ) ) ;
#48616 = CARTESIAN_POINT ( 'NONE',  ( 18.41250000000000142, -5.773502691896255534, -1.060575238724906372E-15 ) ) ;
#48617 = CARTESIAN_POINT ( 'NONE',  ( 26.25000000000000000, 4.330127018922192761, -2.499999999999997780 ) ) ;
#48618 = CARTESIAN_POINT ( 'NONE',  ( 3.176339285701963888, -3.861459405730729433, 3.176339285701963888 ) ) ;
#48619 = CARTESIAN_POINT ( 'NONE',  ( 7.434375000614519280, -4.541064518000419881, 2.621784821874995952 ) ) ;
#48620 = CARTESIAN_POINT ( 'NONE',  ( 17.59687500061451715, 6.054752690667223547, 3.707466751127219781E-16 ) ) ;
#48621 = DIRECTION ( 'NONE',  ( 0.000000000000000000, 0.000000000000000000, 1.000000000000000000 ) ) ;
#48622 = ORIENTED_EDGE ( 'NONE', *, *, #19782, .T. ) ;
#48623 = CARTESIAN_POINT ( 'NONE',  ( 27.02812500061451573, 4.541064518000418104, 2.621784821874999949 ) ) ;
#48624 = CARTESIAN_POINT ( 'NONE',  ( 28.43437500061451573, 4.541064518000418104, 2.621784821874999949 ) ) ;
#48625 = DIRECTION ( 'NONE',  ( 0.000000000000000000, -1.000000000000000000, 0.000000000000000000 ) ) ;
#48626 = CARTESIAN_POINT ( 'NONE',  ( 13.31250000000000178, 2.886751345948126879, 4.999999999999999112 ) ) ;
#48627 = CARTESIAN_POINT ( 'NONE',  ( 11.54062500061451857, -3.027376345333610441, -5.243569643749999898 ) ) ;
#48628 = CARTESIAN_POINT ( 'NONE',  ( 9.581250001229033586, 6.123233995736764310E-16, -4.999999999999998224 ) ) ;
#48629 = CARTESIAN_POINT ( 'NONE',  ( -4.000000000000000888, 18.10624999877096641, 32.30940107675850470 ) ) ;
#48630 = CARTESIAN_POINT ( 'NONE',  ( 27.96562500061451573, 3.027376345333611329, 5.243569643749999010 ) ) ;
#48631 = CARTESIAN_POINT ( 'NONE',  ( 19.57500000122903216, 2.886751345948129099, -4.999999999999998224 ) ) ;
#48632 = DIRECTION ( 'NONE',  ( -1.000000000000000000, -0.000000000000000000, -0.000000000000000000 ) ) ;
#48633 = CARTESIAN_POINT ( 'NONE',  ( 16.92187500061451999, -5.492252693125287522, -1.008910452111647106E-15 ) ) ;
#48634 = CARTESIAN_POINT ( 'NONE',  ( 5.165625000614518569, -6.054752690667223547, -1.112240025338166033E-15 ) ) ;
#48635 = CARTESIAN_POINT ( 'NONE',  ( 23.03437500061451715, 4.541064518000418104, 2.621784821874999949 ) ) ;
#48636 = CARTESIAN_POINT ( 'NONE',  ( 4.243569643749999898, 16.93437500061451573, 30.00000000000000000 ) ) ;
#48637 = CARTESIAN_POINT ( 'NONE',  ( 23.63437500061451502, -4.541064518000419881, 2.621784821874995952 ) ) ;
#48638 = CARTESIAN_POINT ( 'NONE',  ( 4.650000000000001243, 4.330127018922192761, -2.499999999999997780 ) ) ;
#48639 = CARTESIAN_POINT ( 'NONE',  ( 3.999999999999998668, 11.82500000122903572, 27.69059892324149175 ) ) ;
#48640 = CARTESIAN_POINT ( 'NONE',  ( 12.17812500061451608, 4.541064518000418104, 2.621784821874999949 ) ) ;
#48641 = CARTESIAN_POINT ( 'NONE',  ( 4.125000001229034652, -5.773502691896255534, -1.060575238724906372E-15 ) ) ;
#48642 = AXIS2_PLACEMENT_3D ( 'NONE', #30883, #14618, #20153 ) ;
#48643 = CARTESIAN_POINT ( 'NONE',  ( 10.05937500061451750, 0.000000000000000000, 5.243569643749999010 ) ) ;
#48644 = CYLINDRICAL_SURFACE ( 'NONE', #72573, 4.999999999999998224 ) ;
#48645 = CARTESIAN_POINT ( 'NONE',  ( 9.628125000614517148, -4.541064518000419881, 2.621784821874995952 ) ) ;
#48646 = CARTESIAN_POINT ( 'NONE',  ( 14.55937500061451573, 0.000000000000000000, 5.243569643749999010 ) ) ;
#48647 = CARTESIAN_POINT ( 'NONE',  ( 21.61875000122903145, -5.773502691896255534, -1.060575238724906372E-15 ) ) ;
#48648 = CARTESIAN_POINT ( 'NONE',  ( 21.93750000122903288, 4.330127018922191873, 2.499999999999999556 ) ) ;
#48649 = CARTESIAN_POINT ( 'NONE',  ( 10.99687500061451750, -3.027376345333614438, 5.243569643749998122 ) ) ;
#48650 = CARTESIAN_POINT ( 'NONE',  ( 12.85312500061451502, -4.541064518000417216, -2.621784821875001281 ) ) ;
#48651 = CARTESIAN_POINT ( 'NONE',  ( 28.14375000122903359, 5.773502691896255534, 3.535250795749688894E-16 ) ) ;
#48652 = CARTESIAN_POINT ( 'NONE',  ( 20.44687500061451857, -3.027376345333614438, 5.243569643749998122 ) ) ;
#48653 = CARTESIAN_POINT ( 'NONE',  ( 26.71875000122903288, 2.886751345948115333, -5.000000000000023093 ) ) ;
#48654 =( BOUNDED_CURVE ( )  B_SPLINE_CURVE ( 1, ( #46167, #68707 ),
 .UNSPECIFIED., .F., .F. ) 
 B_SPLINE_CURVE_WITH_KNOTS ( ( 2, 2 ),
 ( 0.000000000000000000, 1.000000000000000000 ),
 .UNSPECIFIED. ) 
 CURVE ( )  GEOMETRIC_REPRESENTATION_ITEM ( )  RATIONAL_B_SPLINE_CURVE ( ( 0.9401540970596797830, 0.9401540970596797830 ) ) 
 REPRESENTATION_ITEM ( '' )  );
#48655 = CARTESIAN_POINT ( 'NONE',  ( -1.351880753582008765, 4.820610340066097343, 26.22604083275753695 ) ) ;
#48656 = CARTESIAN_POINT ( 'NONE',  ( 2.121784821875001281, 14.15937500061451715, -26.32496088578401938 ) ) ;
#48657 = CARTESIAN_POINT ( 'NONE',  ( 16.20000000122903216, -2.886751345948129988, 4.999999999999997335 ) ) ;
#48658 = CARTESIAN_POINT ( 'NONE',  ( 10.28437500061451715, 6.421520780324663323E-16, -5.243569643749999010 ) ) ;
#48659 = CARTESIAN_POINT ( 'NONE',  ( 4.243569643749999898, 18.64062500061451644, -27.54997392385601529 ) ) ;
#48660 = CARTESIAN_POINT ( 'NONE',  ( 18.75000000122903288, 5.773502691896255534, 3.535250795749688894E-16 ) ) ;
#48661 = CARTESIAN_POINT ( 'NONE',  ( 13.75312500061451715, -4.541064518000417216, -2.621784821875001281 ) ) ;
#48662 = VERTEX_POINT ( 'NONE', #54384 ) ;
#48663 = CARTESIAN_POINT ( 'NONE',  ( 16.87500000000000000, 4.330127018922191873, 2.499999999999999556 ) ) ;
#48664 = CARTESIAN_POINT ( 'NONE',  ( 29.32499999999999929, 6.123233995736764310E-16, -4.999999999999998224 ) ) ;
#48665 = CARTESIAN_POINT ( 'NONE',  ( 9.084375000614517859, 4.541064518000418104, 2.621784821874999949 ) ) ;
#48666 = CARTESIAN_POINT ( 'NONE',  ( 1.071796769724488785, 16.85134618820330132, 34.00000000000000000 ) ) ;
#48667 = CARTESIAN_POINT ( 'NONE',  ( 11.40000000122903501, -2.886751345948125991, -5.000000000000000000 ) ) ;
#48668 = CARTESIAN_POINT ( 'NONE',  ( 17.70000000122903216, -2.886751345948125991, -5.000000000000000000 ) ) ;
#48669 = CARTESIAN_POINT ( 'NONE',  ( 15.96562500061451573, -6.054752690667223547, -1.112240025338166033E-15 ) ) ;
#48670 = EDGE_CURVE ( 'NONE', #35381, #1580, #8546, .T. ) ;
#48671 = CARTESIAN_POINT ( 'NONE',  ( 19.56562500061451715, -6.054752690667223547, -1.112240025338166033E-15 ) ) ;
#48672 = CARTESIAN_POINT ( 'NONE',  ( 27.86250000122903359, 0.000000000000000000, 4.999999999999998224 ) ) ;
#48673 =( BOUNDED_CURVE ( )  B_SPLINE_CURVE ( 2, ( #15758, #50491, #38298, #49764, #73017, #60826, #16128, #22401, #16850 ),
 .UNSPECIFIED., .F., .F. ) 
 B_SPLINE_CURVE_WITH_KNOTS ( ( 3, 2, 2, 2, 3 ),
 ( 0.5978260869565217295, 0.6014492753623188470, 0.6086956521739130821, 0.6159420289855072062, 0.6195652173913043237 ),
 .UNSPECIFIED. ) 
 CURVE ( )  GEOMETRIC_REPRESENTATION_ITEM ( )  RATIONAL_B_SPLINE_CURVE ( ( 0.9330127018922194093, 0.9330127018922194093, 1.000000000000000000, 0.8660254037844387076, 1.000000000000000000, 0.8660254037844387076, 1.000000000000000000, 0.9330127018922194093, 0.9330127018922194093 ) ) 
 REPRESENTATION_ITEM ( '' )  );
#48674 = CARTESIAN_POINT ( 'NONE',  ( 3.703125000614516882, 0.000000000000000000, 5.243569643749999010 ) ) ;
#48675 = CARTESIAN_POINT ( 'NONE',  ( 24.48749999999999716, 5.773502691896255534, 3.535250795749688894E-16 ) ) ;
#48676 = CARTESIAN_POINT ( 'NONE',  ( -1.878215178124999163, 12.79062499938548392, 26.74683588394047007 ) ) ;
#48677 = CARTESIAN_POINT ( 'NONE',  ( 29.77499999999999858, 6.123233995736764310E-16, -4.999999999999998224 ) ) ;
#48678 = CARTESIAN_POINT ( 'NONE',  ( 29.29687500061451644, 6.054752690667223547, 3.707466751127219781E-16 ) ) ;
#48679 = CARTESIAN_POINT ( 'NONE',  ( 0.000000000000000000, 20.00000000000000000, 26.00000000000000000 ) ) ;
#48680 = CARTESIAN_POINT ( 'NONE',  ( 12.18750000122903465, -4.330127018922194537, 2.499999999999995559 ) ) ;
#48681 = CARTESIAN_POINT ( 'NONE',  ( 29.29687500061451644, 6.054752690667223547, 3.707466751127219781E-16 ) ) ;
#48682 = CARTESIAN_POINT ( 'NONE',  ( 30.00000000000000000, 0.000000000000000000, 0.000000000000000000 ) ) ;
#48683 = CARTESIAN_POINT ( 'NONE',  ( 6.834375000614518747, 4.541064518000418104, 2.621784821874999949 ) ) ;
#48684 = CARTESIAN_POINT ( 'NONE',  ( 27.02812500061451573, 4.541064518000418104, 2.621784821874999949 ) ) ;
#48685 =( BOUNDED_CURVE ( )  B_SPLINE_CURVE ( 2, ( #59194, #59935, #53674, #48869, #70659, #42589, #37039 ),
 .UNSPECIFIED., .F., .F. ) 
 B_SPLINE_CURVE_WITH_KNOTS ( ( 3, 2, 2, 3 ),
 ( 0.4400000000000000022, 0.4433333333333333570, 0.4466666666666666563, 0.4500000000000000111 ),
 .UNSPECIFIED. ) 
 CURVE ( )  GEOMETRIC_REPRESENTATION_ITEM ( )  RATIONAL_B_SPLINE_CURVE ( ( 1.000000000000000000, 0.8660254037844387076, 1.000000000000000000, 0.8660254037844387076, 1.000000000000000000, 0.8660254037844387076, 1.000000000000000000 ) ) 
 REPRESENTATION_ITEM ( '' )  );
#48686 = CARTESIAN_POINT ( 'NONE',  ( -3.756430356249999214, 13.39062499938548179, 27.83122392262697176 ) ) ;
#48687 = CARTESIAN_POINT ( 'NONE',  ( 4.363395578908656702, -2.441916286472800124, 4.408370384982540635 ) ) ;
#48688 = CARTESIAN_POINT ( 'NONE',  ( 5.784375000614517148, 6.421520780324663323E-16, -5.243569643749999010 ) ) ;
#48689 = CARTESIAN_POINT ( 'NONE',  ( 9.871875000614517504, 3.027376345333613106, -5.243569643749998122 ) ) ;
#48690 = CARTESIAN_POINT ( 'NONE',  ( 4.425000000000001599, -4.330127018922194537, 2.499999999999995559 ) ) ;
#48691 = EDGE_CURVE ( 'NONE', #54526, #427, #44533, .T. ) ;
#48692 = CARTESIAN_POINT ( 'NONE',  ( -2.121784821874996840, 13.57812500061459282, 33.67503911421598417 ) ) ;
#48693 = CARTESIAN_POINT ( 'NONE',  ( 21.86250000000000071, 2.886751345948126879, 4.999999999999999112 ) ) ;
#48694 = CARTESIAN_POINT ( 'NONE',  ( 29.17500000000000071, -4.330127018922194537, 2.499999999999995559 ) ) ;
#48695 = CARTESIAN_POINT ( 'NONE',  ( 4.125000000000000000, 6.123233995736764310E-16, -4.999999999999998224 ) ) ;
#48696 = CARTESIAN_POINT ( 'NONE',  ( 12.87187500061451750, 5.824947211148865298E-16, -4.756430356249998326 ) ) ;
#48697 = ORIENTED_EDGE ( 'NONE', *, *, #62265, .F. ) ;
#48698 = CARTESIAN_POINT ( 'NONE',  ( 20.95312500061451999, -4.541064518000417216, -2.621784821875001281 ) ) ;
#48699 = CARTESIAN_POINT ( 'NONE',  ( 9.628125000614517148, -4.541064518000419881, 2.621784821874995952 ) ) ;
#48700 = CARTESIAN_POINT ( 'NONE',  ( 24.64687500061451431, 4.119189519843966529, -2.378215178124998275 ) ) ;
#48701 = CARTESIAN_POINT ( 'NONE',  ( 7.396875000614519635, -3.027376345333614438, 5.243569643749998122 ) ) ;
#48702 = CARTESIAN_POINT ( 'NONE',  ( 24.41250000000000142, 2.886751345948129099, -4.999999999999998224 ) ) ;
#48703 = CARTESIAN_POINT ( 'NONE',  ( 19.87500000122903288, -5.773502691896255534, -1.060575238724906372E-15 ) ) ;
#48704 = CARTESIAN_POINT ( 'NONE',  ( 27.06562500061451004, 3.027376345333611329, 5.243569643749999010 ) ) ;
#48705 = CARTESIAN_POINT ( 'NONE',  ( 3.242103837493086330E-14, 11.00000000122903288, 26.00000000000000711 ) ) ;
#48706 = CARTESIAN_POINT ( 'NONE',  ( 9.384375000614518569, 6.421520780324663323E-16, -5.243569643749999010 ) ) ;
#48707 = CARTESIAN_POINT ( 'NONE',  ( 15.27187500061451786, 3.027376345333613106, -5.243569643749998122 ) ) ;
#48708 = CARTESIAN_POINT ( 'NONE',  ( 24.94687500061451502, -3.027376345333614438, 5.243569643749998122 ) ) ;
#48709 = LINE ( 'NONE', #3279, #31223 ) ;
#48710 = EDGE_CURVE ( 'NONE', #2558, #49922, #3779, .T. ) ;
#48711 = CARTESIAN_POINT ( 'NONE',  ( 12.52500000000000213, -4.330127018922194537, 2.499999999999995559 ) ) ;
#48712 = CARTESIAN_POINT ( 'NONE',  ( 17.67187500061451644, 3.027376345333611329, 5.243569643749999010 ) ) ;
#48713 = CARTESIAN_POINT ( 'NONE',  ( 10.24687500061451750, -3.027376345333610441, -5.243569643749999898 ) ) ;
#48714 = CARTESIAN_POINT ( 'NONE',  ( 3.756430356250000102, 13.09062499938548463, 30.00000000000000000 ) ) ;
#48715 = CARTESIAN_POINT ( 'NONE',  ( 23.62500000000000000, 4.330127018922191873, 2.499999999999999556 ) ) ;
#48716 = CARTESIAN_POINT ( 'NONE',  ( 2.000000000000000444, 14.82500000000000107, 26.53589838486224650 ) ) ;
#48717 = CARTESIAN_POINT ( 'NONE',  ( -2.000000000000000000, 9.687500001229034652, -33.46410161513775705 ) ) ;
#48718 = CARTESIAN_POINT ( 'NONE',  ( 24.34687500061451715, 5.492252693125287522, 3.363034840372157021E-16 ) ) ;
#48719 = CARTESIAN_POINT ( 'NONE',  ( 11.84062500061451750, -3.027376345333614438, 5.243569643749998122 ) ) ;
#48720 = CARTESIAN_POINT ( 'NONE',  ( 29.25937500061451502, 4.541064518000418104, -2.621784821874998173 ) ) ;
#48721 = CARTESIAN_POINT ( 'NONE',  ( -5.810221930991193690E-16, 10.10000000122903430, -34.00000000000000000 ) ) ;
#48722 = CARTESIAN_POINT ( 'NONE',  ( 11.25000000000000000, -4.330127018922190985, -2.500000000000001332 ) ) ;
#48723 = CARTESIAN_POINT ( 'NONE',  ( -1.999999999999997113, 18.83750000122903501, 33.46410161513775705 ) ) ;
#48724 = CARTESIAN_POINT ( 'NONE',  ( 10.95000000122903394, -2.886751345948125991, -5.000000000000000000 ) ) ;
#48725 = CARTESIAN_POINT ( 'NONE',  ( 22.92187500061451644, 3.027376345333613106, -5.243569643749998122 ) ) ;
#48726 = CARTESIAN_POINT ( 'NONE',  ( 17.07187500061451502, 3.027376345333613106, -5.243569643749998122 ) ) ;
#48727 = DIRECTION ( 'NONE',  ( 0.000000000000000000, 0.000000000000000000, 1.000000000000000000 ) ) ;
#48728 = ORIENTED_EDGE ( 'NONE', *, *, #57133, .T. ) ;
#48729 = CARTESIAN_POINT ( 'NONE',  ( 16.79062500061451857, -3.027376345333614438, 5.243569643749998122 ) ) ;
#48730 = CARTESIAN_POINT ( 'NONE',  ( 28.46250000122903145, -4.330127018922190985, -2.500000000000001332 ) ) ;
#48731 = CARTESIAN_POINT ( 'NONE',  ( 17.78437500061451715, -4.541064518000419881, 2.621784821874995952 ) ) ;
#48732 = CARTESIAN_POINT ( 'NONE',  ( 29.37187500061451928, 3.027376345333611329, 5.243569643749999010 ) ) ;
#48733 = CARTESIAN_POINT ( 'NONE',  ( 4.940625000614515372, 6.054752690667223547, 3.707466751127219781E-16 ) ) ;
#48734 = CARTESIAN_POINT ( 'NONE',  ( 18.44062500061451715, 6.054752690667223547, 3.707466751127219781E-16 ) ) ;
#48735 = CARTESIAN_POINT ( 'NONE',  ( 28.77187500061451431, 3.027376345333613106, -5.243569643749998122 ) ) ;
#48736 = CARTESIAN_POINT ( 'NONE',  ( 2.121784821874999061, 13.80312500061451786, 26.32496088578401583 ) ) ;
#48737 = CARTESIAN_POINT ( 'NONE',  ( 17.58750000122903145, -4.330127018922194537, 2.499999999999995559 ) ) ;
#48738 = CARTESIAN_POINT ( 'NONE',  ( 9.759375000614516793, -4.119189519843965641, -2.378215178125001383 ) ) ;
#48739 = CARTESIAN_POINT ( 'NONE',  ( 8.015625000614516438, 3.027376345333612662, -5.243569643749998122 ) ) ;
#48740 = CARTESIAN_POINT ( 'NONE',  ( 26.76562500061451644, -6.054752690667223547, -1.112240025338166033E-15 ) ) ;
#48741 = CARTESIAN_POINT ( 'NONE',  ( -1.389182545231912203, 9.676047173952133207, 26.18324276292616304 ) ) ;
#48742 = CARTESIAN_POINT ( 'NONE',  ( 23.55937500061451573, 0.000000000000000000, 5.243569643749999010 ) ) ;
#48743 = CARTESIAN_POINT ( 'NONE',  ( 11.46562500061451573, -6.054752690667223547, -1.112240025338166033E-15 ) ) ;
#48744 = CARTESIAN_POINT ( 'NONE',  ( 22.35000000122903074, 5.773502691896255534, 3.535250795749688894E-16 ) ) ;
#48745 = CARTESIAN_POINT ( 'NONE',  ( 23.20312500061451644, -4.541064518000417216, -2.621784821875001281 ) ) ;
#48746 = CARTESIAN_POINT ( 'NONE',  ( 16.62187500061451573, 3.027376345333613106, -5.243569643749998122 ) ) ;
#48747 = CARTESIAN_POINT ( 'NONE',  ( 12.14062500061451821, 6.054752690667223547, 3.707466751127219781E-16 ) ) ;
#48748 = CARTESIAN_POINT ( 'NONE',  ( -4.243569643749999898, 14.45937500061451964, 30.00000000000000000 ) ) ;
#48749 = CARTESIAN_POINT ( 'NONE',  ( 19.41562500061451146, 3.027376345333611329, 5.243569643749999010 ) ) ;
#48750 = CARTESIAN_POINT ( 'NONE',  ( 29.72812500061451502, 4.541064518000418104, 2.621784821874999949 ) ) ;
#48751 = ORIENTED_EDGE ( 'NONE', *, *, #66440, .F. ) ;
#48752 = ORIENTED_EDGE ( 'NONE', *, *, #66261, .F. ) ;
#48753 = CARTESIAN_POINT ( 'NONE',  ( 23.40000000000000213, -4.330127018922190985, -2.500000000000001332 ) ) ;
#48754 = CARTESIAN_POINT ( 'NONE',  ( -2.121784821874996840, 19.03437500061451715, -26.32496088578401583 ) ) ;
#48755 = CARTESIAN_POINT ( 'NONE',  ( -6.275039685470489619E-15, 17.97500000122903074, 33.99999999999999289 ) ) ;
#48756 = CARTESIAN_POINT ( 'NONE',  ( 26.20312500061451644, 0.000000000000000000, 5.243569643749999010 ) ) ;
#48757 = CARTESIAN_POINT ( 'NONE',  ( 4.903125000614516615, 4.541064518000418104, -2.621784821874998173 ) ) ;
#48758 = CARTESIAN_POINT ( 'NONE',  ( 18.78750000122903430, 4.330127018922191873, 2.499999999999999556 ) ) ;
#48759 = CARTESIAN_POINT ( 'NONE',  ( 24.17812500061451786, 6.421520780324663323E-16, -5.243569643749999010 ) ) ;
#48760 = CARTESIAN_POINT ( 'NONE',  ( 24.03750000000000142, 5.773502691896255534, 3.535250795749688894E-16 ) ) ;
#48761 = EDGE_CURVE ( 'NONE', #54869, #54799, #20768, .T. ) ;
#48762 = CARTESIAN_POINT ( 'NONE',  ( 28.00312500061451715, 0.000000000000000000, 5.243569643749999010 ) ) ;
#48763 = CARTESIAN_POINT ( 'NONE',  ( 7.153125000614518392, 4.541064518000418104, -2.621784821874998173 ) ) ;
#48764 = EDGE_LOOP ( 'NONE', ( #27818, #10404, #34786, #46096 ) ) ;
#48765 = CARTESIAN_POINT ( 'NONE',  ( 23.24062500061451786, -3.027376345333610441, -5.243569643749999898 ) ) ;
#48766 = CARTESIAN_POINT ( 'NONE',  ( 5.278125000614516615, 6.421520780324663323E-16, -5.243569643749999010 ) ) ;
#48767 = CARTESIAN_POINT ( 'NONE',  ( 14.70937500061451786, -4.119189519843965641, -2.378215178125001383 ) ) ;
#48768 = CARTESIAN_POINT ( 'NONE',  ( 4.898587196589411843E-16, 20.00000000000000000, 33.99999999999999289 ) ) ;
#48769 = CARTESIAN_POINT ( 'NONE',  ( 3.999999999999999112, 13.13750000122903394, -30.00000000000000000 ) ) ;
#48770 = CARTESIAN_POINT ( 'NONE',  ( -3.999999999999999112, 10.55000000000000249, -30.00000000000000000 ) ) ;
#48771 = CARTESIAN_POINT ( 'NONE',  ( 9.712500000000002132, 2.886751345948126879, 4.999999999999999112 ) ) ;
#48772 = CARTESIAN_POINT ( 'NONE',  ( 11.25937500061451679, 4.541064518000418104, -2.621784821874998173 ) ) ;
#48773 = CARTESIAN_POINT ( 'NONE',  ( 5.662500001229035185, 4.330127018922192761, -2.499999999999997780 ) ) ;
#48774 = CARTESIAN_POINT ( 'NONE',  ( 14.33437500061451786, 6.421520780324663323E-16, -5.243569643749999010 ) ) ;
#48775 = CARTESIAN_POINT ( 'NONE',  ( 15.11249999999999893, 2.886751345948126879, 4.999999999999999112 ) ) ;
#48776 = CARTESIAN_POINT ( 'NONE',  ( 7.171875000614517326, 3.027376345333613106, -5.243569643749998122 ) ) ;
#48777 = CARTESIAN_POINT ( 'NONE',  ( 4.000000000000000000, 18.38750000000000284, 32.30940107675849760 ) ) ;
#48778 = FACE_OUTER_BOUND ( 'NONE', #66920, .T. ) ;
#48779 = CARTESIAN_POINT ( 'NONE',  ( 11.78437500061451892, 4.541064518000418104, 2.621784821874999949 ) ) ;
#48780 = CARTESIAN_POINT ( 'NONE',  ( 3.692551571010786127, 3.371233518040734012, 4.016210762354105235 ) ) ;
#48781 = CARTESIAN_POINT ( 'NONE',  ( 21.36562500061451431, -6.054752690667223547, -1.112240025338166033E-15 ) ) ;
#48782 = CARTESIAN_POINT ( 'NONE',  ( 9.001249775931846008E-16, 10.07187500061451857, 34.90005215228797653 ) ) ;
#48783 = CARTESIAN_POINT ( 'NONE',  ( 2.121784821874999061, 19.65312500061459389, 26.32496088578401583 ) ) ;
#48784 = CARTESIAN_POINT ( 'NONE',  ( 24.90937500061451715, 0.000000000000000000, 5.243569643749999010 ) ) ;
#48785 = CARTESIAN_POINT ( 'NONE',  ( 4.352316639481299987, 2.462457182806187639, 4.352316639481299987 ) ) ;
#48786 = CARTESIAN_POINT ( 'NONE',  ( 5.090625000614516615, -3.027376345333614438, 5.243569643749998122 ) ) ;
#48787 = CARTESIAN_POINT ( 'NONE',  ( 22.13437500061451502, -2.746126346562646425, 4.756430356249996549 ) ) ;
#48788 = CARTESIAN_POINT ( 'NONE',  ( 14.78437500061451715, 6.421520780324663323E-16, -5.243569643749999010 ) ) ;
#48789 = CARTESIAN_POINT ( 'NONE',  ( 29.88749999999999929, 5.773502691896255534, 3.535250795749688894E-16 ) ) ;
#48790 = CARTESIAN_POINT ( 'NONE',  ( 27.71250000122903145, 4.330127018922192761, -2.499999999999997780 ) ) ;
#48791 = CARTESIAN_POINT ( 'NONE',  ( 5.259375000614518569, -4.541064518000417216, -2.621784821875001281 ) ) ;
#48792 = CARTESIAN_POINT ( 'NONE',  ( 16.62187500061451573, 3.027376345333613106, -5.243569643749998122 ) ) ;
#48793 = CARTESIAN_POINT ( 'NONE',  ( 24.26249999999999929, -5.773502691896255534, -1.060575238724906372E-15 ) ) ;
#48794 = EDGE_CURVE ( 'NONE', #54869, #61146, #71372, .T. ) ;
#48795 = CARTESIAN_POINT ( 'NONE',  ( 4.125000001229034652, -5.773502691896255534, -1.060575238724906372E-15 ) ) ;
#48796 = CARTESIAN_POINT ( 'NONE',  ( 26.40937500061451715, -4.541064518000417216, -2.621784821875001281 ) ) ;
#48797 = CARTESIAN_POINT ( 'NONE',  ( -3.756430356250000102, 12.97812499938548214, 30.00000000000000000 ) ) ;
#48798 = CARTESIAN_POINT ( 'NONE',  ( 29.58749999999999858, -2.886751345948129988, 4.999999999999997335 ) ) ;
#48799 = CARTESIAN_POINT ( 'NONE',  ( 8.587500000000002132, -2.886751345948125991, -5.000000000000000000 ) ) ;
#48800 = CARTESIAN_POINT ( 'NONE',  ( 9.984375000614516438, -2.746126346562646425, 4.756430356249996549 ) ) ;
#48801 = CARTESIAN_POINT ( 'NONE',  ( 18.77812500061451573, 6.421520780324663323E-16, -5.243569643749999010 ) ) ;
#48802 = CARTESIAN_POINT ( 'NONE',  ( 10.95000000000000107, 4.330127018922192761, -2.499999999999997780 ) ) ;
#48803 = CARTESIAN_POINT ( 'NONE',  ( 5.278125000614516615, 6.421520780324663323E-16, -5.243569643749999010 ) ) ;
#48804 = CARTESIAN_POINT ( 'NONE',  ( 18.71249999999999858, 2.886751345948126879, 4.999999999999999112 ) ) ;
#48805 = CARTESIAN_POINT ( 'NONE',  ( 17.57812500061451644, 4.541064518000418104, 2.621784821874999949 ) ) ;
#48806 = CARTESIAN_POINT ( 'NONE',  ( -5.810221930991193690E-16, 18.65000000122903501, 26.00000000000000355 ) ) ;
#48807 = CARTESIAN_POINT ( 'NONE',  ( 22.35000000122903074, 5.773502691896255534, 3.535250795749688894E-16 ) ) ;
#48808 = CARTESIAN_POINT ( 'NONE',  ( -1.878215178125001827, 20.14062499938548356, 33.25316411605952283 ) ) ;
#48809 = CARTESIAN_POINT ( 'NONE',  ( 29.33437500061451431, 4.541064518000418104, 2.621784821874999949 ) ) ;
#48810 = ORIENTED_EDGE ( 'NONE', *, *, #59386, .T. ) ;
#48811 = CARTESIAN_POINT ( 'NONE',  ( 18.55312500061451431, 0.000000000000000000, 5.243569643749999010 ) ) ;
#48812 = CARTESIAN_POINT ( 'NONE',  ( 24.59062500061451573, -3.027376345333610441, -5.243569643749999898 ) ) ;
#48813 = CARTESIAN_POINT ( 'NONE',  ( 24.57187500061451502, -6.054752690667223547, -1.112240025338166033E-15 ) ) ;
#48814 = CARTESIAN_POINT ( 'NONE',  ( 8.925000000000002487, -4.330127018922194537, 2.499999999999995559 ) ) ;
#48815 = CARTESIAN_POINT ( 'NONE',  ( 11.27812500061451573, 4.541064518000418104, 2.621784821874999949 ) ) ;
#48816 = CARTESIAN_POINT ( 'NONE',  ( 26.91562500061451146, 3.027376345333613106, -5.243569643749998122 ) ) ;
#48817 = CARTESIAN_POINT ( 'NONE',  ( 16.58437500061451786, 6.421520780324663323E-16, -5.243569643749999010 ) ) ;
#48818 = CARTESIAN_POINT ( 'NONE',  ( 10.11562500061451608, -6.054752690667223547, -1.112240025338166033E-15 ) ) ;
#48819 = CARTESIAN_POINT ( 'NONE',  ( 34.99999999999999289, -6.363961030678871644, 6.363961030678982667 ) ) ;
#48820 = CARTESIAN_POINT ( 'NONE',  ( 4.243569643749999898, 19.54062500061451857, 32.45002607614398471 ) ) ;
#48821 = CARTESIAN_POINT ( 'NONE',  ( 22.83750000122903501, 4.330127018922191873, 2.499999999999999556 ) ) ;
#48822 = CARTESIAN_POINT ( 'NONE',  ( 16.80937500061451573, 0.000000000000000000, 4.756430356249998326 ) ) ;
#48823 = CARTESIAN_POINT ( 'NONE',  ( 14.57812500061451644, -4.541064518000419881, 2.621784821874995952 ) ) ;
#48824 = CARTESIAN_POINT ( 'NONE',  ( 7.584375000614516082, 6.421520780324663323E-16, -5.243569643749999010 ) ) ;
#48825 = CARTESIAN_POINT ( 'NONE',  ( 6.121875000614517504, -6.054752690667223547, -1.112240025338166033E-15 ) ) ;
#48826 =( BOUNDED_CURVE ( )  B_SPLINE_CURVE ( 2, ( #51097, #67376, #44111, #16739, #61808, #17101, #49650 ),
 .UNSPECIFIED., .F., .F. ) 
 B_SPLINE_CURVE_WITH_KNOTS ( ( 3, 2, 2, 3 ),
 ( 0.4400000000000000022, 0.4433333333333333570, 0.4466666666666666563, 0.4500000000000000111 ),
 .UNSPECIFIED. ) 
 CURVE ( )  GEOMETRIC_REPRESENTATION_ITEM ( )  RATIONAL_B_SPLINE_CURVE ( ( 1.000000000000000000, 0.8660254037844387076, 1.000000000000000000, 0.8660254037844387076, 1.000000000000000000, 0.8660254037844387076, 1.000000000000000000 ) ) 
 REPRESENTATION_ITEM ( '' )  );
#48827 = ORIENTED_EDGE ( 'NONE', *, *, #25975, .T. ) ;
#48828 = CARTESIAN_POINT ( 'NONE',  ( 1.999999999999998668, 13.55000000000000071, 26.53589838486224650 ) ) ;
#48829 = CARTESIAN_POINT ( 'NONE',  ( 21.85312500061451502, -4.541064518000417216, -2.621784821875001281 ) ) ;
#48830 = CARTESIAN_POINT ( 'NONE',  ( 15.87187500061451573, 3.027376345333611329, 5.243569643749999010 ) ) ;
#48831 = CARTESIAN_POINT ( 'NONE',  ( 20.27812500061451573, 4.541064518000418104, 2.621784821874999949 ) ) ;
#48832 = CARTESIAN_POINT ( 'NONE',  ( 4.000000000000000000, 12.98749999999999893, 32.30940107675849049 ) ) ;
#48833 = CARTESIAN_POINT ( 'NONE',  ( 26.16562500061451502, 3.027376345333611329, 5.243569643749999010 ) ) ;
#48834 = CARTESIAN_POINT ( 'NONE',  ( 7.875000001229034652, 2.886751345948129099, -4.999999999999998224 ) ) ;
#48835 = ORIENTED_EDGE ( 'NONE', *, *, #67839, .T. ) ;
#48836 = FACE_OUTER_BOUND ( 'NONE', #63672, .T. ) ;
#48837 = CARTESIAN_POINT ( 'NONE',  ( 3.999999999999998668, 17.56250000000000000, -32.30940107675850470 ) ) ;
#48838 = CARTESIAN_POINT ( 'NONE',  ( 24.15000000122903145, 5.773502691896255534, 3.535250795749688894E-16 ) ) ;
#48839 = CARTESIAN_POINT ( 'NONE',  ( -3.756430356250000102, 15.22812499938548392, 30.00000000000000000 ) ) ;
#48840 = CARTESIAN_POINT ( 'NONE',  ( 7.059375000614518392, -4.541064518000417216, -2.621784821875001281 ) ) ;
#48841 = CARTESIAN_POINT ( 'NONE',  ( 0.000000000000000000, 20.00000000000000000, -30.00000000000000000 ) ) ;
#48842 = CARTESIAN_POINT ( 'NONE',  ( 12.70312500061451821, 0.000000000000000000, 5.243569643749999010 ) ) ;
#48843 = EDGE_CURVE ( 'NONE', #64135, #56329, #21283, .T. ) ;
#48844 = CARTESIAN_POINT ( 'NONE',  ( 7.621875000614519280, 3.027376345333613106, -5.243569643749998122 ) ) ;
#48845 = CARTESIAN_POINT ( 'NONE',  ( 26.66250000122903430, -4.330127018922190985, -2.500000000000001332 ) ) ;
#48846 = CARTESIAN_POINT ( 'NONE',  ( 16.65937500061452070, 4.541064518000418104, -2.621784821874998173 ) ) ;
#48847 = CARTESIAN_POINT ( 'NONE',  ( 4.959375000614516971, 4.541064518000418104, -2.621784821874998173 ) ) ;
#48848 = CARTESIAN_POINT ( 'NONE',  ( 29.73750000000000071, -2.886751345948125991, -5.000000000000000000 ) ) ;
#48849 = CARTESIAN_POINT ( 'NONE',  ( 5.615625000614517859, -6.054752690667223547, -1.112240025338166033E-15 ) ) ;
#48850 = CARTESIAN_POINT ( 'NONE',  ( 15.85312500061451857, 0.000000000000000000, 5.243569643749999010 ) ) ;
#48851 = EDGE_CURVE ( 'NONE', #9450, #63279, #23214, .T. ) ;
#48852 = VERTEX_POINT ( 'NONE', #31106 ) ;
#48853 = CARTESIAN_POINT ( 'NONE',  ( 11.57812500061451644, 6.421520780324663323E-16, -5.243569643749999010 ) ) ;
#48854 = CARTESIAN_POINT ( 'NONE',  ( 5.700000001229033941, 5.773502691896255534, 3.535250795749688894E-16 ) ) ;
#48855 = CARTESIAN_POINT ( 'NONE',  ( 7.753125000614518036, 0.000000000000000000, 5.243569643749999010 ) ) ;
#48856 = CARTESIAN_POINT ( 'NONE',  ( 21.72187500061451715, 2.746126346562643317, 4.756430356249998326 ) ) ;
#48857 = CARTESIAN_POINT ( 'NONE',  ( 7.875000000000000000, 4.330127018922191873, 2.499999999999999556 ) ) ;
#48858 = CARTESIAN_POINT ( 'NONE',  ( 3.075000001229035718, 2.886751345948126879, 4.999999999999999112 ) ) ;
#48859 = CARTESIAN_POINT ( 'NONE',  ( 17.39999999999999858, 0.000000000000000000, 4.999999999999998224 ) ) ;
#48860 = CARTESIAN_POINT ( 'NONE',  ( 17.44687500061451857, -3.027376345333610441, -5.243569643749999898 ) ) ;
#48861 = CARTESIAN_POINT ( 'NONE',  ( 13.01250000122903394, 0.000000000000000000, 4.999999999999998224 ) ) ;
#48862 = CARTESIAN_POINT ( 'NONE',  ( 23.06250000000000355, 2.886751345948129099, -4.999999999999998224 ) ) ;
#48863 = CARTESIAN_POINT ( 'NONE',  ( -4.243569643749999898, 17.55312500061451786, -30.00000000000000000 ) ) ;
#48864 = CARTESIAN_POINT ( 'NONE',  ( 11.96250000122903501, 4.330127018922192761, -2.499999999999997780 ) ) ;
#48865 = CARTESIAN_POINT ( 'NONE',  ( -2.672702088255949472E-15, 13.45624999877096784, 26.00000000000000000 ) ) ;
#48866 = DIRECTION ( 'NONE',  ( -1.000000000000000000, -0.000000000000000000, -0.000000000000000000 ) ) ;
#48867 = CARTESIAN_POINT ( 'NONE',  ( 29.16562500061451502, 3.027376345333613106, -5.243569643749998122 ) ) ;
#48868 = DIRECTION ( 'NONE',  ( 0.000000000000000000, 0.000000000000000000, 1.000000000000000000 ) ) ;
#48869 = CARTESIAN_POINT ( 'NONE',  ( 19.59375000122902932, 5.773502691896255534, 3.535250795749688401E-16 ) ) ;
#48870 = CARTESIAN_POINT ( 'NONE',  ( 15.08437500061451786, -4.541064518000419881, 2.621784821874995952 ) ) ;
#48871 =( BOUNDED_CURVE ( )  B_SPLINE_CURVE ( 2, ( #35043, #57570, #18399, #40966, #63482, #12869, #35401 ),
 .UNSPECIFIED., .F., .F. ) 
 B_SPLINE_CURVE_WITH_KNOTS ( ( 3, 2, 2, 3 ),
 ( 0.07499999999999996947, 0.07777777777777775126, 0.08055555555555551916, 0.08333333333333328707 ),
 .UNSPECIFIED. ) 
 CURVE ( )  GEOMETRIC_REPRESENTATION_ITEM ( )  RATIONAL_B_SPLINE_CURVE ( ( 1.000000000000001332, 0.8660254037844373753, 1.000000000000000000, 0.8660254037844387076, 1.000000000000000000, 0.8660254037844407060, 0.9999999999999980016 ) ) 
 REPRESENTATION_ITEM ( '' )  );
#48872 = CARTESIAN_POINT ( 'NONE',  ( 28.35000000000000142, -4.330127018922190985, -2.500000000000001332 ) ) ;
#48873 = CARTESIAN_POINT ( 'NONE',  ( 12.17812500061451608, 4.541064518000418104, 2.621784821874999949 ) ) ;
#48874 = CARTESIAN_POINT ( 'NONE',  ( 29.22187500061451360, 4.119189519843966529, 2.378215178124999607 ) ) ;
#48875 = CARTESIAN_POINT ( 'NONE',  ( 20.37187500061451573, 3.027376345333611329, 5.243569643749999010 ) ) ;
#48876 = CARTESIAN_POINT ( 'NONE',  ( 12.42187500061451466, 5.824947211148865298E-16, -4.756430356249998326 ) ) ;
#48877 = CARTESIAN_POINT ( 'NONE',  ( 8.128125000614515372, 4.541064518000418104, 2.621784821874999949 ) ) ;
#48878 = CARTESIAN_POINT ( 'NONE',  ( 13.65937500061451715, 0.000000000000000000, 5.243569643749999010 ) ) ;
#48879 = ORIENTED_EDGE ( 'NONE', *, *, #51676, .F. ) ;
#48880 = CARTESIAN_POINT ( 'NONE',  ( 23.89687500061451786, 6.054752690667223547, 3.707466751127219781E-16 ) ) ;
#48881 = CARTESIAN_POINT ( 'NONE',  ( 27.70312500061451289, -4.541064518000417216, -2.621784821875001281 ) ) ;
#48882 = DIRECTION ( 'NONE',  ( 0.000000000000000000, 0.000000000000000000, 1.000000000000000000 ) ) ;
#48883 = CARTESIAN_POINT ( 'NONE',  ( 7.087499999999999467, -2.886751345948129988, 4.999999999999997335 ) ) ;
#48884 = CARTESIAN_POINT ( 'NONE',  ( 17.85000000122903430, 5.773502691896255534, 3.535250795749688894E-16 ) ) ;
#48885 = CARTESIAN_POINT ( 'NONE',  ( 27.22500000122903785, 2.886751345948162850, -4.999999999999940492 ) ) ;
#48886 = CARTESIAN_POINT ( 'NONE',  ( 9.084375000614516082, -2.746126346562646425, 4.756430356249996549 ) ) ;
#48887 = ORIENTED_EDGE ( 'NONE', *, *, #60961, .T. ) ;
#48888 = CARTESIAN_POINT ( 'NONE',  ( 15.67500000000000071, -4.330127018922194537, 2.499999999999995559 ) ) ;
#48889 = CARTESIAN_POINT ( 'NONE',  ( 18.00000000000000355, -4.330127018922190985, -2.500000000000001332 ) ) ;
#48890 = CARTESIAN_POINT ( 'NONE',  ( 11.65312500061451573, 4.541064518000418104, -2.621784821874998173 ) ) ;
#48891 = VERTEX_POINT ( 'NONE', #53646 ) ;
#48892 = CARTESIAN_POINT ( 'NONE',  ( -1.071796769724491005, 10.90759618943233455, -34.00000000000000000 ) ) ;
#48893 = CARTESIAN_POINT ( 'NONE',  ( 4.243569643749999898, 17.38437500061451502, -30.00000000000000000 ) ) ;
#48894 = CARTESIAN_POINT ( 'NONE',  ( 3.065625000614517592, 3.027376345333613106, -5.243569643749998122 ) ) ;
#48895 = CARTESIAN_POINT ( 'NONE',  ( 10.20000000000000107, 0.000000000000000000, 4.999999999999998224 ) ) ;
#48896 = CARTESIAN_POINT ( 'NONE',  ( 10.05000000000000071, 4.330127018922192761, -2.499999999999997780 ) ) ;
#48897 = CARTESIAN_POINT ( 'NONE',  ( 3.128911089188104011, 3.899989153312591661, 3.342749051770597557 ) ) ;
#48898 = VECTOR ( 'NONE', #16861, 1000.000000000000000 ) ;
#48899 = ORIENTED_EDGE ( 'NONE', *, *, #40501, .T. ) ;
#48900 = CARTESIAN_POINT ( 'NONE',  ( 4.243569643749999010, 12.41562500061451857, 27.54997392385601174 ) ) ;
#48901 = CARTESIAN_POINT ( 'NONE',  ( 25.86562500061451431, -6.054752690667223547, -1.112240025338166033E-15 ) ) ;
#48902 = CARTESIAN_POINT ( 'NONE',  ( 3.756430356250000546, 19.42812499938548143, 27.83122392262697886 ) ) ;
#48903 = CARTESIAN_POINT ( 'NONE',  ( 21.87187500061451573, -6.054752690667223547, -1.112240025338166033E-15 ) ) ;
#48904 = CARTESIAN_POINT ( 'NONE',  ( 19.60312500061451502, -4.541064518000417216, -2.621784821875001281 ) ) ;
#48905 = CARTESIAN_POINT ( 'NONE',  ( -4.243569643749999898, 13.46562500061459744, -32.45002607614398471 ) ) ;
#48906 = CARTESIAN_POINT ( 'NONE',  ( 22.98750000122903003, -4.330127018922194537, 2.499999999999995559 ) ) ;
#48907 = CLOSED_SHELL ( 'NONE', ( #37347, #37175, #55855, #9012, #29568, #40485, #43137, #42580, #19024, #30040, #10333, #4102, #48031, #26087, #56863, #64386, #69287, #69757, #11148, #35563, #12542, #21291, #24565, #55678, #67441, #17317, #62389, #17706, #27243, #60747, #53579, #52407, #11636, #20661, #61932, #9517, #55412, #21155, #62663, #24600, #64171, #34272, #32148, #30551, #7221, #41033, #43795, #9054 ) ) ;
#48908 = CARTESIAN_POINT ( 'NONE',  ( 3.478125000614517237, 6.421520780324663323E-16, -5.243569643749999010 ) ) ;
#48909 = CARTESIAN_POINT ( 'NONE',  ( 26.52187500061451431, 2.746126346562645981, -4.756430356249997438 ) ) ;
#48910 = CARTESIAN_POINT ( 'NONE',  ( 21.74062500061451431, -3.027376345333614438, 5.243569643749998122 ) ) ;
#48911 = DIRECTION ( 'NONE',  ( -1.000000000000000000, -0.000000000000000000, -0.000000000000000000 ) ) ;
#48912 = CARTESIAN_POINT ( 'NONE',  ( 1.878215178125000495, 16.31562499938548427, 26.74683588394047007 ) ) ;
#48913 = CARTESIAN_POINT ( 'NONE',  ( 14.37187500061451928, 3.027376345333613106, -5.243569643749998122 ) ) ;
#48914 = CARTESIAN_POINT ( 'NONE',  ( 15.04687500061451644, -3.027376345333614438, 5.243569643749998122 ) ) ;
#48915 = CARTESIAN_POINT ( 'NONE',  ( 24.42187500061451999, 3.027376345333611329, 5.243569643749999010 ) ) ;
#48916 = CARTESIAN_POINT ( 'NONE',  ( -4.243569643749998122, 14.49687500061451750, 32.45002607614398471 ) ) ;
#48917 = CARTESIAN_POINT ( 'NONE',  ( 5.353125000614515905, 4.541064518000418104, -2.621784821874998173 ) ) ;
#48918 = CARTESIAN_POINT ( 'NONE',  ( 16.46250000122903501, 4.330127018922192761, -2.499999999999997780 ) ) ;
#48919 = VECTOR ( 'NONE', #7078, 1000.000000000000000 ) ;
#48920 = EDGE_CURVE ( 'NONE', #15201, #40801, #38321, .T. ) ;
#48921 = CARTESIAN_POINT ( 'NONE',  ( 29.01562500061451644, -6.054752690667223547, -1.112240025338166033E-15 ) ) ;
#48922 = DIRECTION ( 'NONE',  ( 1.000000000000000000, 0.000000000000000000, 0.000000000000000000 ) ) ;
#48923 = CARTESIAN_POINT ( 'NONE',  ( 4.000000000000000000, 19.73749999999999716, 32.30940107675849049 ) ) ;
#48924 = CARTESIAN_POINT ( 'NONE',  ( 7.696875000614516793, 6.054752690667223547, 3.707466751127219781E-16 ) ) ;
#48925 = DIRECTION ( 'NONE',  ( 1.000000000000000000, 0.000000000000000000, 0.000000000000000000 ) ) ;
#48926 = CARTESIAN_POINT ( 'NONE',  ( 14.10000000122903252, -2.886751345948125991, -5.000000000000000000 ) ) ;
#48927 = CIRCLE ( 'NONE', #33566, 4.000000000000000000 ) ;
#48928 = CARTESIAN_POINT ( 'NONE',  ( 9.675000001229035362, 2.886751345948129099, -4.999999999999998224 ) ) ;
#48929 = CARTESIAN_POINT ( 'NONE',  ( 6.140625000614516438, -3.027376345333610441, -5.243569643749999898 ) ) ;
#48930 = CARTESIAN_POINT ( 'NONE',  ( -1.999999999999999112, 16.64374999877096784, 26.53589838486224650 ) ) ;
#48931 = CARTESIAN_POINT ( 'NONE',  ( 18.61875000122903145, 2.886751345948129099, -4.999999999999998224 ) ) ;
#48932 = CARTESIAN_POINT ( 'NONE',  ( 14.67187500061451821, -6.054752690667223547, -1.112240025338166033E-15 ) ) ;
#48933 = DIRECTION ( 'NONE',  ( -0.000000000000000000, -1.000000000000000000, -0.000000000000000000 ) ) ;
#48934 = EDGE_LOOP ( 'NONE', ( #63, #6453, #21983, #22715 ) ) ;
#48935 = CARTESIAN_POINT ( 'NONE',  ( 21.66562500061451502, 3.027376345333611329, 5.243569643749999010 ) ) ;
#48936 = CARTESIAN_POINT ( 'NONE',  ( 6.815625000614517148, 3.027376345333611329, 5.243569643749999010 ) ) ;
#48937 = CARTESIAN_POINT ( 'NONE',  ( 25.09687500061451715, -3.027376345333610441, -5.243569643749999898 ) ) ;
#48938 = CARTESIAN_POINT ( 'NONE',  ( 6.853125000614516793, 0.000000000000000000, 5.243569643749999010 ) ) ;
#48939 = CARTESIAN_POINT ( 'NONE',  ( 6.525000001229035007, 2.886751345948129099, -4.999999999999997335 ) ) ;
#48940 = CARTESIAN_POINT ( 'NONE',  ( 8.625000001229034652, -5.773502691896255534, -1.060575238724906372E-15 ) ) ;
#48941 = CARTESIAN_POINT ( 'NONE',  ( 23.24062500061451786, -3.027376345333610441, -5.243569643749999898 ) ) ;
#48942 = EDGE_CURVE ( 'NONE', #55986, #38622, #4148, .T. ) ;
#48943 = CARTESIAN_POINT ( 'NONE',  ( 2.121784821874999061, 11.55312500061451786, -33.67503911421598417 ) ) ;
#48944 = CARTESIAN_POINT ( 'NONE',  ( 10.61250000122903536, 4.330127018922192761, -2.499999999999997780 ) ) ;
#48945 = CARTESIAN_POINT ( 'NONE',  ( 18.77812500061451573, 6.421520780324663323E-16, -5.243569643749999010 ) ) ;
#48946 = CARTESIAN_POINT ( 'NONE',  ( 15.74062500061451608, 6.054752690667223547, 3.707466751127219781E-16 ) ) ;
#48947 = CARTESIAN_POINT ( 'NONE',  ( 28.13437500061451502, -4.119189519843968306, 2.378215178124996054 ) ) ;
#48948 = CARTESIAN_POINT ( 'NONE',  ( 15.11249999999999893, 2.886751345948126879, 4.999999999999999112 ) ) ;
#48949 = CARTESIAN_POINT ( 'NONE',  ( 10.31250000122903288, 0.000000000000000000, 4.999999999999998224 ) ) ;
#48950 = CARTESIAN_POINT ( 'NONE',  ( 8.240625000614516082, -3.027376345333614438, 5.243569643749998122 ) ) ;
#48951 = CARTESIAN_POINT ( 'NONE',  ( 11.91562500061451857, -6.054752690667223547, -1.112240025338166033E-15 ) ) ;
#48952 = CARTESIAN_POINT ( 'NONE',  ( 22.12500000122903288, -5.773502691896255534, -1.060575238724906372E-15 ) ) ;
#48953 = AXIS2_PLACEMENT_3D ( 'NONE', #45053, #68312, #17672 ) ;
#48954 = CARTESIAN_POINT ( 'NONE',  ( 19.17187500061451999, -6.054752690667223547, -1.112240025338166033E-15 ) ) ;
#48955 = CARTESIAN_POINT ( 'NONE',  ( 5.137500001229033941, 6.123233995736764310E-16, -4.999999999999998224 ) ) ;
#48956 = AXIS2_PLACEMENT_3D ( 'NONE', #65877, #32627, #49262 ) ;
#48957 = CARTESIAN_POINT ( 'NONE',  ( 4.359375000614517326, -4.541064518000417216, -2.621784821875001281 ) ) ;
#48958 = CARTESIAN_POINT ( 'NONE',  ( 22.32187500061451502, -6.054752690667223547, -1.112240025338166033E-15 ) ) ;
#48959 = CARTESIAN_POINT ( 'NONE',  ( 10.65000000000000036, 0.000000000000000000, 4.999999999999998224 ) ) ;
#48960 = CARTESIAN_POINT ( 'NONE',  ( 18.14062500061451644, -3.027376345333614438, 5.243569643749998122 ) ) ;
#48961 = CARTESIAN_POINT ( 'NONE',  ( 25.05937500061451573, -4.541064518000417216, -2.621784821875001281 ) ) ;
#48962 = CARTESIAN_POINT ( 'NONE',  ( -1.878215178124999163, 20.55312499938548143, 26.74683588394047007 ) ) ;
#48963 = CARTESIAN_POINT ( 'NONE',  ( 5.810221930991193690E-16, 14.41249999999999787, 26.00000000000000000 ) ) ;
#48964 = CARTESIAN_POINT ( 'NONE',  ( 0.000000000000000000, 20.00000000000000000, -33.99999999999999289 ) ) ;
#48965 = CARTESIAN_POINT ( 'NONE',  ( 4.546875000614517326, 6.054752690667223547, 3.707466751127219781E-16 ) ) ;
#48966 = CARTESIAN_POINT ( 'NONE',  ( 14.87812500061451537, 4.541064518000418104, 2.621784821874999949 ) ) ;
#48967 = VECTOR ( 'NONE', #35318, 1000.000000000000000 ) ;
#48968 = CARTESIAN_POINT ( 'NONE',  ( 13.20937500061451786, 0.000000000000000000, 5.243569643749999010 ) ) ;
#48969 = VERTEX_POINT ( 'NONE', #46114 ) ;
#48970 = CARTESIAN_POINT ( 'NONE',  ( 22.38750000122903216, 4.330127018922191873, 2.499999999999999556 ) ) ;
#48971 = CARTESIAN_POINT ( 'NONE',  ( 26.20312500061451644, 0.000000000000000000, 5.243569643749999010 ) ) ;
#48972 = CARTESIAN_POINT ( 'NONE',  ( 1.071796769724476572, 12.93259618943233313, -25.99999999999999289 ) ) ;
#48973 = CARTESIAN_POINT ( 'NONE',  ( 30.00000000000000000, 0.000000000000000000, 4.999999999999998224 ) ) ;
#48974 = CARTESIAN_POINT ( 'NONE',  ( 13.95000000000000107, -4.330127018922190985, -2.500000000000001332 ) ) ;
#48975 = CARTESIAN_POINT ( 'NONE',  ( 25.35000000122903074, -2.886751345948125991, -5.000000000000000000 ) ) ;
#48976 = CARTESIAN_POINT ( 'NONE',  ( 18.89062500061451644, 6.054752690667223547, 3.707466751127219781E-16 ) ) ;
#48977 = ORIENTED_EDGE ( 'NONE', *, *, #32022, .T. ) ;
#48978 = CARTESIAN_POINT ( 'NONE',  ( 23.28750000000000142, -2.886751345948129988, 4.999999999999997335 ) ) ;
#48979 = CARTESIAN_POINT ( 'NONE',  ( 24.60937500061451644, -4.541064518000417216, -2.621784821875001281 ) ) ;
#48980 = ORIENTED_EDGE ( 'NONE', *, *, #531, .T. ) ;
#48981 = CARTESIAN_POINT ( 'NONE',  ( 19.04999999999999716, 4.330127018922192761, -2.499999999999997780 ) ) ;
#48982 = CARTESIAN_POINT ( 'NONE',  ( 10.90312500061451928, 0.000000000000000000, 5.243569643749999010 ) ) ;
#48983 = CARTESIAN_POINT ( 'NONE',  ( 3.815625000614518036, -6.054752690667223547, -1.112240025338166033E-15 ) ) ;
#48984 = CARTESIAN_POINT ( 'NONE',  ( 14.37187500061451573, 4.119189519843966529, 2.378215178124999607 ) ) ;
#48985 = CARTESIAN_POINT ( 'NONE',  ( 26.80312500061451431, -4.541064518000417216, -2.621784821875001281 ) ) ;
#48986 = CARTESIAN_POINT ( 'NONE',  ( 17.55000000000000071, -4.330127018922190985, -2.500000000000001332 ) ) ;
#48987 = CARTESIAN_POINT ( 'NONE',  ( 27.82499999999999929, -4.330127018922194537, 2.499999999999995559 ) ) ;
#48988 = CARTESIAN_POINT ( 'NONE',  ( 7.837499999999999467, 5.773502691896255534, 3.535250795749688401E-16 ) ) ;
#48989 = CARTESIAN_POINT ( 'NONE',  ( 7.209375000614519635, 4.541064518000418104, -2.621784821874998173 ) ) ;
#48990 = CARTESIAN_POINT ( 'NONE',  ( 17.18437500061451573, 4.541064518000418104, 2.621784821874999949 ) ) ;
#48991 = CARTESIAN_POINT ( 'NONE',  ( 19.76250000122903216, 0.000000000000000000, 4.999999999999998224 ) ) ;
#48992 = ORIENTED_EDGE ( 'NONE', *, *, #7054, .F. ) ;
#48993 = CARTESIAN_POINT ( 'NONE',  ( 26.69062500061451715, -3.027376345333614438, 5.243569643749998122 ) ) ;
#48994 = CARTESIAN_POINT ( 'NONE',  ( 27.98437500061451289, 4.541064518000418104, 2.621784821874999949 ) ) ;
#48995 = CARTESIAN_POINT ( 'NONE',  ( 16.78125000122903288, 6.123233995736764310E-16, -4.999999999999998224 ) ) ;
#48996 = CARTESIAN_POINT ( 'NONE',  ( 14.96250000000000036, 2.886751345948129099, -4.999999999999998224 ) ) ;
#48997 = CARTESIAN_POINT ( 'NONE',  ( 10.34062500061451750, 6.054752690667223547, 3.707466751127219781E-16 ) ) ;
#48998 = CARTESIAN_POINT ( 'NONE',  ( 14.17500000000000071, 4.330127018922191873, 2.499999999999999556 ) ) ;
#48999 = CARTESIAN_POINT ( 'NONE',  ( 29.54062500061451502, -3.027376345333610441, -5.243569643749999898 ) ) ;
#49000 = CARTESIAN_POINT ( 'NONE',  ( 16.05000000122903359, 5.773502691896255534, 3.535250795749688894E-16 ) ) ;
#49001 = CARTESIAN_POINT ( 'NONE',  ( 0.000000000000000000, 0.000000000000000000, 50.00000000000000000 ) ) ;
#49002 = CARTESIAN_POINT ( 'NONE',  ( 14.78437500061451715, 5.824947211148865298E-16, -4.756430356249998326 ) ) ;
#49003 = CARTESIAN_POINT ( 'NONE',  ( 5.578125000614518214, -4.541064518000419881, 2.621784821874995952 ) ) ;
#49004 = CARTESIAN_POINT ( 'NONE',  ( 20.85937500061451644, 0.000000000000000000, 5.243569643749999010 ) ) ;
#49005 = CARTESIAN_POINT ( 'NONE',  ( 9.001249775931846008E-16, 17.27187500061451786, 34.90005215228797653 ) ) ;
#49006 = CARTESIAN_POINT ( 'NONE',  ( 22.99687500061451573, 6.054752690667223547, 3.707466751127219781E-16 ) ) ;
#49007 = CARTESIAN_POINT ( 'NONE',  ( 6.299999999999999822, -4.330127018922190985, -2.500000000000001332 ) ) ;
#49008 = CARTESIAN_POINT ( 'NONE',  ( 3.999999999999998668, 10.47500000122903430, 27.69059892324149175 ) ) ;
#49009 = CARTESIAN_POINT ( 'NONE',  ( 13.22812500061451502, -4.541064518000419881, 2.621784821874995952 ) ) ;
#49010 = CARTESIAN_POINT ( 'NONE',  ( 5.400000001229032343, -2.886751345948129988, 4.999999999999997335 ) ) ;
#49011 = CARTESIAN_POINT ( 'NONE',  ( 9.009375000614518569, 4.541064518000418104, -2.621784821874998173 ) ) ;
#49012 = DIRECTION ( 'NONE',  ( -1.000000000000000000, -0.000000000000000000, -0.000000000000000000 ) ) ;
#49013 = AXIS2_PLACEMENT_3D ( 'NONE', #7203, #33829, #6844 ) ;
#49014 = CARTESIAN_POINT ( 'NONE',  ( 10.86562500061451431, 3.027376345333611329, 5.243569643749999010 ) ) ;
#49015 = CARTESIAN_POINT ( 'NONE',  ( 13.95937500061451786, 4.541064518000418104, -2.621784821874998173 ) ) ;
#49016 = DIRECTION ( 'NONE',  ( 0.000000000000000000, 0.000000000000000000, 1.000000000000000000 ) ) ;
#49017 = CARTESIAN_POINT ( 'NONE',  ( 21.18750000122903288, -4.330127018922194537, 2.499999999999995559 ) ) ;
#49018 = CARTESIAN_POINT ( 'NONE',  ( 10.09687500061451715, -3.027376345333614438, 5.243569643749998122 ) ) ;
#49019 = CARTESIAN_POINT ( 'NONE',  ( 11.65312500061451573, 4.541064518000418104, -2.621784821874998173 ) ) ;
#49020 = ADVANCED_FACE ( 'NONE', ( #72098 ), #328, .F. ) ;
#49021 = CARTESIAN_POINT ( 'NONE',  ( 27.88125000122903074, -4.330127018922194537, 2.499999999999995559 ) ) ;
#49022 = CARTESIAN_POINT ( 'NONE',  ( 22.58437500061451431, 4.541064518000418104, 2.621784821874999949 ) ) ;
#49023 = CARTESIAN_POINT ( 'NONE',  ( 25.38750000122903216, 6.123233995736764310E-16, -4.999999999999998224 ) ) ;
#49024 = CARTESIAN_POINT ( 'NONE',  ( -2.081578678577454156, 4.574985540471383061, 26.54335022361717478 ) ) ;
#49025 = CARTESIAN_POINT ( 'NONE',  ( 3.486133158594716510E-16, 19.88749999999999929, -34.00000000000000000 ) ) ;
#49026 = CARTESIAN_POINT ( 'NONE',  ( -4.243569643749998122, 11.34687500061451892, -27.54997392385601174 ) ) ;
#49027 = CARTESIAN_POINT ( 'NONE',  ( 15.07500000122903394, 2.886751345948129099, -4.999999999999998224 ) ) ;
#49028 = VECTOR ( 'NONE', #10467, 1000.000000000000000 ) ;
#49029 = CARTESIAN_POINT ( 'NONE',  ( 10.17187500061451999, -6.054752690667223547, -1.112240025338166033E-15 ) ) ;
#49030 = CARTESIAN_POINT ( 'NONE',  ( 2.121784821874999061, 17.40312500061451573, -33.67503911421598417 ) ) ;
#49031 = CARTESIAN_POINT ( 'NONE',  ( 18.03750000122903430, -4.330127018922194537, 2.499999999999995559 ) ) ;
#49032 = CARTESIAN_POINT ( 'NONE',  ( 10.49062500061451431, -3.027376345333614438, 5.243569643749998122 ) ) ;
#49033 = ORIENTED_EDGE ( 'NONE', *, *, #24479, .T. ) ;
#49034 = AXIS2_PLACEMENT_3D ( 'NONE', #46605, #17778, #1549 ) ;
#49035 = CARTESIAN_POINT ( 'NONE',  ( 14.96250000000000036, 2.886751345948129099, -4.999999999999998224 ) ) ;
#49036 = CARTESIAN_POINT ( 'NONE',  ( -1.071796769724488563, 17.50490381179670152, -26.00000000000000000 ) ) ;
#49037 = CARTESIAN_POINT ( 'NONE',  ( 9.534375000614517148, 4.541064518000418104, 2.621784821874999949 ) ) ;
#49038 = CARTESIAN_POINT ( 'NONE',  ( 4.373597137442938099, -2.423175050767027550, -4.650093653908929703 ) ) ;
#49039 = CARTESIAN_POINT ( 'NONE',  ( 10.35000000122903074, -2.886751345948129988, 4.999999999999997335 ) ) ;
#49040 = CARTESIAN_POINT ( 'NONE',  ( 18.18750000122903288, 6.123233995736764310E-16, -4.999999999999998224 ) ) ;
#49041 = CARTESIAN_POINT ( 'NONE',  ( 14.09062500061451750, -3.027376345333614438, 5.243569643749998122 ) ) ;
#49042 =( BOUNDED_CURVE ( )  B_SPLINE_CURVE ( 2, ( #50018, #32287, #54821, #72542, #45567, #39297, #67730 ),
 .UNSPECIFIED., .F., .F. ) 
 B_SPLINE_CURVE_WITH_KNOTS ( ( 3, 2, 2, 3 ),
 ( 0.5400000000000001465, 0.5433333333333333348, 0.5466666666666666341, 0.5499999999999999334 ),
 .UNSPECIFIED. ) 
 CURVE ( )  GEOMETRIC_REPRESENTATION_ITEM ( )  RATIONAL_B_SPLINE_CURVE ( ( 0.9999999999999955591, 0.8660254037844431485, 1.000000000000000000, 0.8660254037844387076, 1.000000000000000000, 0.8660254037844431485, 0.9999999999999955591 ) ) 
 REPRESENTATION_ITEM ( '' )  );
#49043 = CARTESIAN_POINT ( 'NONE',  ( 17.42812500061451786, 6.421520780324663323E-16, -5.243569643749999010 ) ) ;
#49044 = CARTESIAN_POINT ( 'NONE',  ( 27.03750000122903430, -4.330127018922194537, 2.499999999999995559 ) ) ;
#49045 = CARTESIAN_POINT ( 'NONE',  ( 4.003125000614518925, 4.541064518000418104, -2.621784821874998173 ) ) ;
#49046 = CARTESIAN_POINT ( 'NONE',  ( 24.00000000000000000, 4.330127018922192761, -2.499999999999997780 ) ) ;
#49047 = CARTESIAN_POINT ( 'NONE',  ( -7.967954043666661671E-16, 12.97812499938548392, 34.33755215474603517 ) ) ;
#49048 = CARTESIAN_POINT ( 'NONE',  ( 27.52500000000000213, 6.123233995736764310E-16, -4.999999999999998224 ) ) ;
#49049 = CARTESIAN_POINT ( 'NONE',  ( 25.92187500061451999, -6.054752690667223547, -1.112240025338166033E-15 ) ) ;
#49050 = CARTESIAN_POINT ( 'NONE',  ( 1.071796769724489895, 12.66740381056766651, -34.00000000000000000 ) ) ;
#49051 = CARTESIAN_POINT ( 'NONE',  ( 13.72500000122903074, 2.886751345948129099, -4.999999999999998224 ) ) ;
#49052 = CARTESIAN_POINT ( 'NONE',  ( 3.487500000000000711, -2.886751345948129988, 4.999999999999997335 ) ) ;
#49053 = PLANE ( 'NONE',  #60849 ) ;
#49054 = CARTESIAN_POINT ( 'NONE',  ( 6.309375000614517504, 4.541064518000418104, -2.621784821874998173 ) ) ;
#49055 = CARTESIAN_POINT ( 'NONE',  ( 26.61562500061451786, 3.027376345333611329, 5.243569643749999010 ) ) ;
#49056 = CARTESIAN_POINT ( 'NONE',  ( 3.756430356250000102, 12.75312499938548427, 30.00000000000000000 ) ) ;
#49057 = CARTESIAN_POINT ( 'NONE',  ( 11.55000000122903181, 5.773502691896255534, 3.535250795749688401E-16 ) ) ;
#49058 = PRESENTATION_LAYER_ASSIGNMENT (  '', '', ( #13649 ) ) ;
#49059 = CARTESIAN_POINT ( 'NONE',  ( 5.896875000614518747, 6.054752690667223547, 3.707466751127219781E-16 ) ) ;
#49060 = CARTESIAN_POINT ( 'NONE',  ( 8.971875000614515372, 3.027376345333613106, -5.243569643749998122 ) ) ;
#49061 = CARTESIAN_POINT ( 'NONE',  ( 29.33437500061451431, 4.541064518000418104, 2.621784821874999949 ) ) ;
#49062 = CARTESIAN_POINT ( 'NONE',  ( 9.001249775931846008E-16, 11.81562500061459353, 34.90005215228797653 ) ) ;
#49063 = CARTESIAN_POINT ( 'NONE',  ( 22.31250000000000000, 2.886751345948126879, 4.999999999999999112 ) ) ;
#49064 = CARTESIAN_POINT ( 'NONE',  ( 29.51249999999999929, 2.886751345948126879, 4.999999999999999112 ) ) ;
#49065 = CARTESIAN_POINT ( 'NONE',  ( 5.100000000000000533, 4.330127018922192761, -2.499999999999997780 ) ) ;
#49066 = EDGE_CURVE ( 'NONE', #37967, #18378, #66557, .T. ) ;
#49067 = ORIENTED_EDGE ( 'NONE', *, *, #59834, .F. ) ;
#49068 = CARTESIAN_POINT ( 'NONE',  ( 17.09062500061451573, 6.054752690667223547, 3.707466751127219781E-16 ) ) ;
#49069 = CARTESIAN_POINT ( 'NONE',  ( 10.75312500061451715, 4.541064518000418104, -2.621784821874998173 ) ) ;
#49070 = CARTESIAN_POINT ( 'NONE',  ( 20.82187500061451502, -4.119189519843968306, 2.378215178124996054 ) ) ;
#49071 = CARTESIAN_POINT ( 'NONE',  ( 7.134375000614516793, 6.421520780324663323E-16, -5.243569643749999010 ) ) ;
#49072 = CARTESIAN_POINT ( 'NONE',  ( 23.09999999999999787, 4.330127018922192761, -2.499999999999997780 ) ) ;
#49073 = CARTESIAN_POINT ( 'NONE',  ( 20.55000000122903359, 5.773502691896255534, 3.535250795749688894E-16 ) ) ;
#49074 = CARTESIAN_POINT ( 'NONE',  ( 15.91875000122902684, 2.886751345948018077, -5.000000000000190070 ) ) ;
#49075 = VECTOR ( 'NONE', #26815, 1000.000000000000000 ) ;
#49076 = CARTESIAN_POINT ( 'NONE',  ( 8.559375000614515727, 4.541064518000418104, -2.621784821874998173 ) ) ;
#49077 = CARTESIAN_POINT ( 'NONE',  ( 15.00937500061451679, 0.000000000000000000, 5.243569643749999010 ) ) ;
#49078 = CARTESIAN_POINT ( 'NONE',  ( 24.00937500061451502, 0.000000000000000000, 5.243569643749999010 ) ) ;
#49079 = CARTESIAN_POINT ( 'NONE',  ( 23.40000000000000213, -4.330127018922190985, -2.500000000000001332 ) ) ;
#49080 = ORIENTED_EDGE ( 'NONE', *, *, #1611, .T. ) ;
#49081 = CARTESIAN_POINT ( 'NONE',  ( 14.06250000000000000, 2.886751345948129099, -4.999999999999998224 ) ) ;
#49082 = CARTESIAN_POINT ( 'NONE',  ( 18.42187500061451644, 3.027376345333613106, -5.243569643749998122 ) ) ;
#49083 =( BOUNDED_CURVE ( )  B_SPLINE_CURVE ( 2, ( #43834, #66359, #56004, #67104, #15736, #16462, #33459, #5398, #50468 ),
 .UNSPECIFIED., .F., .F. ) 
 B_SPLINE_CURVE_WITH_KNOTS ( ( 3, 2, 2, 2, 3 ),
 ( 0.4239130434782608647, 0.4275362318840579823, 0.4347826086956521618, 0.4420289855072463969, 0.4456521739130435145 ),
 .UNSPECIFIED. ) 
 CURVE ( )  GEOMETRIC_REPRESENTATION_ITEM ( )  RATIONAL_B_SPLINE_CURVE ( ( 0.9330127018922194093, 0.9330127018922194093, 1.000000000000000000, 0.8660254037844387076, 1.000000000000000000, 0.8660254037844387076, 1.000000000000000000, 0.9330127018922188542, 0.9330127018922194093 ) ) 
 REPRESENTATION_ITEM ( '' )  );
#49084 = CARTESIAN_POINT ( 'NONE',  ( 8.934375000614517504, 6.421520780324663323E-16, -5.243569643749999010 ) ) ;
#49085 = CARTESIAN_POINT ( 'NONE',  ( 2.655984681222220721E-16, 13.65312499938548463, 25.66244784525396483 ) ) ;
#49086 = CARTESIAN_POINT ( 'NONE',  ( 19.98749999999999716, 5.773502691896255534, 3.535250795749688894E-16 ) ) ;
#49087 = CARTESIAN_POINT ( 'NONE',  ( -2.000000000000001776, 14.15000000000000036, 33.46410161513775705 ) ) ;
#49088 = CARTESIAN_POINT ( 'NONE',  ( 4.243569643749999898, 10.14687500061451786, -27.54997392385601529 ) ) ;
#49089 = CARTESIAN_POINT ( 'NONE',  ( 22.99687500061451573, 5.492252693125287522, 3.363034840372157021E-16 ) ) ;
#49090 = CARTESIAN_POINT ( 'NONE',  ( 12.21562500061451573, 3.027376345333611329, 5.243569643749999010 ) ) ;
#49091 = CARTESIAN_POINT ( 'NONE',  ( 29.55937500061451573, -4.541064518000417216, -2.621784821875001281 ) ) ;
#49092 = CYLINDRICAL_SURFACE ( 'NONE', #27959, 4.999999999999998224 ) ;
#49093 = CARTESIAN_POINT ( 'NONE',  ( 12.30000000000000249, 4.330127018922192761, -2.499999999999997780 ) ) ;
#49094 = CARTESIAN_POINT ( 'NONE',  ( -3.999999999999999112, 17.41250000122903430, 30.00000000000000000 ) ) ;
#49095 = CARTESIAN_POINT ( 'NONE',  ( 11.73750000122903181, -4.330127018922194537, 2.499999999999995559 ) ) ;
#49096 = CARTESIAN_POINT ( 'NONE',  ( 21.23437500061451644, 4.541064518000418104, 2.621784821874999949 ) ) ;
#49097 = CARTESIAN_POINT ( 'NONE',  ( 16.43437500061451573, -4.541064518000419881, 2.621784821874995952 ) ) ;
#49098 = LINE ( 'NONE', #49825, #50165 ) ;
#49099 = ORIENTED_EDGE ( 'NONE', *, *, #25255, .F. ) ;
#49100 = CARTESIAN_POINT ( 'NONE',  ( 16.67812500061451786, 4.541064518000418104, 2.621784821874999949 ) ) ;
#49101 = CARTESIAN_POINT ( 'NONE',  ( 27.67500000122903359, 2.886751345948129099, -4.999999999999998224 ) ) ;
#49102 = CARTESIAN_POINT ( 'NONE',  ( 18.27187500061451431, -6.054752690667223547, -1.112240025338166033E-15 ) ) ;
#49103 = CARTESIAN_POINT ( 'NONE',  ( 5.803125000614517859, 4.541064518000418104, -2.621784821874998173 ) ) ;
#49104 = CARTESIAN_POINT ( 'NONE',  ( 20.31562500061451715, 3.027376345333611329, 5.243569643749999010 ) ) ;
#49105 = CARTESIAN_POINT ( 'NONE',  ( -3.999999999999997335, 16.88749999999999929, -27.69059892324149530 ) ) ;
#49106 = CARTESIAN_POINT ( 'NONE',  ( 27.75937500061451502, -4.541064518000417216, -2.621784821875001281 ) ) ;
#49107 = CARTESIAN_POINT ( 'NONE',  ( -4.243569643749997233, 13.54062500061451679, 32.45002607614398471 ) ) ;
#49108 = CARTESIAN_POINT ( 'NONE',  ( 16.80937500061451573, 0.000000000000000000, 5.243569643749999010 ) ) ;
#49109 = CARTESIAN_POINT ( 'NONE',  ( 15.78750000122903430, -4.330127018922194537, 2.499999999999995559 ) ) ;
#49110 = CARTESIAN_POINT ( 'NONE',  ( 10.54687500061451644, -2.746126346562646425, 4.756430356249996549 ) ) ;
#49111 = CARTESIAN_POINT ( 'NONE',  ( 2.000000000000001332, 18.91250000122903430, -26.53589838486224650 ) ) ;
#49112 = CARTESIAN_POINT ( 'NONE',  ( 20.70937500061451786, 4.541064518000418104, -2.621784821874998173 ) ) ;
#49113 = CARTESIAN_POINT ( 'NONE',  ( 21.78750000122903074, 6.123233995736764310E-16, -4.999999999999998224 ) ) ;
#49114 =( BOUNDED_CURVE ( )  B_SPLINE_CURVE ( 2, ( #2441, #24964, #70038, #41971, #13884, #70409, #19785 ),
 .UNSPECIFIED., .F., .F. ) 
 B_SPLINE_CURVE_WITH_KNOTS ( ( 3, 2, 2, 3 ),
 ( 0.1799999999999999378, 0.1833333333333333204, 0.1866666666666667029, 0.1900000000000000855 ),
 .UNSPECIFIED. ) 
 CURVE ( )  GEOMETRIC_REPRESENTATION_ITEM ( )  RATIONAL_B_SPLINE_CURVE ( ( 1.000000000000002220, 0.8660254037844364872, 1.000000000000000000, 0.8660254037844387076, 1.000000000000000000, 0.8660254037844353769, 1.000000000000003331 ) ) 
 REPRESENTATION_ITEM ( '' )  );
#49115 = CARTESIAN_POINT ( 'NONE',  ( 23.65312500061451573, -4.541064518000417216, -2.621784821875001281 ) ) ;
#49116 = CARTESIAN_POINT ( 'NONE',  ( 16.54687500061451644, -3.027376345333610441, -5.243569643749999898 ) ) ;
#49117 = CARTESIAN_POINT ( 'NONE',  ( 12.29062500061451857, -3.027376345333614438, 5.243569643749998122 ) ) ;
#49118 = CARTESIAN_POINT ( 'NONE',  ( 2.121784821875001281, 14.15937500061451715, 33.67503911421598417 ) ) ;
#49119 = CARTESIAN_POINT ( 'NONE',  ( 18.40312500061451573, 4.541064518000418104, -2.621784821874998173 ) ) ;
#49120 = CARTESIAN_POINT ( 'NONE',  ( 28.71562500061451573, 3.027376345333613106, -5.243569643749998122 ) ) ;
#49121 = ORIENTED_EDGE ( 'NONE', *, *, #26290, .T. ) ;
#49122 = CARTESIAN_POINT ( 'NONE',  ( 22.31250000000000000, 2.886751345948126879, 4.999999999999999112 ) ) ;
#49123 = CARTESIAN_POINT ( 'NONE',  ( -4.243569643749999898, 18.92187500061451644, -32.45002607614398471 ) ) ;
#49124 = CARTESIAN_POINT ( 'NONE',  ( 3.734827092922140768, -3.324314453528163682, -3.734827092927292203 ) ) ;
#49125 = CARTESIAN_POINT ( 'NONE',  ( 25.11562500061451431, 3.027376345333613106, -5.243569643749998122 ) ) ;
#49126 = CARTESIAN_POINT ( 'NONE',  ( 5.765625000614519102, 3.027376345333613106, -5.243569643749998122 ) ) ;
#49127 = CARTESIAN_POINT ( 'NONE',  ( 17.81250000122903288, 4.330127018922192761, -2.499999999999997780 ) ) ;
#49128 = ADVANCED_FACE ( 'NONE', ( #68651 ), #38486, .F. ) ;
#49129 = CARTESIAN_POINT ( 'NONE',  ( 22.19062500061451715, -3.027376345333614438, 5.243569643749998122 ) ) ;
#49130 = CARTESIAN_POINT ( 'NONE',  ( 21.78750000000000142, 5.773502691896255534, 3.535250795749688894E-16 ) ) ;
#49131 = CARTESIAN_POINT ( 'NONE',  ( 27.96562500061451928, 3.027376345333611329, 5.243569643749999010 ) ) ;
#49132 = CARTESIAN_POINT ( 'NONE',  ( 7.228125000614517681, 4.541064518000418104, 2.621784821874999949 ) ) ;
#49133 = ORIENTED_EDGE ( 'NONE', *, *, #47219, .F. ) ;
#49134 = CARTESIAN_POINT ( 'NONE',  ( 23.42812500061451786, 4.541064518000418104, 2.621784821874999949 ) ) ;
#49135 = CARTESIAN_POINT ( 'NONE',  ( 3.778125000614519280, -4.541064518000419881, 2.621784821874995952 ) ) ;
#49136 = CARTESIAN_POINT ( 'NONE',  ( 11.74687500061451573, 5.492252693125287522, 3.363034840372157021E-16 ) ) ;
#49137 = CARTESIAN_POINT ( 'NONE',  ( 20.15625000122903288, 0.000000000000000000, 4.999999999999998224 ) ) ;
#49138 = CARTESIAN_POINT ( 'NONE',  ( -1.999999999999997113, 13.88750000122903394, -26.53589838486224295 ) ) ;
#49139 = DIRECTION ( 'NONE',  ( -1.000000000000000000, -0.000000000000000000, -0.000000000000000000 ) ) ;
#49140 = CARTESIAN_POINT ( 'NONE',  ( 11.40000000000000036, 4.330127018922192761, -2.499999999999997780 ) ) ;
#49141 = CARTESIAN_POINT ( 'NONE',  ( 11.52187500061451608, -6.054752690667223547, -1.112240025338166033E-15 ) ) ;
#49142 = CARTESIAN_POINT ( 'NONE',  ( 5.437500001229035540, -4.330127018922194537, 2.499999999999995559 ) ) ;
#49143 = CARTESIAN_POINT ( 'NONE',  ( 14.10937500061451644, 0.000000000000000000, 5.243569643749999010 ) ) ;
#49144 = CARTESIAN_POINT ( 'NONE',  ( 4.884375000614518569, 6.421520780324663323E-16, -5.243569643749999010 ) ) ;
#49145 = CARTESIAN_POINT ( 'NONE',  ( 16.80000000000000071, 4.330127018922192761, -2.499999999999997780 ) ) ;
#49146 = AXIS2_PLACEMENT_3D ( 'NONE', #53900, #9191, #19523 ) ;
#49147 = CARTESIAN_POINT ( 'NONE',  ( -5.810221930991193690E-16, 10.55000000122903359, 26.00000000000000355 ) ) ;
#49148 = CARTESIAN_POINT ( 'NONE',  ( 12.00937500061451857, -4.541064518000417216, -2.621784821875001281 ) ) ;
#49149 = CARTESIAN_POINT ( 'NONE',  ( 6.225000001229035185, 2.886751345948126879, 4.999999999999998224 ) ) ;
#49150 = CARTESIAN_POINT ( 'NONE',  ( 22.37812500061451360, 6.421520780324663323E-16, -5.243569643749999010 ) ) ;
#49151 = DIRECTION ( 'NONE',  ( -0.000000000000000000, -1.000000000000000000, -0.000000000000000000 ) ) ;
#49152 = CARTESIAN_POINT ( 'NONE',  ( -4.243569643749998122, 18.49062500061459247, 32.45002607614398471 ) ) ;
#49153 = CARTESIAN_POINT ( 'NONE',  ( 24.08437500061451786, -4.541064518000419881, 2.621784821874995952 ) ) ;
#49154 = CARTESIAN_POINT ( 'NONE',  ( -2.000000000000000000, 13.73750000122903359, -33.46410161513775705 ) ) ;
#49155 = CARTESIAN_POINT ( 'NONE',  ( 4.265625000614517326, -6.054752690667223547, -1.112240025338166033E-15 ) ) ;
#49156 = CARTESIAN_POINT ( 'NONE',  ( 21.23437500061451644, -2.746126346562646425, 4.756430356249996549 ) ) ;
#49157 = CARTESIAN_POINT ( 'NONE',  ( 25.52812500061451573, 6.421520780324663323E-16, -5.243569643749999010 ) ) ;
#49158 = CARTESIAN_POINT ( 'NONE',  ( 17.35312500061451502, -4.541064518000417216, -2.621784821875001281 ) ) ;
#49159 = CARTESIAN_POINT ( 'NONE',  ( 14.15625000122903288, 4.330127018922192761, -2.499999999999997780 ) ) ;
#49160 = CARTESIAN_POINT ( 'NONE',  ( 14.89687500061451786, 6.054752690667223547, 3.707466751127219781E-16 ) ) ;
#49161 = CARTESIAN_POINT ( 'NONE',  ( -3.999999999999999112, 15.83750000000000036, 27.69059892324149530 ) ) ;
#49162 = CARTESIAN_POINT ( 'NONE',  ( 27.56250000122902932, -4.330127018922190985, -2.500000000000001332 ) ) ;
#49163 = CARTESIAN_POINT ( 'NONE',  ( 6.646875000614518747, -3.027376345333610441, -5.243569643749999898 ) ) ;
#49164 = CARTESIAN_POINT ( 'NONE',  ( 17.14687500061451786, 6.054752690667223547, 3.707466751127219781E-16 ) ) ;
#49165 = FACE_OUTER_BOUND ( 'NONE', #13997, .T. ) ;
#49166 = CARTESIAN_POINT ( 'NONE',  ( 24.03750000000000142, 5.773502691896255534, 3.535250795749688894E-16 ) ) ;
#49167 = CARTESIAN_POINT ( 'NONE',  ( 2.925000001229034918, 2.886751345948129099, -4.999999999999998224 ) ) ;
#49168 = CARTESIAN_POINT ( 'NONE',  ( 25.65937500061451715, 4.541064518000418104, -2.621784821874998173 ) ) ;
#49169 = CARTESIAN_POINT ( 'NONE',  ( 15.83437500061451608, 4.541064518000418104, 2.621784821874999949 ) ) ;
#49170 = CARTESIAN_POINT ( 'NONE',  ( -1.878215178125001827, 13.50312499938548427, 33.25316411605952283 ) ) ;
#49171 = CARTESIAN_POINT ( 'NONE',  ( 27.22499999999999787, 4.330127018922191873, 2.499999999999999556 ) ) ;
#49172 = CARTESIAN_POINT ( 'NONE',  ( 4.949999999999999289, -4.330127018922190985, -2.500000000000001332 ) ) ;
#49173 = CARTESIAN_POINT ( 'NONE',  ( 10.47187500061451715, -4.119189519843968306, 2.378215178124996054 ) ) ;
#49174 = CARTESIAN_POINT ( 'NONE',  ( 18.55312500061451431, 0.000000000000000000, 5.243569643749999010 ) ) ;
#49175 = CARTESIAN_POINT ( 'NONE',  ( 9.074999999999999289, 6.123233995736764310E-16, -4.999999999999998224 ) ) ;
#49176 = EDGE_CURVE ( 'NONE', #72969, #24589, #43957, .T. ) ;
#49177 = CARTESIAN_POINT ( 'NONE',  ( 3.103125000614517237, 4.541064518000418104, -2.621784821874998173 ) ) ;
#49178 = CARTESIAN_POINT ( 'NONE',  ( 20.28750000000000142, -2.886751345948125991, -5.000000000000000000 ) ) ;
#49179 = DIRECTION ( 'NONE',  ( 0.000000000000000000, 0.000000000000000000, -1.000000000000000000 ) ) ;
#49180 = CARTESIAN_POINT ( 'NONE',  ( 24.37500000122903288, -5.773502691896255534, -1.060575238724906372E-15 ) ) ;
#49181 = CARTESIAN_POINT ( 'NONE',  ( 1.968632615237263517, 9.806224642577900497, 35.67136274582625788 ) ) ;
#49182 = CARTESIAN_POINT ( 'NONE',  ( 28.54687500061451644, -3.027376345333614438, 5.243569643749998122 ) ) ;
#49183 = EDGE_LOOP ( 'NONE', ( #25993, #33169, #67787, #23791 ) ) ;
#49184 = CARTESIAN_POINT ( 'NONE',  ( 18.21562500061451573, -6.054752690667223547, -1.112240025338166033E-15 ) ) ;
#49185 = CARTESIAN_POINT ( 'NONE',  ( 23.69062500061451004, -3.027376345333610441, -5.243569643749999898 ) ) ;
#49186 = CARTESIAN_POINT ( 'NONE',  ( 24.12187500061451217, -6.054752690667223547, -1.112240025338166033E-15 ) ) ;
#49187 = CARTESIAN_POINT ( 'NONE',  ( 9.637499999999999289, 5.773502691896255534, 3.535250795749688894E-16 ) ) ;
#49188 = CARTESIAN_POINT ( 'NONE',  ( 12.17812500061451608, 4.541064518000418104, 2.621784821874999949 ) ) ;
#49189 = CARTESIAN_POINT ( 'NONE',  ( 27.29062500061451502, -3.027376345333610441, -5.243569643749999898 ) ) ;
#49190 = CARTESIAN_POINT ( 'NONE',  ( 15.15937500061451715, -4.541064518000417216, -2.621784821875001281 ) ) ;
#49191 = CARTESIAN_POINT ( 'NONE',  ( 19.73437500061451644, 6.421520780324663323E-16, -5.243569643749999010 ) ) ;
#49192 = CARTESIAN_POINT ( 'NONE',  ( 9.001249775931846008E-16, 19.01562500061451644, 34.90005215228797653 ) ) ;
#49193 = CARTESIAN_POINT ( 'NONE',  ( 23.51250000122903216, -4.330127018922190985, -2.500000000000001332 ) ) ;
#49194 = CARTESIAN_POINT ( 'NONE',  ( 17.97187500061451715, 2.746126346562645981, -4.756430356249997438 ) ) ;
#49195 = CARTESIAN_POINT ( 'NONE',  ( 14.09062500061451750, -3.027376345333614438, 5.243569643749998122 ) ) ;
#49196 = CARTESIAN_POINT ( 'NONE',  ( 7.734375000614517326, 4.541064518000418104, 2.621784821874999949 ) ) ;
#49197 = CARTESIAN_POINT ( 'NONE',  ( 7.734375000614517326, 4.541064518000418104, 2.621784821874999949 ) ) ;
#49198 = ORIENTED_EDGE ( 'NONE', *, *, #36389, .T. ) ;
#49199 = CARTESIAN_POINT ( 'NONE',  ( 28.62187500061451573, -6.054752690667223547, -1.112240025338166033E-15 ) ) ;
#49200 = CARTESIAN_POINT ( 'NONE',  ( 19.79062500061451502, 6.054752690667223547, 3.707466751127219781E-16 ) ) ;
#49201 = CARTESIAN_POINT ( 'NONE',  ( 24.30937500061451573, 4.541064518000418104, -2.621784821874998173 ) ) ;
#49202 = CARTESIAN_POINT ( 'NONE',  ( 20.72812500061451502, 4.541064518000418104, 2.621784821874999949 ) ) ;
#49203 = CARTESIAN_POINT ( 'NONE',  ( -1.999999999999997113, 11.97500000000000142, 33.46410161513775705 ) ) ;
#49204 = CARTESIAN_POINT ( 'NONE',  ( 25.34062500061451217, -3.027376345333614438, 5.243569643749998122 ) ) ;
#49205 = CARTESIAN_POINT ( 'NONE',  ( 8.250000001229034652, -2.886751345948125991, -5.000000000000000000 ) ) ;
#49206 = EDGE_LOOP ( 'NONE', ( #16193, #54355, #1203, #10056 ) ) ;
#49207 = CARTESIAN_POINT ( 'NONE',  ( 3.337500001229034563, 6.123233995736764310E-16, -4.999999999999998224 ) ) ;
#49208 = CARTESIAN_POINT ( 'NONE',  ( 3.999999999999998668, 14.86250000000000071, -32.30940107675850470 ) ) ;
#49209 = CARTESIAN_POINT ( 'NONE',  ( 22.50000000122903288, -2.886751345948129988, 4.999999999999997335 ) ) ;
#49210 = CARTESIAN_POINT ( 'NONE',  ( -3.756430356250001434, 15.71562499938548108, 32.16877607737301048 ) ) ;
#49211 = CARTESIAN_POINT ( 'NONE',  ( 3.721875000614518036, 3.027376345333611329, 5.243569643749999010 ) ) ;
#49212 = CARTESIAN_POINT ( 'NONE',  ( 20.21250000122903145, 0.000000000000000000, 4.999999999999998224 ) ) ;
#49213 = CARTESIAN_POINT ( 'NONE',  ( 13.00312500061451537, 4.541064518000418104, -2.621784821874998173 ) ) ;
#49214 = AXIS2_PLACEMENT_3D ( 'NONE', #4379, #45347, #66421 ) ;
#49215 = CARTESIAN_POINT ( 'NONE',  ( 8.971875000614515372, 3.027376345333613106, -5.243569643749998122 ) ) ;
#49216 = CARTESIAN_POINT ( 'NONE',  ( 24.41250000122903430, -4.330127018922190985, -2.500000000000001332 ) ) ;
#49217 = CARTESIAN_POINT ( 'NONE',  ( 15.49687500061451750, -3.027376345333614438, 5.243569643749998122 ) ) ;
#49218 = CARTESIAN_POINT ( 'NONE',  ( 29.69062500061451715, 6.054752690667223547, 3.707466751127219781E-16 ) ) ;
#49219 = CARTESIAN_POINT ( 'NONE',  ( 29.51249999999999929, 2.886751345948126879, 4.999999999999999112 ) ) ;
#49220 = CARTESIAN_POINT ( 'NONE',  ( 4.978125000614518569, 4.541064518000418104, 2.621784821874999949 ) ) ;
#49221 = CARTESIAN_POINT ( 'NONE',  ( 14.20312500061451644, -4.541064518000417216, -2.621784821875001281 ) ) ;
#49222 = VERTEX_POINT ( 'NONE', #57180 ) ;
#49223 = CARTESIAN_POINT ( 'NONE',  ( 12.29062500061451857, -3.027376345333614438, 5.243569643749998122 ) ) ;
#49224 = CARTESIAN_POINT ( 'NONE',  ( 8.578125000614518214, 4.541064518000418104, 2.621784821874999949 ) ) ;
#49225 = CARTESIAN_POINT ( 'NONE',  ( 17.63437500061451502, 4.119189519843966529, 2.378215178124999607 ) ) ;
#49226 = CARTESIAN_POINT ( 'NONE',  ( 7.987500000000000711, -2.886751345948129988, 4.999999999999997335 ) ) ;
#49227 = ADVANCED_FACE ( 'NONE', ( #49576 ), #51495, .T. ) ;
#49228 = CARTESIAN_POINT ( 'NONE',  ( 3.000000001229032875, 5.773502691896255534, 3.535250795749688894E-16 ) ) ;
#49229 = CARTESIAN_POINT ( 'NONE',  ( 17.96250000000000213, -5.773502691896255534, -1.060575238724906372E-15 ) ) ;
#49230 = CARTESIAN_POINT ( 'NONE',  ( 19.09687500061451360, -3.027376345333614438, 5.243569643749998122 ) ) ;
#49231 = CARTESIAN_POINT ( 'NONE',  ( 13.16250000122903430, -4.330127018922190985, -2.500000000000001332 ) ) ;
#49232 = CARTESIAN_POINT ( 'NONE',  ( 22.91249999999999432, -5.773502691896255534, -1.060575238724906372E-15 ) ) ;
#49233 = CARTESIAN_POINT ( 'NONE',  ( 2.121784821874999061, 16.50312500061451715, -33.67503911421598417 ) ) ;
#49234 = CARTESIAN_POINT ( 'NONE',  ( 22.12500000000000000, 6.123233995736764310E-16, -4.999999999999998224 ) ) ;
#49235 = DIRECTION ( 'NONE',  ( 0.000000000000000000, -8.673617379884036705E-17, -1.000000000000000000 ) ) ;
#49236 = CARTESIAN_POINT ( 'NONE',  ( 28.60312500061451502, -4.541064518000417216, -2.621784821875001281 ) ) ;
#49237 = CARTESIAN_POINT ( 'NONE',  ( 28.31249999999999645, -5.773502691896255534, -1.060575238724906372E-15 ) ) ;
#49238 = CARTESIAN_POINT ( 'NONE',  ( 0.000000000000000000, 0.000000000000000000, -50.00000000000000000 ) ) ;
#49239 = CARTESIAN_POINT ( 'NONE',  ( 13.35937500061451821, -4.541064518000417216, -2.621784821875001281 ) ) ;
#49240 = CARTESIAN_POINT ( 'NONE',  ( 25.72499999999999787, 6.123233995736764310E-16, -4.999999999999998224 ) ) ;
#49241 = CARTESIAN_POINT ( 'NONE',  ( 10.60312500061451679, -4.541064518000417216, -2.621784821875001281 ) ) ;
#49242 = CARTESIAN_POINT ( 'NONE',  ( 27.79687500061451289, 4.119189519843966529, -2.378215178124998275 ) ) ;
#49243 = CARTESIAN_POINT ( 'NONE',  ( 21.53437500061451715, 6.421520780324663323E-16, -5.243569643749999010 ) ) ;
#49244 = CARTESIAN_POINT ( 'NONE',  ( 13.88437500061451679, 5.492252693125287522, 3.363034840372157021E-16 ) ) ;
#49245 = CARTESIAN_POINT ( 'NONE',  ( 7.753125000614518036, 0.000000000000000000, 5.243569643749999010 ) ) ;
#49246 = CARTESIAN_POINT ( 'NONE',  ( 13.05937500061451750, 4.541064518000418104, -2.621784821874998173 ) ) ;
#49247 = ORIENTED_EDGE ( 'NONE', *, *, #45494, .T. ) ;
#49248 = CARTESIAN_POINT ( 'NONE',  ( 22.92187500061451644, 3.027376345333613106, -5.243569643749998122 ) ) ;
#49249 = CARTESIAN_POINT ( 'NONE',  ( 3.482548389542084344, 3.599757532507413149, -27.96763060114582444 ) ) ;
#49250 = CARTESIAN_POINT ( 'NONE',  ( 8.737500000000002487, 5.773502691896255534, 3.535250795749688401E-16 ) ) ;
#49251 = CARTESIAN_POINT ( 'NONE',  ( 4.687500000000000000, 5.773502691896255534, 3.535250795749688894E-16 ) ) ;
#49252 = VECTOR ( 'NONE', #50558, 1000.000000000000000 ) ;
#49253 = CARTESIAN_POINT ( 'NONE',  ( 17.77500000122903145, 2.886751345948129099, -4.999999999999998224 ) ) ;
#49254 = CARTESIAN_POINT ( 'NONE',  ( -1.999999999999999112, 19.79374999877096286, 26.53589838486224650 ) ) ;
#49255 = CARTESIAN_POINT ( 'NONE',  ( 9.271875000614517859, 5.824947211148865298E-16, -4.756430356249998326 ) ) ;
#49256 = EDGE_LOOP ( 'NONE', ( #62283, #7669, #27166, #53990 ) ) ;
#49257 = EDGE_CURVE ( 'NONE', #61968, #72906, #10510, .T. ) ;
#49258 = CARTESIAN_POINT ( 'NONE',  ( 15.59999999999999964, 0.000000000000000000, 4.999999999999998224 ) ) ;
#49259 = CARTESIAN_POINT ( 'NONE',  ( 16.94999999999999929, 0.000000000000000000, 4.999999999999998224 ) ) ;
#49260 = CARTESIAN_POINT ( 'NONE',  ( 11.42812500061451608, -4.541064518000419881, 2.621784821874995952 ) ) ;
#49261 = ORIENTED_EDGE ( 'NONE', *, *, #19955, .T. ) ;
#49262 = DIRECTION ( 'NONE',  ( 0.000000000000000000, 0.000000000000000000, 1.000000000000000000 ) ) ;
#49263 = CARTESIAN_POINT ( 'NONE',  ( -4.243569643749999898, 16.22187500061452070, -32.45002607614398471 ) ) ;
#49264 = CARTESIAN_POINT ( 'NONE',  ( 29.28750000122903074, -4.330127018922194537, 2.499999999999995559 ) ) ;
#49265 = CARTESIAN_POINT ( 'NONE',  ( 3.756430356249998770, 14.85312499938548214, 32.16877607737301759 ) ) ;
#49266 = CARTESIAN_POINT ( 'NONE',  ( 9.412499999999999645, -5.773502691896255534, -1.060575238724906372E-15 ) ) ;
#49267 = CARTESIAN_POINT ( 'NONE',  ( 30.00000000000000000, 0.000000000000000000, 0.000000000000000000 ) ) ;
#49268 = ORIENTED_EDGE ( 'NONE', *, *, #26320, .T. ) ;
#49269 = CARTESIAN_POINT ( 'NONE',  ( 23.31562500061451715, 3.027376345333613106, -5.243569643749998122 ) ) ;
#49270 = CARTESIAN_POINT ( 'NONE',  ( 4.201576942248188118, -2.710502447772806800, 4.488682300801404956 ) ) ;
#49271 = CARTESIAN_POINT ( 'NONE',  ( 3.756430356250000546, 18.97812499938548214, 27.83122392262697886 ) ) ;
#49272 = CARTESIAN_POINT ( 'NONE',  ( 20.55937500061451573, -4.541064518000417216, -2.621784821875001281 ) ) ;
#49273 = CARTESIAN_POINT ( 'NONE',  ( 20.27812500061451573, 4.541064518000418104, 2.621784821874999949 ) ) ;
#49274 = CARTESIAN_POINT ( 'NONE',  ( 2.121784821874999061, 14.25312500061459353, -33.67503911421598417 ) ) ;
#49275 = CARTESIAN_POINT ( 'NONE',  ( 23.43750000122902932, -4.330127018922194537, 2.499999999999995559 ) ) ;
#49276 = CARTESIAN_POINT ( 'NONE',  ( 4.340625000614515727, -3.027376345333610441, -5.243569643749999898 ) ) ;
#49277 = CARTESIAN_POINT ( 'NONE',  ( 23.18437500061451573, -4.119189519843968306, 2.378215178124996054 ) ) ;
#49278 = CARTESIAN_POINT ( 'NONE',  ( 21.89062500061451644, -3.027376345333610441, -5.243569643749999898 ) ) ;
#49279 = CARTESIAN_POINT ( 'NONE',  ( 8.109375000614518214, 4.119189519843966529, -2.378215178124998275 ) ) ;
#49280 = CARTESIAN_POINT ( 'NONE',  ( 3.756430356250000102, 17.59062499938548285, 30.00000000000000000 ) ) ;
#49281 = CARTESIAN_POINT ( 'NONE',  ( 14.78437500061451715, 6.421520780324663323E-16, -5.243569643749999010 ) ) ;
#49282 = CARTESIAN_POINT ( 'NONE',  ( 15.12187500061451750, -6.054752690667223547, -1.112240025338166033E-15 ) ) ;
#49283 = CARTESIAN_POINT ( 'NONE',  ( 22.84687500061451715, -3.027376345333610441, -5.243569643749999898 ) ) ;
#49284 = CARTESIAN_POINT ( 'NONE',  ( 9.001249775931846008E-16, 12.32187500061451857, 34.90005215228797653 ) ) ;
#49285 = CARTESIAN_POINT ( 'NONE',  ( 5.990625000614517859, -3.027376345333614438, 5.243569643749998122 ) ) ;
#49286 = CARTESIAN_POINT ( 'NONE',  ( 25.34062500061451217, -3.027376345333614438, 5.243569643749998122 ) ) ;
#49287 = CARTESIAN_POINT ( 'NONE',  ( 27.92812500061451431, 4.541064518000418104, 2.621784821874999949 ) ) ;
#49288 = CARTESIAN_POINT ( 'NONE',  ( 1.999999999999997335, 15.12500000000000000, 33.46410161513775705 ) ) ;
#49289 = CARTESIAN_POINT ( 'NONE',  ( 1.999999999999998668, 19.40000000000000213, 26.53589838486224650 ) ) ;
#49290 = CARTESIAN_POINT ( 'NONE',  ( 7.659375000614518036, 4.541064518000418104, -2.621784821874998173 ) ) ;
#49291 = DIRECTION ( 'NONE',  ( 1.000000000000000000, 0.000000000000000000, 0.000000000000000000 ) ) ;
#49292 = CARTESIAN_POINT ( 'NONE',  ( 13.65000000122903323, -2.886751345948125991, -5.000000000000000000 ) ) ;
#49293 = CARTESIAN_POINT ( 'NONE',  ( 10.35000000122903074, -2.886751345948129988, 4.999999999999997335 ) ) ;
#49294 = CARTESIAN_POINT ( 'NONE',  ( 29.43750000122903288, 6.123233995736764310E-16, -4.999999999999998224 ) ) ;
#49295 = CARTESIAN_POINT ( 'NONE',  ( 3.999999999999998668, 16.45624999877096784, 32.30940107675850470 ) ) ;
#49296 = CARTESIAN_POINT ( 'NONE',  ( 18.05625000122903501, -4.330127018922190985, -2.500000000000001332 ) ) ;
#49297 = CARTESIAN_POINT ( 'NONE',  ( 14.89687500061451786, 6.054752690667223547, 3.707466751127219781E-16 ) ) ;
#49298 = CARTESIAN_POINT ( 'NONE',  ( 11.96250000000000213, 2.886751345948126879, 4.999999999999998224 ) ) ;
#49299 = VERTEX_POINT ( 'NONE', #69401 ) ;
#49300 = CARTESIAN_POINT ( 'NONE',  ( 18.77812500061451573, 6.421520780324663323E-16, -5.243569643749999010 ) ) ;
#49301 = CARTESIAN_POINT ( 'NONE',  ( 8.503125000614515372, 4.541064518000418104, -2.621784821874998173 ) ) ;
#49302 = CARTESIAN_POINT ( 'NONE',  ( 21.45937500061451786, -4.541064518000417216, -2.621784821875001281 ) ) ;
#49303 = CARTESIAN_POINT ( 'NONE',  ( 5.053125000614517859, 0.000000000000000000, 5.243569643749999010 ) ) ;
#49304 = FACE_OUTER_BOUND ( 'NONE', #5862, .T. ) ;
#49305 = CARTESIAN_POINT ( 'NONE',  ( 7.050000001229036251, 5.773502691896255534, 3.535250795749688894E-16 ) ) ;
#49306 = CARTESIAN_POINT ( 'NONE',  ( 23.16562500061451502, -6.054752690667223547, -1.112240025338166033E-15 ) ) ;
#49307 = CARTESIAN_POINT ( 'NONE',  ( 3.999999999999998668, 17.22500000122903785, -32.30940107675850470 ) ) ;
#49308 = CARTESIAN_POINT ( 'NONE',  ( 10.68750000122903288, 4.330127018922191873, 2.499999999999999556 ) ) ;
#49309 = CARTESIAN_POINT ( 'NONE',  ( 18.89062500061451644, 6.054752690667223547, 3.707466751127219781E-16 ) ) ;
#49310 = CARTESIAN_POINT ( 'NONE',  ( 16.45312500061451289, -4.541064518000417216, -2.621784821875001281 ) ) ;
#49311 = CARTESIAN_POINT ( 'NONE',  ( 29.48437500061451644, -4.119189519843968306, 2.378215178124996054 ) ) ;
#49312 = CARTESIAN_POINT ( 'NONE',  ( 16.46249999999999503, 2.886751345948126879, 4.999999999999999112 ) ) ;
#49313 = CARTESIAN_POINT ( 'NONE',  ( 11.85000000122903430, -2.886751345948125991, -5.000000000000000000 ) ) ;
#49314 = CIRCLE ( 'NONE', #17427, 1.500000000000000444 ) ;
#49315 = CARTESIAN_POINT ( 'NONE',  ( 7.828125000614517326, -4.541064518000419881, 2.621784821874995952 ) ) ;
#49316 = CARTESIAN_POINT ( 'NONE',  ( 11.61562500061451608, 3.027376345333613106, -5.243569643749998122 ) ) ;
#49317 = EDGE_CURVE ( 'NONE', #43350, #26212, #13715, .T. ) ;
#49318 =( BOUNDED_CURVE ( )  B_SPLINE_CURVE ( 2, ( #3443, #25962, #20406, #48502, #31132, #14504, #41853 ),
 .UNSPECIFIED., .F., .F. ) 
 B_SPLINE_CURVE_WITH_KNOTS ( ( 3, 2, 2, 3 ),
 ( 0.7800000000000001377, 0.7833333333333334370, 0.7866666666666667362, 0.7900000000000001465 ),
 .UNSPECIFIED. ) 
 CURVE ( )  GEOMETRIC_REPRESENTATION_ITEM ( )  RATIONAL_B_SPLINE_CURVE ( ( 0.9999999999999955591, 0.8660254037844431485, 1.000000000000000000, 0.8660254037844387076, 1.000000000000000000, 0.8660254037844342667, 1.000000000000004441 ) ) 
 REPRESENTATION_ITEM ( '' )  );
#49319 = CARTESIAN_POINT ( 'NONE',  ( 21.63750000122903572, -4.330127018922194537, 2.499999999999995559 ) ) ;
#49320 = CARTESIAN_POINT ( 'NONE',  ( 19.77187500061451786, 3.027376345333613106, -5.243569643749998122 ) ) ;
#49321 = CARTESIAN_POINT ( 'NONE',  ( 25.05000000000000071, 0.000000000000000000, 4.999999999999998224 ) ) ;
#49322 = CARTESIAN_POINT ( 'NONE',  ( 5.550000001229032698, -2.886751345948125991, -5.000000000000000000 ) ) ;
#49323 = CARTESIAN_POINT ( 'NONE',  ( 4.771875000614516971, -6.054752690667223547, -1.112240025338166033E-15 ) ) ;
#49324 = CARTESIAN_POINT ( 'NONE',  ( 23.59687500061451715, -3.027376345333614438, 5.243569643749998122 ) ) ;
#49325 = CARTESIAN_POINT ( 'NONE',  ( 8.625000000000000000, 6.123233995736764310E-16, -4.999999999999998224 ) ) ;
#49326 = CARTESIAN_POINT ( 'NONE',  ( 19.30312500061451786, 4.541064518000418104, -2.621784821874998173 ) ) ;
#49327 = CARTESIAN_POINT ( 'NONE',  ( 23.74687500061451573, -3.027376345333610441, -5.243569643749999898 ) ) ;
#49328 = CARTESIAN_POINT ( 'NONE',  ( -3.756430356250000102, 19.27812499938548640, 30.00000000000000000 ) ) ;
#49329 = CARTESIAN_POINT ( 'NONE',  ( -3.999999999999999112, 11.07500000122903394, -32.30940107675850470 ) ) ;
#49330 = CARTESIAN_POINT ( 'NONE',  ( 29.74687500061451217, 6.054752690667223547, 3.707466751127219781E-16 ) ) ;
#49331 = CARTESIAN_POINT ( 'NONE',  ( 20.44687500061451502, -4.119189519843965641, -2.378215178125001383 ) ) ;
#49332 = CARTESIAN_POINT ( 'NONE',  ( 13.94062500061451892, 6.054752690667223547, 3.707466751127219781E-16 ) ) ;
#49333 = CARTESIAN_POINT ( 'NONE',  ( 12.19687500061451679, 6.054752690667223547, 3.707466751127219781E-16 ) ) ;
#49334 = ORIENTED_EDGE ( 'NONE', *, *, #24198, .F. ) ;
#49335 = CARTESIAN_POINT ( 'NONE',  ( 29.09999999999999787, 0.000000000000000000, 4.999999999999998224 ) ) ;
#49336 = CARTESIAN_POINT ( 'NONE',  ( 22.45312500061451644, 4.541064518000418104, -2.621784821874998173 ) ) ;
#49337 = CARTESIAN_POINT ( 'NONE',  ( 0.000000000000000000, 27.50000000000000000, 30.00000000000000000 ) ) ;
#49338 = CARTESIAN_POINT ( 'NONE',  ( 28.68750000122903288, 4.330127018922191873, 2.499999999999999556 ) ) ;
#49339 = CARTESIAN_POINT ( 'NONE',  ( 13.64999999999999858, 4.330127018922192761, -2.499999999999997780 ) ) ;
#49340 = CARTESIAN_POINT ( 'NONE',  ( 23.40000000122903145, -2.886751345948129988, 4.999999999999997335 ) ) ;
#49341 = CARTESIAN_POINT ( 'NONE',  ( 18.66562500061451146, -6.054752690667223547, -1.112240025338166033E-15 ) ) ;
#49342 = ORIENTED_EDGE ( 'NONE', *, *, #29976, .T. ) ;
#49343 = CARTESIAN_POINT ( 'NONE',  ( 21.56250000000000000, -5.773502691896255534, -1.060575238724906372E-15 ) ) ;
#49344 = CARTESIAN_POINT ( 'NONE',  ( 22.88437500061451857, 6.421520780324663323E-16, -5.243569643749999010 ) ) ;
#49345 = EDGE_CURVE ( 'NONE', #40707, #5936, #45874, .T. ) ;
#49346 = ORIENTED_EDGE ( 'NONE', *, *, #61190, .T. ) ;
#49347 = CARTESIAN_POINT ( 'NONE',  ( 20.06250000000000000, 2.886751345948126879, 4.999999999999998224 ) ) ;
#49348 = CARTESIAN_POINT ( 'NONE',  ( 9.890625000614516438, 6.054752690667223547, 3.707466751127219781E-16 ) ) ;
#49349 = CARTESIAN_POINT ( 'NONE',  ( 3.215625000614518836, 3.027376345333611329, 5.243569643749999010 ) ) ;
#49350 = CARTESIAN_POINT ( 'NONE',  ( 14.93437500061451573, -2.746126346562646425, 4.756430356249996549 ) ) ;
#49351 = CARTESIAN_POINT ( 'NONE',  ( 26.76562500061451644, -6.054752690667223547, -1.112240025338166033E-15 ) ) ;
#49352 = CARTESIAN_POINT ( 'NONE',  ( 17.66249999999999787, 2.886751345948129099, -4.999999999999998224 ) ) ;
#49353 = CARTESIAN_POINT ( 'NONE',  ( 25.34999999999999787, 4.330127018922192761, -2.499999999999997780 ) ) ;
#49354 = CARTESIAN_POINT ( 'NONE',  ( 3.531447089546592366, -3.539662852346280975, -3.745757099853723293 ) ) ;
#49355 = CARTESIAN_POINT ( 'NONE',  ( 5.671875000614519102, -6.054752690667223547, -1.112240025338166033E-15 ) ) ;
#49356 = CARTESIAN_POINT ( 'NONE',  ( 16.84687500061451715, -3.027376345333614438, 5.243569643749998122 ) ) ;
#49357 = CARTESIAN_POINT ( 'NONE',  ( 29.18437500061451573, 6.421520780324663323E-16, -5.243569643749999010 ) ) ;
#49358 = ORIENTED_EDGE ( 'NONE', *, *, #16519, .T. ) ;
#49359 = CARTESIAN_POINT ( 'NONE',  ( 25.71562500061451573, 3.027376345333611329, 5.243569643749999010 ) ) ;
#49360 = CARTESIAN_POINT ( 'NONE',  ( 27.64687500061452141, -3.027376345333614438, 5.243569643749998122 ) ) ;
#49361 = CARTESIAN_POINT ( 'NONE',  ( -1.626862140677534273E-15, 15.03124999877096535, 34.00000000000000000 ) ) ;
#49362 = CARTESIAN_POINT ( 'NONE',  ( 12.82499999999999929, 4.330127018922191873, 2.499999999999999556 ) ) ;
#49363 = CARTESIAN_POINT ( 'NONE',  ( 11.20312500061451644, 4.541064518000418104, -2.621784821874998173 ) ) ;
#49364 = CARTESIAN_POINT ( 'NONE',  ( 3.808519521103546523, 3.239781818325435658, 3.901918515728798997 ) ) ;
#49365 = CARTESIAN_POINT ( 'NONE',  ( 16.98750000000000426, -2.886751345948074920, 5.000000000000092371 ) ) ;
#49366 = CARTESIAN_POINT ( 'NONE',  ( 28.04062500061451502, -3.027376345333614438, 5.243569643749998122 ) ) ;
#49367 = CARTESIAN_POINT ( 'NONE',  ( 16.68750000122903288, -4.330127018922194537, 2.499999999999995559 ) ) ;
#49368 = CARTESIAN_POINT ( 'NONE',  ( 3.853125000614517681, -4.541064518000417216, -2.621784821875001281 ) ) ;
#49369 = CARTESIAN_POINT ( 'NONE',  ( 15.27187500061451786, 2.746126346562645981, -4.756430356249997438 ) ) ;
#49370 = CARTESIAN_POINT ( 'NONE',  ( 5.428125000614517859, 4.541064518000418104, 2.621784821874999949 ) ) ;
#49371 = CARTESIAN_POINT ( 'NONE',  ( 22.54687500061451999, 6.054752690667223547, 3.707466751127219781E-16 ) ) ;
#49372 = CARTESIAN_POINT ( 'NONE',  ( 9.001249775931846008E-16, 18.17187500061451999, 34.90005215228797653 ) ) ;
#49373 = CARTESIAN_POINT ( 'NONE',  ( 20.52187500061451786, -6.054752690667223547, -1.112240025338166033E-15 ) ) ;
#49374 = CARTESIAN_POINT ( 'NONE',  ( 29.70937500061451431, 4.541064518000418104, -2.621784821874998173 ) ) ;
#49375 = CARTESIAN_POINT ( 'NONE',  ( -4.243569643749999898, 18.95937500061451431, 30.00000000000000000 ) ) ;
#49376 = CARTESIAN_POINT ( 'NONE',  ( 12.47812500061451502, 6.421520780324663323E-16, -5.243569643749999010 ) ) ;
#49377 = CARTESIAN_POINT ( 'NONE',  ( 3.975000001229033852, 2.886751345948126879, 4.999999999999999112 ) ) ;
#49378 = CARTESIAN_POINT ( 'NONE',  ( 7.621875000614519280, 3.027376345333613106, -5.243569643749998122 ) ) ;
#49379 = CARTESIAN_POINT ( 'NONE',  ( 12.44999999999999929, 0.000000000000000000, 4.999999999999998224 ) ) ;
#49380 = CARTESIAN_POINT ( 'NONE',  ( 10.97812500061451679, -4.541064518000419881, 2.621784821874995952 ) ) ;
#49381 = CARTESIAN_POINT ( 'NONE',  ( 13.80937500061451750, -4.541064518000417216, -2.621784821875001281 ) ) ;
#49382 = CARTESIAN_POINT ( 'NONE',  ( 22.50000000122903288, -2.886751345948129988, 4.999999999999997335 ) ) ;
#49383 = CARTESIAN_POINT ( 'NONE',  ( 9.046875000614518214, 6.054752690667223547, 3.707466751127219781E-16 ) ) ;
#49384 = CARTESIAN_POINT ( 'NONE',  ( 10.37812500061451715, 4.541064518000418104, 2.621784821874999949 ) ) ;
#49385 = CARTESIAN_POINT ( 'NONE',  ( 24.88125000122903074, 6.123233995736764310E-16, -4.999999999999998224 ) ) ;
#49386 = CARTESIAN_POINT ( 'NONE',  ( 22.02187500061452141, 3.027376345333613106, -5.243569643749998122 ) ) ;
#49387 = CARTESIAN_POINT ( 'NONE',  ( 26.75625000122903430, 4.330127018922192761, -2.499999999999997780 ) ) ;
#49388 = CARTESIAN_POINT ( 'NONE',  ( -3.999828644916960663, 3.000228472979582506, 30.14345285717328693 ) ) ;
#49389 = CARTESIAN_POINT ( 'NONE',  ( 2.915625000614516793, -6.054752690667223547, -1.112240025338166033E-15 ) ) ;
#49390 = CARTESIAN_POINT ( 'NONE',  ( 2.121784821874999061, 11.15937500061451715, -33.67503911421598417 ) ) ;
#49391 = CARTESIAN_POINT ( 'NONE',  ( 14.40000000122903323, -2.886751345948129988, 4.999999999999997335 ) ) ;
#49392 = CARTESIAN_POINT ( 'NONE',  ( -2.121784821874996840, 14.92812500061451608, -26.32496088578401583 ) ) ;
#49393 = CARTESIAN_POINT ( 'NONE',  ( 16.46250000122903501, 4.330127018922192761, -2.499999999999997780 ) ) ;
#49394 = CARTESIAN_POINT ( 'NONE',  ( 9.778125000614517504, 6.421520780324663323E-16, -5.243569643749999010 ) ) ;
#49395 = ORIENTED_EDGE ( 'NONE', *, *, #45137, .T. ) ;
#49396 = CARTESIAN_POINT ( 'NONE',  ( 13.83749999999999858, -2.886751345948129988, 4.999999999999997335 ) ) ;
#49397 = CARTESIAN_POINT ( 'NONE',  ( 13.63125000122903252, 6.123233995736764310E-16, -4.999999999999998224 ) ) ;
#49398 = CARTESIAN_POINT ( 'NONE',  ( 23.01562500061451644, 3.027376345333611329, 5.243569643749999010 ) ) ;
#49399 = CARTESIAN_POINT ( 'NONE',  ( 10.73437500061451644, 6.421520780324663323E-16, -5.243569643749999010 ) ) ;
#49400 = LINE ( 'NONE', #70828, #65688 ) ;
#49401 = CARTESIAN_POINT ( 'NONE',  ( 9.600000001229034297, -2.886751345948125991, -5.000000000000000000 ) ) ;
#49402 = CARTESIAN_POINT ( 'NONE',  ( 19.31250000122903288, 0.000000000000000000, 4.999999999999998224 ) ) ;
#49403 = CARTESIAN_POINT ( 'NONE',  ( 15.02812500061451750, -4.541064518000419881, 2.621784821874995952 ) ) ;
#49404 = CARTESIAN_POINT ( 'NONE',  ( 18.92812500061451431, 4.541064518000418104, 2.621784821874999949 ) ) ;
#49405 = CARTESIAN_POINT ( 'NONE',  ( 25.87500000122903288, 2.886751345948129099, -4.999999999999998224 ) ) ;
#49406 = CARTESIAN_POINT ( 'NONE',  ( 26.88750000122903216, 4.330127018922191873, 2.499999999999999556 ) ) ;
#49407 = CARTESIAN_POINT ( 'NONE',  ( 26.21249999999999858, 2.886751345948129099, -4.999999999999998224 ) ) ;
#49408 = CARTESIAN_POINT ( 'NONE',  ( -1.878215178125001827, 13.84062499938548285, 33.25316411605952283 ) ) ;
#49409 = CARTESIAN_POINT ( 'NONE',  ( 26.93437500061451573, 6.421520780324663323E-16, -5.243569643749999010 ) ) ;
#49410 = DIRECTION ( 'NONE',  ( -0.000000000000000000, -1.000000000000000000, -0.000000000000000000 ) ) ;
#49411 = CARTESIAN_POINT ( 'NONE',  ( 12.93750000122903465, 4.330127018922191873, 2.499999999999999556 ) ) ;
#49412 = CARTESIAN_POINT ( 'NONE',  ( 3.300000000000000711, 4.330127018922192761, -2.499999999999997780 ) ) ;
#49413 = DIRECTION ( 'NONE',  ( 0.000000000000000000, -1.000000000000000000, 3.469446951953613006E-15 ) ) ;
#49414 = CARTESIAN_POINT ( 'NONE',  ( 3.984375000614517326, 6.421520780324663323E-16, -5.243569643749999010 ) ) ;
#49415 = CARTESIAN_POINT ( 'NONE',  ( 25.64062500061451644, 6.054752690667223547, 3.707466751127219781E-16 ) ) ;
#49416 = CARTESIAN_POINT ( 'NONE',  ( 22.42500000000000071, -4.330127018922194537, 2.499999999999995559 ) ) ;
#49417 = CARTESIAN_POINT ( 'NONE',  ( 11.03437500061451715, -4.541064518000419881, 2.621784821874995952 ) ) ;
#49418 = CARTESIAN_POINT ( 'NONE',  ( -4.000000000000000888, 16.81250000000000000, 32.30940107675850470 ) ) ;
#49419 = CARTESIAN_POINT ( 'NONE',  ( 29.72812500061451502, 4.541064518000418104, 2.621784821874999949 ) ) ;
#49420 = CARTESIAN_POINT ( 'NONE',  ( 8.334375000614516082, -4.541064518000419881, 2.621784821874995952 ) ) ;
#49421 = CARTESIAN_POINT ( 'NONE',  ( 28.58437500061451786, -4.541064518000419881, 2.621784821874995952 ) ) ;
#49422 = CARTESIAN_POINT ( 'NONE',  ( 4.243569643749999898, 11.92812500061459247, 30.00000000000000000 ) ) ;
#49423 = CARTESIAN_POINT ( 'NONE',  ( 21.11249999999999716, -5.773502691896255534, -1.060575238724906372E-15 ) ) ;
#49424 = EDGE_LOOP ( 'NONE', ( #3665, #56779, #38577, #30554 ) ) ;
#49425 = CARTESIAN_POINT ( 'NONE',  ( 20.70000000122903216, -2.886751345948096681, 5.000000000000054179 ) ) ;
#49426 = CARTESIAN_POINT ( 'NONE',  ( 4.425000000000001599, -4.330127018922194537, 2.499999999999995559 ) ) ;
#49427 = EDGE_CURVE ( 'NONE', #63177, #31702, #36387, .T. ) ;
#49428 = ORIENTED_EDGE ( 'NONE', *, *, #57151, .F. ) ;
#49429 = CARTESIAN_POINT ( 'NONE',  ( 17.84062500061451573, -3.027376345333610441, -5.243569643749999898 ) ) ;
#49430 = CARTESIAN_POINT ( 'NONE',  ( 11.42812500061451608, -4.541064518000419881, 2.621784821874995952 ) ) ;
#49431 = CARTESIAN_POINT ( 'NONE',  ( 21.42187500061451644, 5.824947211148865298E-16, -4.756430356249998326 ) ) ;
#49432 = CARTESIAN_POINT ( 'NONE',  ( 7.434375000614519280, -4.541064518000419881, 2.621784821874995952 ) ) ;
#49433 = CARTESIAN_POINT ( 'NONE',  ( 20.96250000122903145, 4.330127018922192761, -2.499999999999997780 ) ) ;
#49434 = CARTESIAN_POINT ( 'NONE',  ( 24.00000000122903288, -2.886751345948092684, -5.000000000000057732 ) ) ;
#49435 = CARTESIAN_POINT ( 'NONE',  ( 6.234375000614519102, 6.421520780324663323E-16, -5.243569643749999010 ) ) ;
#49436 = CARTESIAN_POINT ( 'NONE',  ( 14.33437500061451786, 6.421520780324663323E-16, -5.243569643749999010 ) ) ;
#49437 = CARTESIAN_POINT ( 'NONE',  ( 24.42187500061451999, 3.027376345333611329, 5.243569643749999010 ) ) ;
#49438 = DIRECTION ( 'NONE',  ( -0.000000000000000000, -1.000000000000000000, -0.000000000000000000 ) ) ;
#49439 = ORIENTED_EDGE ( 'NONE', *, *, #64274, .F. ) ;
#49440 = CARTESIAN_POINT ( 'NONE',  ( 12.41249999999999964, 2.886751345948126879, 4.999999999999999112 ) ) ;
#49441 = CARTESIAN_POINT ( 'NONE',  ( 17.89687500061451431, -3.027376345333610441, -5.243569643749999898 ) ) ;
#49442 = CARTESIAN_POINT ( 'NONE',  ( 9.384375000614518569, 6.421520780324663323E-16, -5.243569643749999010 ) ) ;
#49443 = CARTESIAN_POINT ( 'NONE',  ( 3.756430356250000546, 14.47812499938548747, 27.83122392262697886 ) ) ;
#49444 = CARTESIAN_POINT ( 'NONE',  ( 20.06250000000000000, 2.886751345948126879, 4.999999999999999112 ) ) ;
#49445 = CARTESIAN_POINT ( 'NONE',  ( -2.000000000000001776, 17.75000000000000355, 33.46410161513775705 ) ) ;
#49446 = CARTESIAN_POINT ( 'NONE',  ( 29.84999999999999787, 4.330127018922192761, -2.499999999999997780 ) ) ;
#49447 = CARTESIAN_POINT ( 'NONE',  ( 23.55937500061451573, 0.000000000000000000, 4.756430356249998326 ) ) ;
#49448 = CARTESIAN_POINT ( 'NONE',  ( 11.69062500061451360, 6.054752690667223547, 3.707466751127219781E-16 ) ) ;
#49449 = CARTESIAN_POINT ( 'NONE',  ( 28.28437500061451715, 6.421520780324663323E-16, -5.243569643749999010 ) ) ;
#49450 = DIRECTION ( 'NONE',  ( -1.000000000000000000, -0.000000000000000000, -0.000000000000000000 ) ) ;
#49451 = CARTESIAN_POINT ( 'NONE',  ( 28.54687500061451644, -3.027376345333614438, 5.243569643749998122 ) ) ;
#49452 = CARTESIAN_POINT ( 'NONE',  ( 11.28749999999999787, -2.886751345948125991, -5.000000000000000000 ) ) ;
#49453 = CARTESIAN_POINT ( 'NONE',  ( -3.999999999999999556, 17.82500000122903572, 27.69059892324149530 ) ) ;
#49454 = CARTESIAN_POINT ( 'NONE',  ( 12.18750000122903465, -4.330127018922194537, 2.499999999999995559 ) ) ;
#49455 = CARTESIAN_POINT ( 'NONE',  ( 21.87187500061451573, -6.054752690667223547, -1.112240025338166033E-15 ) ) ;
#49456 = CARTESIAN_POINT ( 'NONE',  ( 17.40937500061451715, -4.541064518000417216, -2.621784821875001281 ) ) ;
#49457 = CARTESIAN_POINT ( 'NONE',  ( 1.071796769724497445, 16.82990381179670081, 26.00000000000000355 ) ) ;
#49458 = VERTEX_POINT ( 'NONE', #58650 ) ;
#49459 = CARTESIAN_POINT ( 'NONE',  ( 17.05312500061451786, 4.541064518000418104, -2.621784821874998173 ) ) ;
#49460 = CARTESIAN_POINT ( 'NONE',  ( 28.16250000122903074, 4.330127018922192761, -2.499999999999997780 ) ) ;
#49461 = CARTESIAN_POINT ( 'NONE',  ( 14.82187500061451679, 3.027376345333613106, -5.243569643749998122 ) ) ;
#49462 = CARTESIAN_POINT ( 'NONE',  ( 2.840625000614518392, -3.027376345333614438, 5.243569643749998122 ) ) ;
#49463 = CARTESIAN_POINT ( 'NONE',  ( 18.66562500061451146, -6.054752690667223547, -1.112240025338166033E-15 ) ) ;
#49464 = DIRECTION ( 'NONE',  ( -1.000000000000000000, -0.000000000000000000, -0.000000000000000000 ) ) ;
#49465 = CARTESIAN_POINT ( 'NONE',  ( 28.47187500061451715, 3.027376345333611329, 5.243569643749999010 ) ) ;
#49466 = CARTESIAN_POINT ( 'NONE',  ( 9.001249775931846008E-16, 13.61562500061451786, 34.90005215228797653 ) ) ;
#49467 = CARTESIAN_POINT ( 'NONE',  ( 16.54687500061451644, -3.027376345333610441, -5.243569643749999898 ) ) ;
#49468 = CARTESIAN_POINT ( 'NONE',  ( 14.70000000122903394, 5.773502691896255534, 3.535250795749688894E-16 ) ) ;
#49469 = CARTESIAN_POINT ( 'NONE',  ( 10.35937500061451644, 4.119189519843966529, -2.378215178124998275 ) ) ;
#49470 = CARTESIAN_POINT ( 'NONE',  ( -2.121784821874996840, 19.03437500061451715, -26.32496088578401583 ) ) ;
#49471 =( BOUNDED_CURVE ( )  B_SPLINE_CURVE ( 2, ( #9211, #42827, #3678, #59434, #29645, #31378, #49111, #71640, #1951 ),
 .UNSPECIFIED., .F., .F. ) 
 B_SPLINE_CURVE_WITH_KNOTS ( ( 3, 2, 2, 2, 3 ),
 ( 0.05434782608695652717, 0.05797101449275362389, 0.06521739130434782428, 0.07246376811594203160, 0.07608695652173913526 ),
 .UNSPECIFIED. ) 
 CURVE ( )  GEOMETRIC_REPRESENTATION_ITEM ( )  RATIONAL_B_SPLINE_CURVE ( ( 0.9330127018922194093, 0.9330127018922194093, 1.000000000000000000, 0.8660254037844387076, 1.000000000000000000, 0.8660254037844387076, 1.000000000000000000, 0.9330127018922191873, 0.9330127018922192983 ) ) 
 REPRESENTATION_ITEM ( '' )  );
#49472 = CARTESIAN_POINT ( 'NONE',  ( 19.77187500061451786, 3.027376345333613106, -5.243569643749998122 ) ) ;
#49473 = CARTESIAN_POINT ( 'NONE',  ( 22.23750000122903003, 6.123233995736764310E-16, -4.999999999999998224 ) ) ;
#49474 = CARTESIAN_POINT ( 'NONE',  ( 16.35937500061451644, 0.000000000000000000, 5.243569643749999010 ) ) ;
#49475 = CARTESIAN_POINT ( 'NONE',  ( 12.02812500061451573, 6.421520780324663323E-16, -5.243569643749999010 ) ) ;
#49476 = CARTESIAN_POINT ( 'NONE',  ( -4.243569643749999898, 14.42187500061451644, 27.54997392385601529 ) ) ;
#49477 = CARTESIAN_POINT ( 'NONE',  ( 17.54062500061451502, 6.054752690667223547, 3.707466751127219781E-16 ) ) ;
#49478 = ORIENTED_EDGE ( 'NONE', *, *, #39698, .F. ) ;
#49479 = ORIENTED_EDGE ( 'NONE', *, *, #34377, .T. ) ;
#49480 = CARTESIAN_POINT ( 'NONE',  ( 23.25000000000000000, 0.000000000000000000, 4.999999999999998224 ) ) ;
#49481 = CARTESIAN_POINT ( 'NONE',  ( 2.121784821875001281, 18.65937500061451715, -26.32496088578401938 ) ) ;
#49482 = DIRECTION ( 'NONE',  ( -1.000000000000000000, 0.000000000000000000, 0.000000000000000000 ) ) ;
#49483 = CARTESIAN_POINT ( 'NONE',  ( 24.66562500061451502, 3.027376345333613106, -5.243569643749998122 ) ) ;
#49484 = CARTESIAN_POINT ( 'NONE',  ( 5.015625000614518214, 3.027376345333611329, 5.243569643749999010 ) ) ;
#49485 = CARTESIAN_POINT ( 'NONE',  ( 18.37500000122903288, 2.886751345948126879, 4.999999999999999112 ) ) ;
#49486 = CARTESIAN_POINT ( 'NONE',  ( 22.71562500061451573, -6.054752690667223547, -1.112240025338166033E-15 ) ) ;
#49487 = CARTESIAN_POINT ( 'NONE',  ( 22.46250000000000213, -5.773502691896255534, -1.060575238724906372E-15 ) ) ;
#49488 = CARTESIAN_POINT ( 'NONE',  ( 25.19062500061451715, 6.054752690667223547, 3.707466751127219781E-16 ) ) ;
#49489 = CARTESIAN_POINT ( 'NONE',  ( 5.915625000614515905, 3.027376345333611329, 5.243569643749999010 ) ) ;
#49490 = ORIENTED_EDGE ( 'NONE', *, *, #71191, .T. ) ;
#49491 = ADVANCED_FACE ( 'NONE', ( #42044 ), #7689, .T. ) ;
#49492 = CARTESIAN_POINT ( 'NONE',  ( 22.90312500061451573, 4.541064518000418104, -2.621784821874998173 ) ) ;
#49493 = CARTESIAN_POINT ( 'NONE',  ( 65.00000000000000000, -6.363961030678871644, 4.863961030678981778 ) ) ;
#49494 = EDGE_CURVE ( 'NONE', #16672, #27542, #8057, .T. ) ;
#49495 = CARTESIAN_POINT ( 'NONE',  ( 10.92187500061451644, 2.746126346562643317, 4.756430356249998326 ) ) ;
#49496 = CARTESIAN_POINT ( 'NONE',  ( 65.00000000000000000, 1.494782592887768269, 8.874999999999982236 ) ) ;
#49497 = CARTESIAN_POINT ( 'NONE',  ( -2.000000000000000000, 13.73750000122903359, -33.46410161513775705 ) ) ;
#49498 = CARTESIAN_POINT ( 'NONE',  ( -3.999999999999999112, 13.70000000000000107, -30.00000000000000000 ) ) ;
#49499 = CARTESIAN_POINT ( 'NONE',  ( 11.13750000000000284, -2.886751345948129988, 4.999999999999997335 ) ) ;
#49500 = EDGE_CURVE ( 'NONE', #39358, #72520, #59016, .T. ) ;
#49501 = CARTESIAN_POINT ( 'NONE',  ( 11.55937500061451928, -4.541064518000417216, -2.621784821875001281 ) ) ;
#49502 = CARTESIAN_POINT ( 'NONE',  ( 7.312500001229033764, -4.330127018922190985, -2.500000000000001332 ) ) ;
#49503 = CARTESIAN_POINT ( 'NONE',  ( 13.88437500061451679, 6.421520780324663323E-16, -5.243569643749999010 ) ) ;
#49504 = CARTESIAN_POINT ( 'NONE',  ( 7.096875000614517148, -3.027376345333610441, -5.243569643749999898 ) ) ;
#49505 = CARTESIAN_POINT ( 'NONE',  ( 2.121784821874999061, 10.20312500061451821, -33.67503911421598417 ) ) ;
#49506 = LINE ( 'NONE', #4080, #20576 ) ;
#49507 = EDGE_CURVE ( 'NONE', #18523, #54370, #41139, .T. ) ;
#49508 = CARTESIAN_POINT ( 'NONE',  ( 11.63437500061451857, 6.421520780324663323E-16, -5.243569643749999010 ) ) ;
#49509 = CARTESIAN_POINT ( 'NONE',  ( 13.31250000000000178, 2.886751345948126879, 4.999999999999998224 ) ) ;
#49510 = CARTESIAN_POINT ( 'NONE',  ( 20.87812500061451715, -4.541064518000419881, 2.621784821874995952 ) ) ;
#49511 =( BOUNDED_CURVE ( )  B_SPLINE_CURVE ( 2, ( #45414, #67592, #29507, #6249, #5530, #28067, #39511 ),
 .UNSPECIFIED., .F., .F. ) 
 B_SPLINE_CURVE_WITH_KNOTS ( ( 3, 2, 2, 3 ),
 ( 0.7500000000000000000, 0.7533333333333332993, 0.7566666666666667096, 0.7600000000000000089 ),
 .UNSPECIFIED. ) 
 CURVE ( )  GEOMETRIC_REPRESENTATION_ITEM ( )  RATIONAL_B_SPLINE_CURVE ( ( 1.000000000000000000, 0.8660254037844387076, 1.000000000000000000, 0.8660254037844387076, 1.000000000000000000, 0.8660254037844387076, 1.000000000000000000 ) ) 
 REPRESENTATION_ITEM ( '' )  );
#49512 = CARTESIAN_POINT ( 'NONE',  ( 2.121784821875001281, 18.60312500061459673, 33.67503911421598417 ) ) ;
#49513 = CARTESIAN_POINT ( 'NONE',  ( 22.50937500061451857, 4.541064518000418104, -2.621784821874998173 ) ) ;
#49514 = CARTESIAN_POINT ( 'NONE',  ( 1.999999999999998668, 19.40000000000000213, 26.53589838486224650 ) ) ;
#49515 =( BOUNDED_CURVE ( )  B_SPLINE_CURVE ( 2, ( #50434, #44893, #62589, #34508, #57036, #18222, #23423 ),
 .UNSPECIFIED., .F., .F. ) 
 B_SPLINE_CURVE_WITH_KNOTS ( ( 3, 2, 2, 3 ),
 ( 0.4200000000000000955, 0.4233333333333334503, 0.4266666666666668051, 0.4300000000000001044 ),
 .UNSPECIFIED. ) 
 CURVE ( )  GEOMETRIC_REPRESENTATION_ITEM ( )  RATIONAL_B_SPLINE_CURVE ( ( 0.9999999999999955591, 0.8660254037844431485, 1.000000000000000000, 0.8660254037844387076, 1.000000000000000000, 0.8660254037844342667, 1.000000000000004441 ) ) 
 REPRESENTATION_ITEM ( '' )  );
#49516 = CARTESIAN_POINT ( 'NONE',  ( 29.40000000122903145, -2.886751345948125991, -5.000000000000000000 ) ) ;
#49517 = CARTESIAN_POINT ( 'NONE',  ( 20.52187500061451786, 5.824947211148865298E-16, -4.756430356249998326 ) ) ;
#49518 = CARTESIAN_POINT ( 'NONE',  ( 25.45312500061451644, -4.541064518000417216, -2.621784821875001281 ) ) ;
#49519 = CARTESIAN_POINT ( 'NONE',  ( 18.51562500061451289, 3.027376345333611329, 5.243569643749999010 ) ) ;
#49520 = CARTESIAN_POINT ( 'NONE',  ( 15.31875000122903252, -5.773502691896255534, -1.060575238724906372E-15 ) ) ;
#49521 = CARTESIAN_POINT ( 'NONE',  ( 14.14687500061451786, -3.027376345333614438, 5.243569643749998122 ) ) ;
#49522 = CARTESIAN_POINT ( 'NONE',  ( 7.359375000614516438, -5.492252693125287522, -1.008910452111647106E-15 ) ) ;
#49523 = CARTESIAN_POINT ( 'NONE',  ( 27.48750000122903359, -4.330127018922194537, 2.499999999999995559 ) ) ;
#49524 = CARTESIAN_POINT ( 'NONE',  ( 6.534375000614517148, -4.541064518000419881, 2.621784821874995952 ) ) ;
#49525 = CARTESIAN_POINT ( 'NONE',  ( 14.59687500061452070, -3.027376345333614438, 5.243569643749998122 ) ) ;
#49526 = CARTESIAN_POINT ( 'NONE',  ( 16.05000000000000071, 0.000000000000000000, 4.999999999999998224 ) ) ;
#49527 = CARTESIAN_POINT ( 'NONE',  ( 8.137500001229033941, -4.330127018922194537, 2.499999999999995559 ) ) ;
#49528 = CARTESIAN_POINT ( 'NONE',  ( 4.200000001229033053, -2.886751345948125991, -5.000000000000000000 ) ) ;
#49529 = CARTESIAN_POINT ( 'NONE',  ( 25.39687500061451431, -3.027376345333614438, 5.243569643749998122 ) ) ;
#49530 = CARTESIAN_POINT ( 'NONE',  ( 17.55937500061451573, 4.541064518000418104, -2.621784821874998173 ) ) ;
#49531 = CARTESIAN_POINT ( 'NONE',  ( -7.967954043666661671E-16, 15.34062499938548463, 34.33755215474603517 ) ) ;
#49532 = CARTESIAN_POINT ( 'NONE',  ( 29.28749999999999787, -2.886751345948125991, -5.000000000000000000 ) ) ;
#49533 = CARTESIAN_POINT ( 'NONE',  ( 6.637500000000001066, -2.886751345948129988, 4.999999999999997335 ) ) ;
#49534 = CARTESIAN_POINT ( 'NONE',  ( 28.54687500061451644, -2.746126346562646425, 4.756430356249996549 ) ) ;
#49535 = CARTESIAN_POINT ( 'NONE',  ( 20.65312500061451573, 4.541064518000418104, -2.621784821874998173 ) ) ;
#49536 = CARTESIAN_POINT ( 'NONE',  ( 8.662499999999999645, 2.886751345948129099, -4.999999999999998224 ) ) ;
#49537 = EDGE_CURVE ( 'NONE', #72457, #67390, #54585, .T. ) ;
#49538 = CARTESIAN_POINT ( 'NONE',  ( 4.828125000614518214, 6.421520780324663323E-16, -5.243569643749999010 ) ) ;
#49539 = CARTESIAN_POINT ( 'NONE',  ( 20.21250000000000213, -5.773502691896255534, -1.060575238724906372E-15 ) ) ;
#49540 =( BOUNDED_CURVE ( )  B_SPLINE_CURVE ( 1, ( #47790, #13420 ),
 .UNSPECIFIED., .F., .F. ) 
 B_SPLINE_CURVE_WITH_KNOTS ( ( 2, 2 ),
 ( 0.000000000000000000, 1.000000000000000000 ),
 .UNSPECIFIED. ) 
 CURVE ( )  GEOMETRIC_REPRESENTATION_ITEM ( )  RATIONAL_B_SPLINE_CURVE ( ( 0.9401540804572410259, 0.9401540804572410259 ) ) 
 REPRESENTATION_ITEM ( '' )  );
#49541 = CARTESIAN_POINT ( 'NONE',  ( 1.592000809091587073E-14, 17.18750000000000355, 26.00000000000000000 ) ) ;
#49542 = CARTESIAN_POINT ( 'NONE',  ( 24.11250000122903359, 4.330127018922192761, -2.499999999999997780 ) ) ;
#49543 = CARTESIAN_POINT ( 'NONE',  ( 5.948646956027291210, 8.038298999021536773, 30.80897801260831770 ) ) ;
#49544 = CARTESIAN_POINT ( 'NONE',  ( 3.112500000000000711, -5.773502691896255534, -1.060575238724906372E-15 ) ) ;
#49545 = ORIENTED_EDGE ( 'NONE', *, *, #11547, .F. ) ;
#49546 = CARTESIAN_POINT ( 'NONE',  ( 16.49062500061451786, -3.027376345333610441, -5.243569643749999898 ) ) ;
#49547 = CARTESIAN_POINT ( 'NONE',  ( 24.47812500061451502, -4.541064518000419881, 2.621784821874995952 ) ) ;
#49548 = CARTESIAN_POINT ( 'NONE',  ( 25.80937500061451928, 0.000000000000000000, 5.243569643749999010 ) ) ;
#49549 = CARTESIAN_POINT ( 'NONE',  ( 6.037500000000001421, 5.773502691896255534, 3.535250795749688894E-16 ) ) ;
#49550 = CARTESIAN_POINT ( 'NONE',  ( 10.34062500061451750, 6.054752690667223547, 3.707466751127219781E-16 ) ) ;
#49551 = CARTESIAN_POINT ( 'NONE',  ( 26.31562500061451715, -6.054752690667223547, -1.112240025338166033E-15 ) ) ;
#49552 = CARTESIAN_POINT ( 'NONE',  ( 14.85937500061451644, 4.541064518000418104, -2.621784821874998173 ) ) ;
#49553 = CARTESIAN_POINT ( 'NONE',  ( 18.68437500061451928, -4.541064518000419881, 2.621784821874995952 ) ) ;
#49554 = CARTESIAN_POINT ( 'NONE',  ( 30.00000000000000000, 6.123233995736764310E-16, -4.999999999999998224 ) ) ;
#49555 = CARTESIAN_POINT ( 'NONE',  ( 2.121784821875001281, 10.10937500061451821, 33.67503911421598417 ) ) ;
#49556 = CARTESIAN_POINT ( 'NONE',  ( 23.62500000122902932, 2.886751345948129099, -4.999999999999998224 ) ) ;
#49557 = CARTESIAN_POINT ( 'NONE',  ( 16.69687500061451502, 5.492252693125287522, 3.363034840372157021E-16 ) ) ;
#49558 = CARTESIAN_POINT ( 'NONE',  ( 12.40312500061451573, -4.541064518000417216, -2.621784821875001281 ) ) ;
#49559 = CARTESIAN_POINT ( 'NONE',  ( 6.796875000614516438, 6.054752690667223547, 3.707466751127219781E-16 ) ) ;
#49560 = CARTESIAN_POINT ( 'NONE',  ( 7.884375000614517681, -4.541064518000419881, 2.621784821874995952 ) ) ;
#49561 = ORIENTED_EDGE ( 'NONE', *, *, #54635, .T. ) ;
#49562 = CARTESIAN_POINT ( 'NONE',  ( 27.00937500061451857, 4.541064518000418104, -2.621784821874998173 ) ) ;
#49563 = CARTESIAN_POINT ( 'NONE',  ( 19.34062500061451573, 6.054752690667223547, 3.707466751127219781E-16 ) ) ;
#49564 = CARTESIAN_POINT ( 'NONE',  ( 29.66250000122903074, 0.000000000000000000, 4.999999999999998224 ) ) ;
#49565 = CARTESIAN_POINT ( 'NONE',  ( 3.046875000614519990, -3.027376345333610441, -5.243569643749999898 ) ) ;
#49566 = CARTESIAN_POINT ( 'NONE',  ( 24.23437500061451644, 6.421520780324663323E-16, -5.243569643749999010 ) ) ;
#49567 = CARTESIAN_POINT ( 'NONE',  ( 18.92812500061451431, 4.541064518000418104, 2.621784821874999949 ) ) ;
#49568 = CARTESIAN_POINT ( 'NONE',  ( 8.484601909799253346E-16, 11.11250000000000071, 34.61880215351700230 ) ) ;
#49569 = CARTESIAN_POINT ( 'NONE',  ( 24.77812500061451217, 4.541064518000418104, 2.621784821874999949 ) ) ;
#49570 = CARTESIAN_POINT ( 'NONE',  ( 5.437500001229035540, -4.330127018922194537, 2.499999999999995559 ) ) ;
#49571 = ORIENTED_EDGE ( 'NONE', *, *, #35816, .F. ) ;
#49572 = LINE ( 'NONE', #15933, #41604 ) ;
#49573 = CARTESIAN_POINT ( 'NONE',  ( 1.999999999999998668, 15.80000000000000071, -33.46410161513775705 ) ) ;
#49574 = CARTESIAN_POINT ( 'NONE',  ( -3.756430356249999214, 16.09062499938548285, 27.83122392262697531 ) ) ;
#49575 = CARTESIAN_POINT ( 'NONE',  ( 5.709375000614517859, -4.541064518000417216, -2.621784821875001281 ) ) ;
#49576 = FACE_OUTER_BOUND ( 'NONE', #27464, .T. ) ;
#49577 = CARTESIAN_POINT ( 'NONE',  ( 12.89062500061451821, -3.027376345333610441, -5.243569643749999898 ) ) ;
#49578 = CARTESIAN_POINT ( 'NONE',  ( 5.671875000614519102, -6.054752690667223547, -1.112240025338166033E-15 ) ) ;
#49579 = CARTESIAN_POINT ( 'NONE',  ( 25.38750000122903216, 6.123233995736764310E-16, -4.999999999999998224 ) ) ;
#49580 = CARTESIAN_POINT ( 'NONE',  ( 15.15937500061451715, -4.541064518000417216, -2.621784821875001281 ) ) ;
#49581 = CARTESIAN_POINT ( 'NONE',  ( 29.72812500061451502, 4.541064518000418104, 2.621784821874999949 ) ) ;
#49582 = CARTESIAN_POINT ( 'NONE',  ( 14.62500000122903288, 2.886751345948129099, -4.999999999999997335 ) ) ;
#49583 = CARTESIAN_POINT ( 'NONE',  ( 16.07812500061451289, 6.421520780324663323E-16, -5.243569643749999010 ) ) ;
#49584 = ORIENTED_EDGE ( 'NONE', *, *, #64257, .F. ) ;
#49585 = CARTESIAN_POINT ( 'NONE',  ( 10.45312500061451644, 0.000000000000000000, 5.243569643749999010 ) ) ;
#49586 = CARTESIAN_POINT ( 'NONE',  ( 8.690625000614515372, -3.027376345333614438, 5.243569643749998122 ) ) ;
#49587 = CARTESIAN_POINT ( 'NONE',  ( 18.42187500061451644, 2.746126346562645981, -4.756430356249997438 ) ) ;
#49588 = CARTESIAN_POINT ( 'NONE',  ( 8.512499999999999289, -5.773502691896255534, -1.060575238724906372E-15 ) ) ;
#49589 = CARTESIAN_POINT ( 'NONE',  ( 3.787500001229033408, 6.123233995736764310E-16, -4.999999999999998224 ) ) ;
#49590 = CARTESIAN_POINT ( 'NONE',  ( 18.45000000000000284, -4.330127018922190985, -2.500000000000001332 ) ) ;
#49591 = EDGE_CURVE ( 'NONE', #21163, #70620, #2944, .T. ) ;
#49592 = CARTESIAN_POINT ( 'NONE',  ( 18.75937500061451857, -4.541064518000417216, -2.621784821875001281 ) ) ;
#49593 = CARTESIAN_POINT ( 'NONE',  ( 13.35000000122903430, 5.773502691896255534, 3.535250795749688894E-16 ) ) ;
#49594 = CARTESIAN_POINT ( 'NONE',  ( 20.96250000000000213, 2.886751345948126879, 4.999999999999999112 ) ) ;
#49595 = CARTESIAN_POINT ( 'NONE',  ( -4.243569643749999898, 16.16562500061451857, -32.45002607614398471 ) ) ;
#49596 = CARTESIAN_POINT ( 'NONE',  ( 20.66250000000000142, -5.773502691896255534, -1.060575238724906372E-15 ) ) ;
#49597 = CARTESIAN_POINT ( 'NONE',  ( 24.20625000122903359, 0.000000000000000000, 4.999999999999998224 ) ) ;
#49598 = CARTESIAN_POINT ( 'NONE',  ( 29.69062500061451715, 6.054752690667223547, 3.707466751127219781E-16 ) ) ;
#49599 = CARTESIAN_POINT ( 'NONE',  ( 0.000000000000000000, 0.000000000000000000, -50.00000000000000000 ) ) ;
#49600 = CARTESIAN_POINT ( 'NONE',  ( 1.071796769724497445, 16.26740381056766438, -33.99999999999998579 ) ) ;
#49601 = CARTESIAN_POINT ( 'NONE',  ( 12.90937500061451537, -4.541064518000417216, -2.621784821875001281 ) ) ;
#49602 = CARTESIAN_POINT ( 'NONE',  ( 26.32499999999999929, 4.330127018922191873, 2.499999999999999556 ) ) ;
#49603 = CARTESIAN_POINT ( 'NONE',  ( 9.965625000614517504, 3.027376345333611329, 5.243569643749999010 ) ) ;
#49604 = CARTESIAN_POINT ( 'NONE',  ( 27.08437500061451431, -2.746126346562646425, 4.756430356249996549 ) ) ;
#49605 = CARTESIAN_POINT ( 'NONE',  ( 22.39687500061451075, -3.027376345333610441, -5.243569643749999898 ) ) ;
#49606 = CARTESIAN_POINT ( 'NONE',  ( 14.18437500061451573, -2.746126346562641984, -4.756430356249999214 ) ) ;
#49607 = CARTESIAN_POINT ( 'NONE',  ( 7.303125000614516082, 0.000000000000000000, 5.243569643749999010 ) ) ;
#49608 = CARTESIAN_POINT ( 'NONE',  ( 13.13437500061451857, 4.541064518000418104, 2.621784821874999949 ) ) ;
#49609 = ORIENTED_EDGE ( 'NONE', *, *, #6300, .T. ) ;
#49610 = CARTESIAN_POINT ( 'NONE',  ( 24.60937500061451644, -4.541064518000417216, -2.621784821875001281 ) ) ;
#49611 = CARTESIAN_POINT ( 'NONE',  ( 1.091159441285790788, 4.887044806266472641, -26.14197170220922573 ) ) ;
#49612 = DIRECTION ( 'NONE',  ( 0.000000000000000000, 0.000000000000000000, 1.000000000000000000 ) ) ;
#49614 = ADVANCED_FACE ( 'NONE', ( #71945 ), #3988, .F. ) ;
#49613 = CARTESIAN_POINT ( 'NONE',  ( 5.287500000000000533, -2.886751345948129988, 4.999999999999997335 ) ) ;
#49615 = CARTESIAN_POINT ( 'NONE',  ( 16.12500000122903288, 2.886751345948126879, 4.999999999999999112 ) ) ;
#49616 = CARTESIAN_POINT ( 'NONE',  ( -1.071796769724492115, 19.96115380933863293, 34.00000000000000000 ) ) ;
#49617 = CARTESIAN_POINT ( 'NONE',  ( -3.999999999999997335, 19.13750000000000284, -27.69059892324149530 ) ) ;
#49618 = EDGE_LOOP ( 'NONE', ( #69966, #20839, #123, #33011 ) ) ;
#49619 = CARTESIAN_POINT ( 'NONE',  ( 12.30000000000000249, 4.330127018922192761, -2.499999999999997780 ) ) ;
#49620 = CARTESIAN_POINT ( 'NONE',  ( 17.51249999999999929, -5.773502691896255534, -1.060575238724906372E-15 ) ) ;
#49621 = CARTESIAN_POINT ( 'NONE',  ( 13.20000000122903394, -2.886751345948125991, -5.000000000000000000 ) ) ;
#49622 = CARTESIAN_POINT ( 'NONE',  ( 10.60312500061451679, -4.541064518000417216, -2.621784821875001281 ) ) ;
#49623 = ORIENTED_EDGE ( 'NONE', *, *, #10028, .F. ) ;
#49624 = CARTESIAN_POINT ( 'NONE',  ( 10.05000000000000071, 4.330127018922192761, -2.499999999999997780 ) ) ;
#49625 = CARTESIAN_POINT ( 'NONE',  ( -1.999999999999997113, 17.03750000122903430, -26.53589838486224295 ) ) ;
#49626 = CARTESIAN_POINT ( 'NONE',  ( 2.121784821875001281, 15.05937500061451928, -26.32496088578401938 ) ) ;
#49627 = CARTESIAN_POINT ( 'NONE',  ( 3.440625000614518036, -3.027376345333610441, -5.243569643749999898 ) ) ;
#49628 = CARTESIAN_POINT ( 'NONE',  ( 3.756430356250000546, 15.82812499938548356, 27.83122392262697886 ) ) ;
#49629 = CARTESIAN_POINT ( 'NONE',  ( 10.49999999999999822, 4.330127018922192761, -2.499999999999997780 ) ) ;
#49630 = CARTESIAN_POINT ( 'NONE',  ( 3.059722729795383067, 3.954539355547352919, 3.095961626413553436 ) ) ;
#49631 = VERTEX_POINT ( 'NONE', #20954 ) ;
#49632 = CARTESIAN_POINT ( 'NONE',  ( 25.11562500061451431, 3.027376345333613106, -5.243569643749998122 ) ) ;
#49633 = CARTESIAN_POINT ( 'NONE',  ( 25.55625000122903501, 0.000000000000000000, 4.999999999999998224 ) ) ;
#49634 = CARTESIAN_POINT ( 'NONE',  ( 1.878215178125000495, 19.91562499938548569, 26.74683588394047007 ) ) ;
#49635 = CARTESIAN_POINT ( 'NONE',  ( 21.38437500061451502, -4.541064518000419881, 2.621784821874995952 ) ) ;
#49636 = CARTESIAN_POINT ( 'NONE',  ( 18.51562500061451289, 3.027376345333611329, 5.243569643749999010 ) ) ;
#49637 = ADVANCED_FACE ( 'NONE', ( #37589, #38318 ), #43508, .F. ) ;
#49638 = CARTESIAN_POINT ( 'NONE',  ( 9.001249775931846008E-16, 11.81562500061459531, -25.09994784771203058 ) ) ;
#49639 = CARTESIAN_POINT ( 'NONE',  ( 6.853125000614516793, 0.000000000000000000, 5.243569643749999010 ) ) ;
#49640 = CARTESIAN_POINT ( 'NONE',  ( 3.515625000614516882, 3.027376345333613106, -5.243569643749998122 ) ) ;
#49641 = CARTESIAN_POINT ( 'NONE',  ( 24.12187500061451573, -5.492252693125287522, -1.008910452111647106E-15 ) ) ;
#49642 = CARTESIAN_POINT ( 'NONE',  ( 20.76562500061451999, 3.027376345333611329, 5.243569643749999010 ) ) ;
#49643 = CARTESIAN_POINT ( 'NONE',  ( 8.484375000614518214, 5.824947211148865298E-16, -4.756430356249998326 ) ) ;
#49644 = CARTESIAN_POINT ( 'NONE',  ( -3.756430356250000102, 17.81562499938548427, 30.00000000000000000 ) ) ;
#49645 = CARTESIAN_POINT ( 'NONE',  ( 15.27187500061451786, 3.027376345333613106, -5.243569643749998122 ) ) ;
#49646 = CARTESIAN_POINT ( 'NONE',  ( 14.59687500061452070, -3.027376345333614438, 5.243569643749998122 ) ) ;
#49647 = CARTESIAN_POINT ( 'NONE',  ( 23.22187500061451715, -6.054752690667223547, -1.112240025338166033E-15 ) ) ;
#49648 = ORIENTED_EDGE ( 'NONE', *, *, #46542, .T. ) ;
#49649 = CARTESIAN_POINT ( 'NONE',  ( -4.243569643749999898, 12.65937500061451715, 30.00000000000000000 ) ) ;
#49650 = CARTESIAN_POINT ( 'NONE',  ( 19.87500000000000000, 6.123233995736764310E-16, -4.999999999999998224 ) ) ;
#49651 = CARTESIAN_POINT ( 'NONE',  ( 25.79062500061451502, -3.027376345333614438, 5.243569643749998122 ) ) ;
#49652 = CARTESIAN_POINT ( 'NONE',  ( 25.67812500061451431, 4.541064518000418104, 2.621784821874999949 ) ) ;
#49653 = CARTESIAN_POINT ( 'NONE',  ( 1.626862140677534273E-15, 13.36250000000000071, -26.00000000000000355 ) ) ;
#49654 = CARTESIAN_POINT ( 'NONE',  ( -3.999999999999999556, 18.61250000000000426, 27.69059892324149530 ) ) ;
#49655 = CARTESIAN_POINT ( 'NONE',  ( 5.221875000614519813, -6.054752690667223547, -1.112240025338166033E-15 ) ) ;
#49656 = APPLICATION_PROTOCOL_DEFINITION ( 'draft international standard', 'automotive_design', 1998, #29032 ) ;
#49657 = CARTESIAN_POINT ( 'NONE',  ( 13.68750000122903288, 6.123233995736764310E-16, -4.999999999999998224 ) ) ;
#49658 = CARTESIAN_POINT ( 'NONE',  ( 9.862500001229033586, 0.000000000000000000, 4.999999999999998224 ) ) ;
#49659 = CARTESIAN_POINT ( 'NONE',  ( 3.290625000614516793, -3.027376345333614438, 5.243569643749998122 ) ) ;
#49660 = CARTESIAN_POINT ( 'NONE',  ( -3.999999999999999556, 16.68124999877096570, 27.69059892324149175 ) ) ;
#49661 = CARTESIAN_POINT ( 'NONE',  ( 18.58125000122903003, 6.123233995736764310E-16, -4.999999999999998224 ) ) ;
#49662 = CARTESIAN_POINT ( 'NONE',  ( 11.22187500061451892, 3.027376345333613106, -5.243569643749998122 ) ) ;
#49663 = CARTESIAN_POINT ( 'NONE',  ( 1.071796769724490561, 12.85759618943233917, 34.00000000000000000 ) ) ;
#49664 = ORIENTED_EDGE ( 'NONE', *, *, #55830, .T. ) ;
#49665 = CARTESIAN_POINT ( 'NONE',  ( 19.82812500061451644, 4.541064518000418104, 2.621784821874999949 ) ) ;
#49666 = CARTESIAN_POINT ( 'NONE',  ( 12.27187500061451786, 3.027376345333611329, 5.243569643749999010 ) ) ;
#49667 = CARTESIAN_POINT ( 'NONE',  ( 4.678125000614516971, -4.541064518000419881, 2.621784821874995952 ) ) ;
#49668 = CARTESIAN_POINT ( 'NONE',  ( 23.14687500061451786, -3.027376345333614438, 5.243569643749998122 ) ) ;
#49669 = EDGE_CURVE ( 'NONE', #33507, #19228, #14866, .T. ) ;
#49670 = CARTESIAN_POINT ( 'NONE',  ( 6.290625000614517681, 6.054752690667223547, 3.707466751127219781E-16 ) ) ;
#49671 = CARTESIAN_POINT ( 'NONE',  ( 6.712500001229034119, 0.000000000000000000, 4.999999999999998224 ) ) ;
#49672 = CARTESIAN_POINT ( 'NONE',  ( 8.737500001229033586, 6.123233995736764310E-16, -4.999999999999998224 ) ) ;
#49673 = CARTESIAN_POINT ( 'NONE',  ( 21.59062500061451928, 6.054752690667223547, 3.707466751127219781E-16 ) ) ;
#49674 = CARTESIAN_POINT ( 'NONE',  ( 2.000000000000001332, 17.11250000122903359, -26.53589838486224650 ) ) ;
#49675 = CARTESIAN_POINT ( 'NONE',  ( 7.687500001229033764, -4.330127018922194537, 2.499999999999995559 ) ) ;
#49676 = CARTESIAN_POINT ( 'NONE',  ( 16.60312500061451857, 4.541064518000418104, -2.621784821874998173 ) ) ;
#49677 = CARTESIAN_POINT ( 'NONE',  ( 14.42812500061451786, 4.541064518000418104, 2.621784821874999949 ) ) ;
#49678 = CARTESIAN_POINT ( 'NONE',  ( 25.54687500061451644, -2.746126346562642428, -4.756430356249999214 ) ) ;
#49679 = CARTESIAN_POINT ( 'NONE',  ( 14.58750000000000036, 5.773502691896255534, 3.535250795749688894E-16 ) ) ;
#49680 = CARTESIAN_POINT ( 'NONE',  ( 11.02500000122903501, 2.886751345948129099, -4.999999999999998224 ) ) ;
#49681 = CARTESIAN_POINT ( 'NONE',  ( 7.528125000614515727, 6.421520780324663323E-16, -5.243569643749999010 ) ) ;
#49682 = CARTESIAN_POINT ( 'NONE',  ( 10.49062500061451431, -3.027376345333614438, 5.243569643749998122 ) ) ;
#49683 = CARTESIAN_POINT ( 'NONE',  ( 19.91250000122903074, -4.330127018922190985, -2.500000000000001332 ) ) ;
#49684 = CARTESIAN_POINT ( 'NONE',  ( -2.121784821874996840, 12.73437500061451821, -26.32496088578401583 ) ) ;
#49685 = CARTESIAN_POINT ( 'NONE',  ( 20.37187500061451573, 3.027376345333611329, 5.243569643749999010 ) ) ;
#49686 = CYLINDRICAL_SURFACE ( 'NONE', #53637, 4.999999999999998224 ) ;
#49687 = CARTESIAN_POINT ( 'NONE',  ( 6.075000001229034829, 2.886751345948129099, -4.999999999999998224 ) ) ;
#49688 = CARTESIAN_POINT ( 'NONE',  ( 3.684375000614518836, 4.541064518000418104, 2.621784821874999949 ) ) ;
#49689 = CARTESIAN_POINT ( 'NONE',  ( 21.00937500061451857, -4.541064518000417216, -2.621784821875001281 ) ) ;
#49690 = AXIS2_PLACEMENT_3D ( 'NONE', #70501, #8436, #19507 ) ;
#49691 = LINE ( 'NONE', #39335, #61014 ) ;
#49692 = CARTESIAN_POINT ( 'NONE',  ( 17.20312500061451644, 0.000000000000000000, 5.243569643749999010 ) ) ;
#49693 = CARTESIAN_POINT ( 'NONE',  ( 10.74375000122903323, -2.886751345948129988, 4.999999999999997335 ) ) ;
#49694 = CARTESIAN_POINT ( 'NONE',  ( -1.071796769724502107, 20.67634618820330417, 26.00000000000000711 ) ) ;
#49695 = CARTESIAN_POINT ( 'NONE',  ( 14.00625000122903252, -4.330127018922190985, -2.500000000000001332 ) ) ;
#49696 = CARTESIAN_POINT ( 'NONE',  ( 27.53437500061451360, 4.541064518000418104, 2.621784821874999949 ) ) ;
#49697 = CARTESIAN_POINT ( 'NONE',  ( 20.03437500061451715, -2.746126346562641984, -4.756430356249999214 ) ) ;
#49698 = CARTESIAN_POINT ( 'NONE',  ( 14.50312500061451537, 0.000000000000000000, 5.243569643749999010 ) ) ;
#49699 = CARTESIAN_POINT ( 'NONE',  ( 13.02187500061451608, 3.027376345333613106, -5.243569643749998122 ) ) ;
#49700 = ORIENTED_EDGE ( 'NONE', *, *, #59478, .T. ) ;
#49701 = CYLINDRICAL_SURFACE ( 'NONE', #35978, 4.999999999999998224 ) ;
#49702 = CARTESIAN_POINT ( 'NONE',  ( 22.56562500061451715, 3.027376345333611329, 5.243569643749999010 ) ) ;
#49703 = CARTESIAN_POINT ( 'NONE',  ( 17.66250000122903430, -4.330127018922190985, -2.500000000000001332 ) ) ;
#49704 = DIRECTION ( 'NONE',  ( 0.000000000000000000, 0.7071067811865535679, 0.7071067811865414665 ) ) ;
#49705 = CARTESIAN_POINT ( 'NONE',  ( 12.15000000000000036, -4.330127018922190985, -2.500000000000001332 ) ) ;
#49706 = CARTESIAN_POINT ( 'NONE',  ( 23.02500000122903145, -5.773502691896255534, -1.060575238724906372E-15 ) ) ;
#49707 = CARTESIAN_POINT ( 'NONE',  ( 17.61562500061451786, 3.027376345333611329, 5.243569643749999010 ) ) ;
#49708 = ORIENTED_EDGE ( 'NONE', *, *, #52890, .T. ) ;
#49709 = CARTESIAN_POINT ( 'NONE',  ( 19.46249999999999858, 2.886751345948129099, -4.999999999999998224 ) ) ;
#49710 = CARTESIAN_POINT ( 'NONE',  ( 20.67187500061451289, 3.027376345333613106, -5.243569643749998122 ) ) ;
#49711 = ORIENTED_EDGE ( 'NONE', *, *, #58454, .F. ) ;
#49712 = CARTESIAN_POINT ( 'NONE',  ( 1.999999999999997335, 19.17500000000000071, 33.46410161513775705 ) ) ;
#49713 = CARTESIAN_POINT ( 'NONE',  ( 10.52812500061451750, -4.541064518000419881, 2.621784821874995952 ) ) ;
#49714 = CARTESIAN_POINT ( 'NONE',  ( 3.325761423091350366, 3.733538664146505592, 3.492540098399592452 ) ) ;
#49715 = CARTESIAN_POINT ( 'NONE',  ( 13.09687500061451715, 0.000000000000000000, 4.756430356249998326 ) ) ;
#49716 = CARTESIAN_POINT ( 'NONE',  ( 16.01249999999999929, 2.886751345948126879, 4.999999999999999112 ) ) ;
#49717 = CARTESIAN_POINT ( 'NONE',  ( 24.67500000000000071, -4.330127018922194537, 2.499999999999995559 ) ) ;
#49718 = CARTESIAN_POINT ( 'NONE',  ( -2.121784821874999949, 18.82812500061451644, 26.32496088578401938 ) ) ;
#49719 = CARTESIAN_POINT ( 'NONE',  ( 3.496875000614518836, -3.027376345333610441, -5.243569643749999898 ) ) ;
#49720 = CARTESIAN_POINT ( 'NONE',  ( 27.57187500061451857, 3.027376345333611329, 5.243569643749999010 ) ) ;
#49721 = ORIENTED_EDGE ( 'NONE', *, *, #8883, .F. ) ;
#49722 = MECHANICAL_DESIGN_GEOMETRIC_PRESENTATION_REPRESENTATION (  '', ( #37895 ), #62674 ) ;
#49723 = CARTESIAN_POINT ( 'NONE',  ( 26.24062500061451431, -3.027376345333614438, 5.243569643749998122 ) ) ;
#49724 = CARTESIAN_POINT ( 'NONE',  ( 28.39687500061452141, 6.054752690667223547, 3.707466751127219781E-16 ) ) ;
#49725 = CARTESIAN_POINT ( 'NONE',  ( 3.159375000614518036, 4.541064518000418104, -2.621784821874998173 ) ) ;
#49726 = CARTESIAN_POINT ( 'NONE',  ( 14.28750000000000142, -2.886751345948129988, 4.999999999999997335 ) ) ;
#49727 = CARTESIAN_POINT ( 'NONE',  ( 11.16562500061451679, 3.027376345333613106, -5.243569643749998122 ) ) ;
#49728 = CARTESIAN_POINT ( 'NONE',  ( 6.075000000000000178, 4.330127018922191873, 2.499999999999999556 ) ) ;
#49729 = FACE_OUTER_BOUND ( 'NONE', #71048, .T. ) ;
#49730 = CARTESIAN_POINT ( 'NONE',  ( 27.77812500061451573, 6.421520780324663323E-16, -5.243569643749999010 ) ) ;
#49731 = CARTESIAN_POINT ( 'NONE',  ( 16.83750000122903145, 6.123233995736764310E-16, -4.999999999999998224 ) ) ;
#49732 = CARTESIAN_POINT ( 'NONE',  ( 29.03437500061451360, -2.746126346562641984, -4.756430356249999214 ) ) ;
#49733 = CARTESIAN_POINT ( 'NONE',  ( 15.57187500061451679, -5.492252693125287522, -1.008910452111647106E-15 ) ) ;
#49734 = CARTESIAN_POINT ( 'NONE',  ( 5.540625000614515905, -3.027376345333614438, 5.243569643749998122 ) ) ;
#49735 = CARTESIAN_POINT ( 'NONE',  ( 22.20937500061451431, 0.000000000000000000, 5.243569643749999010 ) ) ;
#49736 = CARTESIAN_POINT ( 'NONE',  ( -4.243569643749999898, 14.45937500061451964, 30.00000000000000000 ) ) ;
#49737 = CARTESIAN_POINT ( 'NONE',  ( 21.42187500061451644, -6.054752690667223547, -1.112240025338166033E-15 ) ) ;
#49738 = CARTESIAN_POINT ( 'NONE',  ( 3.000000000000002665, 0.000000000000000000, 4.999999999999998224 ) ) ;
#49739 = CARTESIAN_POINT ( 'NONE',  ( 4.243569643749999010, 19.67187500061451644, 27.54997392385601174 ) ) ;
#49740 = CARTESIAN_POINT ( 'NONE',  ( 10.67812500061451608, 6.421520780324663323E-16, -5.243569643749999010 ) ) ;
#49741 = CYLINDRICAL_SURFACE ( 'NONE', #43119, 4.999999999999998224 ) ;
#49742 = CARTESIAN_POINT ( 'NONE',  ( 7.921875000614517326, -6.054752690667223547, -1.112240025338166033E-15 ) ) ;
#49743 = CARTESIAN_POINT ( 'NONE',  ( 13.04999999999999893, -4.330127018922190985, -2.500000000000001332 ) ) ;
#49744 = CARTESIAN_POINT ( 'NONE',  ( 7.715625000614515727, 3.027376345333611329, 5.243569643749999010 ) ) ;
#49745 = CARTESIAN_POINT ( 'NONE',  ( 11.82187500061451679, 3.027376345333611329, 5.243569643749999010 ) ) ;
#49746 = CARTESIAN_POINT ( 'NONE',  ( 25.53750000000000142, -2.886751345948116221, 5.000000000000021316 ) ) ;
#49747 = CARTESIAN_POINT ( 'NONE',  ( 21.48750000122903003, 4.330127018922191873, 2.499999999999999556 ) ) ;
#49748 = CARTESIAN_POINT ( 'NONE',  ( 7.509375000614517681, -4.541064518000417216, -2.621784821875001281 ) ) ;
#49749 = CARTESIAN_POINT ( 'NONE',  ( 9.440625000614517148, 6.054752690667223547, 3.707466751127219781E-16 ) ) ;
#49750 = CARTESIAN_POINT ( 'NONE',  ( 25.93125000122903145, 4.330127018922191873, 2.499999999999999556 ) ) ;
#49751 = CARTESIAN_POINT ( 'NONE',  ( 19.92187500061451644, 3.027376345333611329, 5.243569643749999010 ) ) ;
#49752 = CARTESIAN_POINT ( 'NONE',  ( 65.00000000000000000, 6.363961030678916053, -6.363961030678939146 ) ) ;
#49753 = CARTESIAN_POINT ( 'NONE',  ( 21.71250000122903501, -4.330127018922190985, -2.500000000000001332 ) ) ;
#49754 = CARTESIAN_POINT ( 'NONE',  ( 29.40937500061451715, 0.000000000000000000, 5.243569643749999010 ) ) ;
#49755 = COLOUR_RGB ( '',0.8941176470588234615, 0.8941176470588234615, 0.8941176470588234615 ) ;
#49756 = CARTESIAN_POINT ( 'NONE',  ( 2.121784821875001281, 12.80937500061451928, -26.32496088578401938 ) ) ;
#49757 = CARTESIAN_POINT ( 'NONE',  ( 14.62500000122903288, 2.886751345948129099, -4.999999999999998224 ) ) ;
#49758 =( BOUNDED_CURVE ( )  B_SPLINE_CURVE ( 2, ( #52005, #56804, #51644, #23915, #41289, #46101, #46463 ),
 .UNSPECIFIED., .F., .F. ) 
 B_SPLINE_CURVE_WITH_KNOTS ( ( 3, 2, 2, 3 ),
 ( 0.3800000000000000044, 0.3833333333333333592, 0.3866666666666666585, 0.3900000000000000133 ),
 .UNSPECIFIED. ) 
 CURVE ( )  GEOMETRIC_REPRESENTATION_ITEM ( )  RATIONAL_B_SPLINE_CURVE ( ( 1.000000000000000000, 0.8660254037844387076, 1.000000000000000000, 0.8660254037844387076, 1.000000000000000000, 0.8660254037844387076, 1.000000000000000000 ) ) 
 REPRESENTATION_ITEM ( '' )  );
#49759 = CARTESIAN_POINT ( 'NONE',  ( -2.121784821874999949, 15.67812500061451608, -33.67503911421598417 ) ) ;
#49760 = CARTESIAN_POINT ( 'NONE',  ( 16.12500000122903288, 2.886751345948126879, 4.999999999999999112 ) ) ;
#49761 = CARTESIAN_POINT ( 'NONE',  ( 9.553125000614517859, 0.000000000000000000, 5.243569643749999010 ) ) ;
#49762 = ORIENTED_EDGE ( 'NONE', *, *, #32239, .T. ) ;
#49763 = CARTESIAN_POINT ( 'NONE',  ( 13.01249999999999929, -5.773502691896255534, -1.060575238724906372E-15 ) ) ;
#49764 = CARTESIAN_POINT ( 'NONE',  ( -3.999999999999997335, 13.73749999999999893, 32.30940107675850470 ) ) ;
#49765 = CARTESIAN_POINT ( 'NONE',  ( 22.34062500061451573, -3.027376345333610441, -5.243569643749999898 ) ) ;
#49766 = CARTESIAN_POINT ( 'NONE',  ( 7.809375000614519280, 0.000000000000000000, 5.243569643749999010 ) ) ;
#49767 = CARTESIAN_POINT ( 'NONE',  ( 34.99999999999999289, -2.499999999999999556, 3.499999999999999556 ) ) ;
#49768 = CARTESIAN_POINT ( 'NONE',  ( 10.05000000122903181, -2.886751345948125991, -5.000000000000000000 ) ) ;
#49769 = CARTESIAN_POINT ( 'NONE',  ( 17.55000000122903359, -2.886751345948129988, 4.999999999999997335 ) ) ;
#49770 = CARTESIAN_POINT ( 'NONE',  ( 15.47812500061451679, -4.541064518000419881, 2.621784821874995952 ) ) ;
#49771 = CARTESIAN_POINT ( 'NONE',  ( 18.96562500061451573, 3.027376345333611329, 5.243569643749999010 ) ) ;
#49772 = CARTESIAN_POINT ( 'NONE',  ( 25.95000000122903216, 5.773502691896255534, 3.535250795749688894E-16 ) ) ;
#49773 = ADVANCED_FACE ( 'NONE', ( #9881 ), #38698, .F. ) ;
#49774 = CARTESIAN_POINT ( 'NONE',  ( 27.82500000122903572, 2.886751345948126879, 4.999999999999999112 ) ) ;
#49775 = CARTESIAN_POINT ( 'NONE',  ( 22.31250000000000000, 2.886751345948126879, 4.999999999999999112 ) ) ;
#49776 = CARTESIAN_POINT ( 'NONE',  ( -3.756430356249999214, 13.27812499938548463, 27.83122392262697531 ) ) ;
#49777 = CARTESIAN_POINT ( 'NONE',  ( 24.79687500061451999, 6.054752690667223547, 3.707466751127219781E-16 ) ) ;
#49778 = DIRECTION ( 'NONE',  ( 1.000000000000000000, -0.000000000000000000, -0.000000000000000000 ) ) ;
#49779 = CARTESIAN_POINT ( 'NONE',  ( 13.65000000122903323, -2.886751345948125991, -5.000000000000000000 ) ) ;
#49780 = CARTESIAN_POINT ( 'NONE',  ( 27.12187500061451573, 3.027376345333611329, 5.243569643749999010 ) ) ;
#49781 = CARTESIAN_POINT ( 'NONE',  ( -2.000000000000001776, 18.59374999877096357, 33.46410161513775705 ) ) ;
#49782 = CARTESIAN_POINT ( 'NONE',  ( 5.971875000614516260, 3.027376345333611329, 5.243569643749999010 ) ) ;
#49783 = CARTESIAN_POINT ( 'NONE',  ( 25.45312500061451644, -4.541064518000417216, -2.621784821875001281 ) ) ;
#49784 = CARTESIAN_POINT ( 'NONE',  ( -7.967954043666661671E-16, 13.99062499938548498, 34.33755215474603517 ) ) ;
#49785 = CARTESIAN_POINT ( 'NONE',  ( 10.39687500061451786, 6.054752690667223547, 3.707466751127219781E-16 ) ) ;
#49786 = CARTESIAN_POINT ( 'NONE',  ( -2.000000000000001776, 16.85000000000000142, 33.46410161513775705 ) ) ;
#49787 = CARTESIAN_POINT ( 'NONE',  ( 3.309375000614518836, 0.000000000000000000, 5.243569643749999010 ) ) ;
#49788 = CARTESIAN_POINT ( 'NONE',  ( 9.946875000614516793, 6.054752690667223547, 3.707466751127219781E-16 ) ) ;
#49789 = CARTESIAN_POINT ( 'NONE',  ( 28.39687500061452141, 6.054752690667223547, 3.707466751127219781E-16 ) ) ;
#49790 = CARTESIAN_POINT ( 'NONE',  ( -4.243569643749999898, 13.46562500061459744, 27.54997392385601529 ) ) ;
#49791 = CARTESIAN_POINT ( 'NONE',  ( 19.57500000000000284, 4.330127018922191873, 2.499999999999999556 ) ) ;
#49792 = ORIENTED_EDGE ( 'NONE', *, *, #42731, .F. ) ;
#49793 = CARTESIAN_POINT ( 'NONE',  ( 29.55000000000000071, 0.000000000000000000, 4.999999999999998224 ) ) ;
#49794 = CARTESIAN_POINT ( 'NONE',  ( 3.187500000000002220, -2.886751345948125991, -5.000000000000000000 ) ) ;
#49795 = EDGE_LOOP ( 'NONE', ( #27494, #61637, #41558, #45757 ) ) ;
#49796 = VECTOR ( 'NONE', #34114, 1000.000000000000000 ) ;
#49797 = CARTESIAN_POINT ( 'NONE',  ( 17.16562500061451502, 3.027376345333611329, 5.243569643749999010 ) ) ;
#49798 = CARTESIAN_POINT ( 'NONE',  ( 8.240625000614516082, -3.027376345333614438, 5.243569643749998122 ) ) ;
#49799 = CARTESIAN_POINT ( 'NONE',  ( 21.27187500061451431, -4.119189519843968306, 2.378215178124996054 ) ) ;
#49800 = CARTESIAN_POINT ( 'NONE',  ( 6.796875000614516438, 6.054752690667223547, 3.707466751127219781E-16 ) ) ;
#49801 = CARTESIAN_POINT ( 'NONE',  ( 18.86250000122903359, 0.000000000000000000, 4.999999999999998224 ) ) ;
#49802 = CARTESIAN_POINT ( 'NONE',  ( -0.6945863667395647534, 9.663023495605401081, -33.93923213064925903 ) ) ;
#49803 = CARTESIAN_POINT ( 'NONE',  ( 7.621875000614519280, 3.027376345333613106, -5.243569643749998122 ) ) ;
#49804 = CARTESIAN_POINT ( 'NONE',  ( 12.42187500061451821, -6.054752690667223547, -1.112240025338166033E-15 ) ) ;
#49805 = CARTESIAN_POINT ( 'NONE',  ( 23.85937500061451644, 4.541064518000418104, -2.621784821874998173 ) ) ;
#49806 = CARTESIAN_POINT ( 'NONE',  ( -3.999999999999999112, 14.56250000000000000, -32.30940107675850470 ) ) ;
#49807 = VERTEX_POINT ( 'NONE', #3620 ) ;
#49808 = CARTESIAN_POINT ( 'NONE',  ( 10.80000000000000071, -4.330127018922190985, -2.500000000000001332 ) ) ;
#49809 = CARTESIAN_POINT ( 'NONE',  ( 17.37187500061451573, -6.054752690667223547, -1.112240025338166033E-15 ) ) ;
#49810 = CARTESIAN_POINT ( 'NONE',  ( 8.784375000614518925, -4.541064518000419881, 2.621784821874995952 ) ) ;
#49811 = CARTESIAN_POINT ( 'NONE',  ( 3.756430356249998770, 13.95312499938548179, 32.16877607737302469 ) ) ;
#49812 = CARTESIAN_POINT ( 'NONE',  ( 21.03750000000000142, -2.886751345948129988, 4.999999999999997335 ) ) ;
#49813 = CARTESIAN_POINT ( 'NONE',  ( 1.999999999999997335, 16.47500000000000142, 33.46410161513775705 ) ) ;
#49814 = CARTESIAN_POINT ( 'NONE',  ( 34.99999999999999289, 6.123233995736764310E-16, -4.999999999999998224 ) ) ;
#49815 = CARTESIAN_POINT ( 'NONE',  ( 21.45937500061451786, -4.119189519843965641, -2.378215178125001383 ) ) ;
#49816 = CARTESIAN_POINT ( 'NONE',  ( 13.07812500061451821, 4.541064518000418104, 2.621784821874999949 ) ) ;
#49817 = CARTESIAN_POINT ( 'NONE',  ( 29.10937500061451644, -4.541064518000417216, -2.621784821875001281 ) ) ;
#49818 = DIRECTION ( 'NONE',  ( -0.000000000000000000, -1.000000000000000000, -0.000000000000000000 ) ) ;
#49819 = CARTESIAN_POINT ( 'NONE',  ( 29.18437500061451573, 6.421520780324663323E-16, -5.243569643749999010 ) ) ;
#49820 = CARTESIAN_POINT ( 'NONE',  ( 9.975000000000001421, 6.123233995736764310E-16, -4.999999999999998224 ) ) ;
#49821 = CARTESIAN_POINT ( 'NONE',  ( -3.999999999999997335, 15.20000000122903572, 32.30940107675850470 ) ) ;
#49822 = CARTESIAN_POINT ( 'NONE',  ( 8.287500001229034297, 6.123233995736764310E-16, -4.999999999999998224 ) ) ;
#49823 = CARTESIAN_POINT ( 'NONE',  ( 21.15937500061451715, 4.541064518000418104, -2.621784821874998173 ) ) ;
#49824 = CARTESIAN_POINT ( 'NONE',  ( 13.80937500061451750, -4.541064518000417216, -2.621784821875001281 ) ) ;
#49825 = CARTESIAN_POINT ( 'NONE',  ( 45.00000000000000000, 6.123233995736764310E-16, -4.999999999999998224 ) ) ;
#49826 = ORIENTED_EDGE ( 'NONE', *, *, #48710, .F. ) ;
#49827 = CARTESIAN_POINT ( 'NONE',  ( 16.00312500061451715, -4.541064518000417216, -2.621784821875001281 ) ) ;
#49828 = CARTESIAN_POINT ( 'NONE',  ( 27.75000000122903288, 5.773502691896255534, 3.535250795749688894E-16 ) ) ;
#49829 = CARTESIAN_POINT ( 'NONE',  ( 16.39687500061451786, -3.027376345333614438, 5.243569643749998122 ) ) ;
#49830 = CARTESIAN_POINT ( 'NONE',  ( 5.959992197959416593, 8.030459126529553515, -30.80005261327864829 ) ) ;
#49831 = CARTESIAN_POINT ( 'NONE',  ( 16.97812500061451502, 6.421520780324663323E-16, -5.243569643749999010 ) ) ;
#49832 = CARTESIAN_POINT ( 'NONE',  ( 18.45000000000000284, -4.330127018922190985, -2.500000000000001332 ) ) ;
#49833 = CARTESIAN_POINT ( 'NONE',  ( 28.88437500061451502, 4.541064518000418104, 2.621784821874999949 ) ) ;
#49834 = CARTESIAN_POINT ( 'NONE',  ( -4.243569643749999898, 11.70312500061451644, 30.00000000000000000 ) ) ;
#49835 = CARTESIAN_POINT ( 'NONE',  ( 16.24687500061451573, 6.054752690667223547, 3.707466751127219781E-16 ) ) ;
#49836 = CARTESIAN_POINT ( 'NONE',  ( 14.55000000122903181, -2.886751345948125991, -5.000000000000000000 ) ) ;
#49837 = CARTESIAN_POINT ( 'NONE',  ( 10.73437500061451644, 5.824947211148865298E-16, -4.756430356249998326 ) ) ;
#49838 = CARTESIAN_POINT ( 'NONE',  ( -4.243569643749999898, 18.50937500061451857, -30.00000000000000000 ) ) ;
#49839 = CARTESIAN_POINT ( 'NONE',  ( 21.72187500061451715, 3.027376345333611329, 5.243569643749999010 ) ) ;
#49840 = CARTESIAN_POINT ( 'NONE',  ( 23.51250000122903216, -4.330127018922190985, -2.500000000000001332 ) ) ;
#49841 = CARTESIAN_POINT ( 'NONE',  ( 16.80937500061451573, 0.000000000000000000, 5.243569643749999010 ) ) ;
#49842 = CARTESIAN_POINT ( 'NONE',  ( 13.37812500061451715, 6.421520780324663323E-16, -5.243569643749999010 ) ) ;
#49843 = CARTESIAN_POINT ( 'NONE',  ( 4.243569643749999010, 12.47187500061451715, 27.54997392385601174 ) ) ;
#49844 = CARTESIAN_POINT ( 'NONE',  ( 18.02812500061451573, 4.541064518000418104, 2.621784821874999949 ) ) ;
#49845 = ORIENTED_EDGE ( 'NONE', *, *, #49856, .T. ) ;
#49846 = EDGE_LOOP ( 'NONE', ( #25199, #24354, #67434, #51511 ) ) ;
#49847 = CARTESIAN_POINT ( 'NONE',  ( 20.73750000000000071, -2.886751345948125991, -5.000000000000000000 ) ) ;
#49848 = CARTESIAN_POINT ( 'NONE',  ( 24.81562500061451715, 3.027376345333611329, 5.243569643749999010 ) ) ;
#49849 = CARTESIAN_POINT ( 'NONE',  ( 5.203125000614518214, -4.541064518000417216, -2.621784821875001281 ) ) ;
#49850 = CARTESIAN_POINT ( 'NONE',  ( 17.55000000122903359, -2.886751345948129988, 4.999999999999997335 ) ) ;
#49851 = CARTESIAN_POINT ( 'NONE',  ( 22.00312500061451360, 4.541064518000418104, -2.621784821874998173 ) ) ;
#49852 = CARTESIAN_POINT ( 'NONE',  ( 23.40000000000000213, -4.330127018922190985, -2.500000000000001332 ) ) ;
#49853 = CARTESIAN_POINT ( 'NONE',  ( 24.70312500061451644, 4.541064518000418104, -2.621784821874998173 ) ) ;
#49854 = CARTESIAN_POINT ( 'NONE',  ( 6.253125000614517148, 4.541064518000418104, -2.621784821874998173 ) ) ;
#49855 = VERTEX_POINT ( 'NONE', #26885 ) ;
#49856 = EDGE_CURVE ( 'NONE', #33629, #29982, #21321, .T. ) ;
#49857 = AXIS2_PLACEMENT_3D ( 'NONE', #53623, #26282, #15184 ) ;
#49858 = CARTESIAN_POINT ( 'NONE',  ( 29.36250000000000071, 2.886751345948129099, -4.999999999999998224 ) ) ;
#49859 = CARTESIAN_POINT ( 'NONE',  ( 3.665625000614517681, 3.027376345333611329, 5.243569643749999010 ) ) ;
#49860 = CARTESIAN_POINT ( 'NONE',  ( 12.30937500061451573, 0.000000000000000000, 4.756430356249998326 ) ) ;
#49861 = CARTESIAN_POINT ( 'NONE',  ( 45.00000000000000000, 0.000000000000000000, 4.999999999999998224 ) ) ;
#49862 = CARTESIAN_POINT ( 'NONE',  ( 2.000000000000001332, 12.61250000122903536, -26.53589838486224650 ) ) ;
#49863 = CARTESIAN_POINT ( 'NONE',  ( 4.243569643749999898, 19.14687500061451431, -27.54997392385601529 ) ) ;
#49864 = CARTESIAN_POINT ( 'NONE',  ( 11.21250000000000036, -5.773502691896255534, -1.060575238724906372E-15 ) ) ;
#49865 = CARTESIAN_POINT ( 'NONE',  ( 12.12187500061451573, 3.027376345333613106, -5.243569643749998122 ) ) ;
#49866 = CARTESIAN_POINT ( 'NONE',  ( 6.150000001229033231, 5.773502691896255534, 3.535250795749688894E-16 ) ) ;
#49867 = CARTESIAN_POINT ( 'NONE',  ( 13.32187500061451502, -6.054752690667223547, -1.112240025338166033E-15 ) ) ;
#49868 = CARTESIAN_POINT ( 'NONE',  ( 5.446875000614518569, 6.054752690667223547, 3.707466751127219781E-16 ) ) ;
#49869 = DIRECTION ( 'NONE',  ( 0.000000000000000000, 0.000000000000000000, -1.000000000000000000 ) ) ;
#49870 = CARTESIAN_POINT ( 'NONE',  ( 9.159375000614515372, 0.000000000000000000, 5.243569643749999010 ) ) ;
#49871 = CARTESIAN_POINT ( 'NONE',  ( 45.00000000000000000, -2.499999999999999556, 3.499999999999999556 ) ) ;
#49872 = CARTESIAN_POINT ( 'NONE',  ( 20.84062500061451573, -3.027376345333614438, 5.243569643749998122 ) ) ;
#49873 = FACE_OUTER_BOUND ( 'NONE', #54833, .T. ) ;
#49874 = DIRECTION ( 'NONE',  ( -1.000000000000000000, -0.000000000000000000, -0.000000000000000000 ) ) ;
#49875 = CARTESIAN_POINT ( 'NONE',  ( 23.93437500061451573, 4.541064518000418104, 2.621784821874999949 ) ) ;
#49876 = CARTESIAN_POINT ( 'NONE',  ( -1.999999999999997113, 13.88750000122903394, -26.53589838486224295 ) ) ;
#49877 = CARTESIAN_POINT ( 'NONE',  ( 28.16250000122903074, 4.330127018922192761, -2.499999999999997780 ) ) ;
#49878 = CARTESIAN_POINT ( 'NONE',  ( 18.90937500061451360, 2.746126346562643317, 4.756430356249998326 ) ) ;
#49879 = CARTESIAN_POINT ( 'NONE',  ( 25.04062500061451502, -3.027376345333610441, -5.243569643749999898 ) ) ;
#49880 = CARTESIAN_POINT ( 'NONE',  ( 15.25312500061451715, 4.541064518000418104, -2.621784821874998173 ) ) ;
#49881 = CARTESIAN_POINT ( 'NONE',  ( 13.81875000122903074, 2.886751345948126879, 4.999999999999999112 ) ) ;
#49882 = CARTESIAN_POINT ( 'NONE',  ( 13.58437500061451786, 4.541064518000418104, 2.621784821874999949 ) ) ;
#49883 = CARTESIAN_POINT ( 'NONE',  ( 16.80000000000000071, 4.330127018922192761, -2.499999999999997780 ) ) ;
#49884 = CARTESIAN_POINT ( 'NONE',  ( 24.63750000122903216, 4.330127018922191873, 2.499999999999999556 ) ) ;
#49885 = CARTESIAN_POINT ( 'NONE',  ( 3.684375000614518836, 4.541064518000418104, 2.621784821874999949 ) ) ;
#49886 = CARTESIAN_POINT ( 'NONE',  ( 14.14687500061451786, -3.027376345333614438, 5.243569643749998122 ) ) ;
#49887 = CARTESIAN_POINT ( 'NONE',  ( 16.23749999999999716, -2.886751345948193048, -4.999999999999883649 ) ) ;
#49888 = CARTESIAN_POINT ( 'NONE',  ( -3.999999999999999112, 11.41250000000000142, 27.69059892324149885 ) ) ;
#49889 = CARTESIAN_POINT ( 'NONE',  ( 2.887500001229035274, 6.123233995736764310E-16, -4.999999999999998224 ) ) ;
#49890 = CARTESIAN_POINT ( 'NONE',  ( 25.69687500061451502, 6.054752690667223547, 3.707466751127219781E-16 ) ) ;
#49891 = CARTESIAN_POINT ( 'NONE',  ( 16.24687500061451573, 6.054752690667223547, 3.707466751127219781E-16 ) ) ;
#49892 = CARTESIAN_POINT ( 'NONE',  ( 3.756430356250000546, 16.84062499938548285, 27.83122392262697886 ) ) ;
#49893 = CARTESIAN_POINT ( 'NONE',  ( 27.56250000000000000, 2.886751345948129099, -4.999999999999998224 ) ) ;
#49894 = CARTESIAN_POINT ( 'NONE',  ( 3.900000001229034563, 5.773502691896255534, 3.535250795749688894E-16 ) ) ;
#49895 = CARTESIAN_POINT ( 'NONE',  ( 6.150000000000003020, 0.000000000000000000, 4.999999999999998224 ) ) ;
#49896 = CARTESIAN_POINT ( 'NONE',  ( 7.771875000614516082, -4.119189519843968306, 2.378215178124996054 ) ) ;
#49897 = CARTESIAN_POINT ( 'NONE',  ( 20.24062500061451431, 6.054752690667223547, 3.707466751127219781E-16 ) ) ;
#49898 = CARTESIAN_POINT ( 'NONE',  ( 10.46249999999999858, 2.886751345948129099, -4.999999999999998224 ) ) ;
#49899 =( BOUNDED_CURVE ( )  B_SPLINE_CURVE ( 2, ( #70106, #40959, #46491, #57919, #64193, #58645, #18391 ),
 .UNSPECIFIED., .F., .F. ) 
 B_SPLINE_CURVE_WITH_KNOTS ( ( 3, 2, 2, 3 ),
 ( 0.4099999999999999201, 0.4133333333333333304, 0.4166666666666667407, 0.4200000000000000955 ),
 .UNSPECIFIED. ) 
 CURVE ( )  GEOMETRIC_REPRESENTATION_ITEM ( )  RATIONAL_B_SPLINE_CURVE ( ( 1.000000000000002220, 0.8660254037844364872, 1.000000000000000000, 0.8660254037844387076, 1.000000000000000000, 0.8660254037844342667, 1.000000000000004441 ) ) 
 REPRESENTATION_ITEM ( '' )  );
#49900 = CARTESIAN_POINT ( 'NONE',  ( 4.978125000614518569, 4.541064518000418104, 2.621784821874999949 ) ) ;
#49901 = CARTESIAN_POINT ( 'NONE',  ( 18.22499999999999787, 4.330127018922191873, 2.499999999999999556 ) ) ;
#49902 = CARTESIAN_POINT ( 'NONE',  ( 10.00000000000000000, 1.224646799147353256E-15, 50.00000000000000000 ) ) ;
#49903 = CARTESIAN_POINT ( 'NONE',  ( 21.78750000122903074, 6.123233995736764310E-16, -4.999999999999998224 ) ) ;
#49904 = CARTESIAN_POINT ( 'NONE',  ( -1.389181105737270716, 10.01354714573257532, -33.81675806816645036 ) ) ;
#49905 = CARTESIAN_POINT ( 'NONE',  ( 28.58437500061451786, -4.541064518000419881, 2.621784821874995952 ) ) ;
#49906 = ORIENTED_EDGE ( 'NONE', *, *, #43332, .F. ) ;
#49907 = CARTESIAN_POINT ( 'NONE',  ( 16.79062500061451857, -3.027376345333614438, 5.243569643749998122 ) ) ;
#49908 = CARTESIAN_POINT ( 'NONE',  ( 24.51562500061451289, -6.054752690667223547, -1.112240025338166033E-15 ) ) ;
#49909 = CARTESIAN_POINT ( 'NONE',  ( 22.95937500061451431, 4.541064518000418104, -2.621784821874998173 ) ) ;
#49910 = CARTESIAN_POINT ( 'NONE',  ( 6.187500000000002665, -2.886751345948129988, 4.999999999999997335 ) ) ;
#49911 = CARTESIAN_POINT ( 'NONE',  ( 8.390625000614518214, -3.027376345333610441, -5.243569643749999898 ) ) ;
#49912 = CARTESIAN_POINT ( 'NONE',  ( 23.72812500061451502, 6.421520780324663323E-16, -5.243569643749999010 ) ) ;
#49913 = CARTESIAN_POINT ( 'NONE',  ( 15.23437500061451644, 6.421520780324663323E-16, -5.243569643749999010 ) ) ;
#49914 = CARTESIAN_POINT ( 'NONE',  ( 18.23437500061451999, -4.541064518000419881, 2.621784821874995952 ) ) ;
#49915 = CARTESIAN_POINT ( 'NONE',  ( 17.73750000122903359, 6.123233995736764310E-16, -4.999999999999998224 ) ) ;
#49916 = CARTESIAN_POINT ( 'NONE',  ( -4.243569643749999898, 19.76562500061451644, 27.54997392385601529 ) ) ;
#49917 = CARTESIAN_POINT ( 'NONE',  ( 21.75000000122903288, -2.886751345948125991, -5.000000000000000000 ) ) ;
#49918 = CARTESIAN_POINT ( 'NONE',  ( 16.50937500061451502, -4.119189519843965641, -2.378215178125001383 ) ) ;
#49919 = CARTESIAN_POINT ( 'NONE',  ( 13.00312500061451537, 4.541064518000418104, -2.621784821874998173 ) ) ;
#49920 = CARTESIAN_POINT ( 'NONE',  ( 7.621875000614519280, 3.027376345333613106, -5.243569643749998122 ) ) ;
#49921 = CARTESIAN_POINT ( 'NONE',  ( 6.909375000614518036, 0.000000000000000000, 5.243569643749999010 ) ) ;
#49922 = VERTEX_POINT ( 'NONE', #10251 ) ;
#49923 = CARTESIAN_POINT ( 'NONE',  ( 27.60937500061451644, 0.000000000000000000, 5.243569643749999010 ) ) ;
#49924 = CARTESIAN_POINT ( 'NONE',  ( 18.29062500061451502, -3.027376345333610441, -5.243569643749999898 ) ) ;
#49925 = CARTESIAN_POINT ( 'NONE',  ( 28.91250000122903074, -4.330127018922190985, -2.500000000000001332 ) ) ;
#49926 = CARTESIAN_POINT ( 'NONE',  ( 27.85312500061451502, 4.541064518000418104, -2.621784821874998173 ) ) ;
#49927 = CARTESIAN_POINT ( 'NONE',  ( 24.83437500061451431, 4.541064518000418104, 2.621784821874999949 ) ) ;
#49928 = CARTESIAN_POINT ( 'NONE',  ( 18.77812500061451573, 6.421520780324663323E-16, -5.243569643749999010 ) ) ;
#49929 = CARTESIAN_POINT ( 'NONE',  ( -4.243569643749999898, 19.85937500061451644, 30.00000000000000000 ) ) ;
#49930 = CARTESIAN_POINT ( 'NONE',  ( 25.60312500061451502, 4.541064518000418104, -2.621784821874998173 ) ) ;
#49931 = CARTESIAN_POINT ( 'NONE',  ( 4.200000001229033053, -2.886751345948125991, -5.000000000000000000 ) ) ;
#49932 = EDGE_LOOP ( 'NONE', ( #63975, #26392, #28395, #139 ) ) ;
#49933 = CARTESIAN_POINT ( 'NONE',  ( 26.58750000000000213, -2.886751345948125991, -5.000000000000000000 ) ) ;
#49934 = CARTESIAN_POINT ( 'NONE',  ( -2.000000000000000000, 14.97499999999999964, -33.46410161513775705 ) ) ;
#49935 = CARTESIAN_POINT ( 'NONE',  ( -3.756430356250001434, 18.41562499938548214, 32.16877607737301048 ) ) ;
#49936 = EDGE_CURVE ( 'NONE', #1846, #64001, #16108, .T. ) ;
#49937 = CARTESIAN_POINT ( 'NONE',  ( 4.021875000614516082, 3.027376345333613106, -5.243569643749998122 ) ) ;
#49938 = CARTESIAN_POINT ( 'NONE',  ( 12.66562500061451502, 3.027376345333611329, 5.243569643749999010 ) ) ;
#49939 = CARTESIAN_POINT ( 'NONE',  ( 5.409375000614516260, 4.541064518000418104, -2.621784821874998173 ) ) ;
#49940 = CARTESIAN_POINT ( 'NONE',  ( 23.70000000122903216, 5.773502691896255534, 3.535250795749688894E-16 ) ) ;
#49941 = CARTESIAN_POINT ( 'NONE',  ( 14.97187500061451892, 3.027376345333611329, 5.243569643749999010 ) ) ;
#49942 = CARTESIAN_POINT ( 'NONE',  ( 3.796875000614517326, -3.027376345333614438, 5.243569643749998122 ) ) ;
#49943 = CARTESIAN_POINT ( 'NONE',  ( 29.02499999999999858, 4.330127018922191873, 2.499999999999999556 ) ) ;
#49944 = CARTESIAN_POINT ( 'NONE',  ( 26.82187500061451857, -6.054752690667223547, -1.112240025338166033E-15 ) ) ;
#49945 = CARTESIAN_POINT ( 'NONE',  ( 3.553125000614516082, 4.541064518000418104, -2.621784821874998173 ) ) ;
#49946 = CARTESIAN_POINT ( 'NONE',  ( 13.45312500061451466, 4.541064518000418104, -2.621784821874998173 ) ) ;
#49947 = ORIENTED_EDGE ( 'NONE', *, *, #21313, .T. ) ;
#49948 = CARTESIAN_POINT ( 'NONE',  ( 11.01562500061451821, -6.054752690667223547, -1.112240025338166033E-15 ) ) ;
#49949 = CARTESIAN_POINT ( 'NONE',  ( 7.865625000614516971, -6.054752690667223547, -1.112240025338166033E-15 ) ) ;
#49950 = CARTESIAN_POINT ( 'NONE',  ( 19.28437500061451360, 5.824947211148865298E-16, -4.756430356249998326 ) ) ;
#49951 = CARTESIAN_POINT ( 'NONE',  ( 8.887499999999999289, -2.886751345948129988, 4.999999999999997335 ) ) ;
#49952 = CARTESIAN_POINT ( 'NONE',  ( 2.850000001229036073, -2.886751345948125991, -5.000000000000000000 ) ) ;
#49953 = CARTESIAN_POINT ( 'NONE',  ( 18.52499999999999858, 6.123233995736764310E-16, -4.999999999999998224 ) ) ;
#49954 =( BOUNDED_CURVE ( )  B_SPLINE_CURVE ( 2, ( #17614, #58221, #24613, #11729, #47160, #62693, #655, #56778, #34245 ),
 .UNSPECIFIED., .F., .F. ) 
 B_SPLINE_CURVE_WITH_KNOTS ( ( 3, 2, 2, 2, 3 ),
 ( 0.2500000000000000000, 0.2536231884057971175, 0.2608695652173912971, 0.2681159420289855322, 0.2717391304347826497 ),
 .UNSPECIFIED. ) 
 CURVE ( )  GEOMETRIC_REPRESENTATION_ITEM ( )  RATIONAL_B_SPLINE_CURVE ( ( 0.9330127018922194093, 0.9330127018922190762, 1.000000000000000000, 0.8660254037844387076, 1.000000000000000000, 0.8660254037844387076, 1.000000000000000000, 0.9330127018922188542, 0.9330127018922194093 ) ) 
 REPRESENTATION_ITEM ( '' )  );
#49955 = CARTESIAN_POINT ( 'NONE',  ( 17.74687500061451928, -3.027376345333614438, 5.243569643749998122 ) ) ;
#49956 = CARTESIAN_POINT ( 'NONE',  ( 14.55000000122903181, -2.886751345948125991, -5.000000000000000000 ) ) ;
#49957 = CARTESIAN_POINT ( 'NONE',  ( 19.83750000000000213, -2.886751345948125991, -5.000000000000000000 ) ) ;
#49958 = CARTESIAN_POINT ( 'NONE',  ( 9.001249775931846008E-16, 15.41562500061451679, -25.09994784771203058 ) ) ;
#49959 = CARTESIAN_POINT ( 'NONE',  ( 21.60000000000000142, -4.330127018922190985, -2.500000000000001332 ) ) ;
#49960 = CARTESIAN_POINT ( 'NONE',  ( 25.77187500061451431, -4.119189519843968306, 2.378215178124996054 ) ) ;
#49961 = CARTESIAN_POINT ( 'NONE',  ( 14.41875000122903394, -5.773502691896255534, -1.060575238724906372E-15 ) ) ;
#49962 = CARTESIAN_POINT ( 'NONE',  ( 25.86562500061451431, -6.054752690667223547, -1.112240025338166033E-15 ) ) ;
#49963 = CARTESIAN_POINT ( 'NONE',  ( 20.17500000122903003, 2.886751345948161074, 4.999999999999941380 ) ) ;
#49964 = CARTESIAN_POINT ( 'NONE',  ( 30.00000000000000000, 0.000000000000000000, 0.000000000000000000 ) ) ;
#49965 = CARTESIAN_POINT ( 'NONE',  ( 14.29687500061451821, -3.027376345333610441, -5.243569643749999898 ) ) ;
#49966 = CARTESIAN_POINT ( 'NONE',  ( 25.80000000000000071, 4.330127018922192761, -2.499999999999997780 ) ) ;
#49967 = CARTESIAN_POINT ( 'NONE',  ( 9.403125000614517504, 4.541064518000418104, -2.621784821874998173 ) ) ;
#49968 = CARTESIAN_POINT ( 'NONE',  ( 27.27187500061451786, 5.824947211148865298E-16, -4.756430356249998326 ) ) ;
#49969 = CARTESIAN_POINT ( 'NONE',  ( 21.34687500061451715, -3.027376345333614438, 5.243569643749998122 ) ) ;
#49970 = CARTESIAN_POINT ( 'NONE',  ( 14.52187500061451608, -4.119189519843968306, 2.378215178124996054 ) ) ;
#49971 = CARTESIAN_POINT ( 'NONE',  ( 6.928125000614516082, -4.541064518000419881, 2.621784821874995952 ) ) ;
#49972 = CARTESIAN_POINT ( 'NONE',  ( 11.52187500061451608, -6.054752690667223547, -1.112240025338166033E-15 ) ) ;
#49973 = ORIENTED_EDGE ( 'NONE', *, *, #14935, .F. ) ;
#49974 = CARTESIAN_POINT ( 'NONE',  ( 21.64687500061451786, 6.054752690667223547, 3.707466751127219781E-16 ) ) ;
#49975 = DIRECTION ( 'NONE',  ( -0.000000000000000000, -1.000000000000000000, -0.000000000000000000 ) ) ;
#49976 = CARTESIAN_POINT ( 'NONE',  ( 17.19375000122903430, -2.886751345948070480, -5.000000000000095923 ) ) ;
#49977 = CARTESIAN_POINT ( 'NONE',  ( 4.125000000000000000, 6.123233995736764310E-16, -4.999999999999998224 ) ) ;
#49978 = CARTESIAN_POINT ( 'NONE',  ( 14.58750000122903323, 6.123233995736764310E-16, -4.999999999999998224 ) ) ;
#49979 = CARTESIAN_POINT ( 'NONE',  ( 4.000000000000000000, 15.23750000000000071, -27.69059892324149885 ) ) ;
#49980 = CARTESIAN_POINT ( 'NONE',  ( -5.810221930991193690E-16, 11.90000000122903323, -34.00000000000000000 ) ) ;
#49981 = VERTEX_POINT ( 'NONE', #9520 ) ;
#49982 = CARTESIAN_POINT ( 'NONE',  ( 11.73750000000000249, -2.886751345948125991, -5.000000000000000000 ) ) ;
#49983 = CARTESIAN_POINT ( 'NONE',  ( 15.41250000000000142, 2.886751345948129099, -4.999999999999998224 ) ) ;
#49984 = CARTESIAN_POINT ( 'NONE',  ( 14.02500000122903323, -5.773502691896255534, -1.060575238724906372E-15 ) ) ;
#49985 = CARTESIAN_POINT ( 'NONE',  ( 12.29062500061451857, -3.027376345333614438, 5.243569643749998122 ) ) ;
#49986 = EDGE_CURVE ( 'NONE', #49299, #70620, #9153, .T. ) ;
#49987 = EDGE_LOOP ( 'NONE', ( #34800, #7312, #61005, #39069 ) ) ;
#49988 = CARTESIAN_POINT ( 'NONE',  ( 8.625000000000000000, 6.123233995736764310E-16, -4.999999999999998224 ) ) ;
#49989 = CARTESIAN_POINT ( 'NONE',  ( 27.41250000122903430, 0.000000000000000000, 4.999999999999998224 ) ) ;
#49990 = CARTESIAN_POINT ( 'NONE',  ( 2.121784821875001281, 15.50937500061451857, -26.32496088578401938 ) ) ;
#49991 = CARTESIAN_POINT ( 'NONE',  ( 29.55000000122903003, 5.773502691896255534, 3.535250795749688894E-16 ) ) ;
#49992 = CARTESIAN_POINT ( 'NONE',  ( -1.878215178125001827, 13.84062499938548285, 33.25316411605952283 ) ) ;
#49993 = CARTESIAN_POINT ( 'NONE',  ( 9.825000000000001066, -4.330127018922194537, 2.499999999999995559 ) ) ;
#49994 = LINE ( 'NONE', #43722, #13745 ) ;
#49995 = VERTEX_POINT ( 'NONE', #61217 ) ;
#49996 = CARTESIAN_POINT ( 'NONE',  ( 24.70312500061451644, 4.541064518000418104, -2.621784821874998173 ) ) ;
#49997 = CARTESIAN_POINT ( 'NONE',  ( 3.999999999999998668, 13.51250000000000107, -32.30940107675850470 ) ) ;
#49998 = CARTESIAN_POINT ( 'NONE',  ( 18.93750000122903288, -4.330127018922194537, 2.499999999999995559 ) ) ;
#49999 = CARTESIAN_POINT ( 'NONE',  ( 21.12187500061451573, 3.027376345333613106, -5.243569643749998122 ) ) ;
#50000 = ADVANCED_FACE ( 'NONE', ( #14680 ), #49053, .F. ) ;
#50001 = CARTESIAN_POINT ( 'NONE',  ( 15.96562500061451573, -6.054752690667223547, -1.112240025338166033E-15 ) ) ;
#50002 = CARTESIAN_POINT ( 'NONE',  ( -2.121784821874996840, 11.77812500061459566, -26.32496088578401583 ) ) ;
#50003 = CARTESIAN_POINT ( 'NONE',  ( 5.540625000614515905, -3.027376345333614438, 5.243569643749998122 ) ) ;
#50004 = CARTESIAN_POINT ( 'NONE',  ( 27.52500000122903145, -5.773502691896255534, -1.060575238724906372E-15 ) ) ;
#50005 = CARTESIAN_POINT ( 'NONE',  ( 24.23437500061451644, 5.824947211148865298E-16, -4.756430356249998326 ) ) ;
#50006 = CARTESIAN_POINT ( 'NONE',  ( 19.15312500061451573, -4.541064518000417216, -2.621784821875001281 ) ) ;
#50007 = CARTESIAN_POINT ( 'NONE',  ( 7.546875000614517326, -2.746126346562642428, -4.756430356249999214 ) ) ;
#50008 = CARTESIAN_POINT ( 'NONE',  ( -1.878215178124999163, 18.64062499938548356, 26.74683588394047007 ) ) ;
#50010 = EDGE_CURVE ( 'NONE', #8864, #51420, #70911, .T. ) ;
#50009 = CARTESIAN_POINT ( 'NONE',  ( 14.03437500061451715, 4.541064518000418104, 2.621784821874999949 ) ) ;
#50011 = CARTESIAN_POINT ( 'NONE',  ( 13.65937500061451715, 0.000000000000000000, 5.243569643749999010 ) ) ;
#50012 = CARTESIAN_POINT ( 'NONE',  ( 21.72187500061451715, 3.027376345333611329, 5.243569643749999010 ) ) ;
#50013 = ORIENTED_EDGE ( 'NONE', *, *, #27534, .T. ) ;
#50014 = CARTESIAN_POINT ( 'NONE',  ( 4.243569643749999898, 11.94687500061451857, 32.45002607614398471 ) ) ;
#50015 = CARTESIAN_POINT ( 'NONE',  ( 2.990625000614519191, -3.027376345333610441, -5.243569643749999898 ) ) ;
#50016 = CARTESIAN_POINT ( 'NONE',  ( 27.47812500061451502, 4.541064518000418104, 2.621784821874999949 ) ) ;
#50017 = CARTESIAN_POINT ( 'NONE',  ( 26.50312500061451360, 4.541064518000418104, -2.621784821874998173 ) ) ;
#50018 = CARTESIAN_POINT ( 'NONE',  ( 17.45625000122903003, 0.000000000000000000, 4.999999999999998224 ) ) ;
#50019 = CARTESIAN_POINT ( 'NONE',  ( -2.000000000000000000, 16.77500000000000213, 26.53589838486224650 ) ) ;
#50020 = CARTESIAN_POINT ( 'NONE',  ( 4.321875000614517681, -6.054752690667223547, -1.112240025338166033E-15 ) ) ;
#50021 = CARTESIAN_POINT ( 'NONE',  ( 13.08750000122903323, -4.330127018922194537, 2.499999999999995559 ) ) ;
#50022 = CARTESIAN_POINT ( 'NONE',  ( 9.037500001229034297, -4.330127018922194537, 2.499999999999995559 ) ) ;
#50023 = CARTESIAN_POINT ( 'NONE',  ( 3.665625000614517681, 3.027376345333611329, 5.243569643749999010 ) ) ;
#50024 = CARTESIAN_POINT ( 'NONE',  ( 3.999999999999998668, 18.70624999877096784, 32.30940107675850470 ) ) ;
#50025 = CARTESIAN_POINT ( 'NONE',  ( 18.99375000122903501, -2.886751345948125991, -5.000000000000000000 ) ) ;
#50026 = CARTESIAN_POINT ( 'NONE',  ( 12.90937500061451537, -4.541064518000417216, -2.621784821875001281 ) ) ;
#50027 = CARTESIAN_POINT ( 'NONE',  ( 2.000000000000001332, 14.75000000000000178, -26.53589838486224650 ) ) ;
#50028 = VERTEX_POINT ( 'NONE', #56044 ) ;
#50029 = CARTESIAN_POINT ( 'NONE',  ( 19.37812500061451715, 4.541064518000418104, 2.621784821874999949 ) ) ;
#50030 = CARTESIAN_POINT ( 'NONE',  ( 14.07187500061451679, 3.027376345333611329, 5.243569643749999010 ) ) ;
#50031 = CARTESIAN_POINT ( 'NONE',  ( 5.840625000614516615, 6.054752690667223547, 3.707466751127219781E-16 ) ) ;
#50032 = CARTESIAN_POINT ( 'NONE',  ( 22.54687500061451644, 6.054752690667223547, 3.707466751127219781E-16 ) ) ;
#50033 = CARTESIAN_POINT ( 'NONE',  ( 4.715625000614516615, -6.054752690667223547, -1.112240025338166033E-15 ) ) ;
#50034 = CYLINDRICAL_SURFACE ( 'NONE', #1443, 4.000000000000000000 ) ;
#50035 = CARTESIAN_POINT ( 'NONE',  ( 6.712500001229034119, 0.000000000000000000, 4.999999999999998224 ) ) ;
#50036 = CARTESIAN_POINT ( 'NONE',  ( 19.52812500061451573, -4.541064518000419881, 2.621784821874995952 ) ) ;
#50037 = CARTESIAN_POINT ( 'NONE',  ( 8.325000001229033941, 2.886751345948129099, -4.999999999999998224 ) ) ;
#50038 = CARTESIAN_POINT ( 'NONE',  ( 17.31562500061451715, -6.054752690667223547, -1.112240025338166033E-15 ) ) ;
#50039 = CARTESIAN_POINT ( 'NONE',  ( 15.55312500061451608, -4.541064518000417216, -2.621784821875001281 ) ) ;
#50040 = CARTESIAN_POINT ( 'NONE',  ( 26.52187500061451431, 2.746126346562645981, -4.756430356249997438 ) ) ;
#50041 = CARTESIAN_POINT ( 'NONE',  ( 15.97499999999999964, 4.330127018922191873, 2.499999999999999556 ) ) ;
#50042 = CARTESIAN_POINT ( 'NONE',  ( 12.37500000122903465, 2.886751345948129099, -4.999999999999998224 ) ) ;
#50043 = ADVANCED_FACE ( 'NONE', ( #69218 ), #5436, .F. ) ;
#50044 = CARTESIAN_POINT ( 'NONE',  ( 7.978125000614517681, 6.421520780324663323E-16, -5.243569643749999010 ) ) ;
#50045 = CARTESIAN_POINT ( 'NONE',  ( 11.54062500061451857, -3.027376345333610441, -5.243569643749999898 ) ) ;
#50046 = CARTESIAN_POINT ( 'NONE',  ( 20.28750000122903074, -4.330127018922194537, 2.499999999999995559 ) ) ;
#50047 = CARTESIAN_POINT ( 'NONE',  ( 4.243569643749999010, 12.92187500061451644, -32.45002607614398471 ) ) ;
#50048 = B_SPLINE_CURVE_WITH_KNOTS ( 'NONE', 1,
 ( #13159, #1378 ),
 .UNSPECIFIED., .F., .F.,
 ( 2, 2 ),
 ( 0.000000000000000000, 1.000000000000000000 ),
 .UNSPECIFIED. ) ;
#50049 = CARTESIAN_POINT ( 'NONE',  ( 6.450000001229034829, -2.886751345948125991, -5.000000000000000000 ) ) ;
#50050 = CARTESIAN_POINT ( 'NONE',  ( 4.696875000614518569, -3.027376345333614438, 5.243569643749998122 ) ) ;
#50051 = CARTESIAN_POINT ( 'NONE',  ( 20.63437500061451857, 6.421520780324663323E-16, -5.243569643749999010 ) ) ;
#50052 = CARTESIAN_POINT ( 'NONE',  ( -2.000000000000000000, 14.97499999999999964, 26.53589838486224650 ) ) ;
#50053 = CARTESIAN_POINT ( 'NONE',  ( 15.96562500061451573, -6.054752690667223547, -1.112240025338166033E-15 ) ) ;
#50054 = CARTESIAN_POINT ( 'NONE',  ( 11.79375000122903394, -2.886751345948125991, -5.000000000000000000 ) ) ;
#50055 = CARTESIAN_POINT ( 'NONE',  ( 9.581250001229033586, 6.123233995736764310E-16, -4.999999999999998224 ) ) ;
#50056 = CARTESIAN_POINT ( 'NONE',  ( 28.69687500061451502, -3.027376345333610441, -5.243569643749999898 ) ) ;
#50057 = CARTESIAN_POINT ( 'NONE',  ( 20.93437500061450862, -2.746126346562641984, -4.756430356249999214 ) ) ;
#50058 = AXIS2_PLACEMENT_3D ( 'NONE', #11423, #33940, #56483 ) ;
#50059 = CARTESIAN_POINT ( 'NONE',  ( 14.42812500061451786, 4.541064518000418104, 2.621784821874999949 ) ) ;
#50060 = CARTESIAN_POINT ( 'NONE',  ( 10.84687500061451892, 6.054752690667223547, 3.707466751127219781E-16 ) ) ;
#50061 = ORIENTED_EDGE ( 'NONE', *, *, #19119, .T. ) ;
#50062 = CARTESIAN_POINT ( 'NONE',  ( 3.479729569495786379, -3.590471016896914946, -3.821457900550485398 ) ) ;
#50063 = CARTESIAN_POINT ( 'NONE',  ( 21.62812500061451360, 4.541064518000418104, 2.621784821874999949 ) ) ;
#50064 = FACE_OUTER_BOUND ( 'NONE', #5224, .T. ) ;
#50065 = CARTESIAN_POINT ( 'NONE',  ( 28.72500000122903074, 2.886751345948164182, 4.999999999999933387 ) ) ;
#50066 = CARTESIAN_POINT ( 'NONE',  ( 13.27500000000000213, 4.330127018922191873, 2.499999999999999556 ) ) ;
#50067 = CARTESIAN_POINT ( 'NONE',  ( 21.90000000122903145, 5.773502691896255534, 3.535250795749688894E-16 ) ) ;
#50068 = CARTESIAN_POINT ( 'NONE',  ( 17.24062500061451786, -3.027376345333614438, 5.243569643749998122 ) ) ;
#50069 = CARTESIAN_POINT ( 'NONE',  ( 12.98437500061451289, 5.492252693125287522, 3.363034840372157021E-16 ) ) ;
#50070 = ORIENTED_EDGE ( 'NONE', *, *, #31407, .F. ) ;
#50071 = CARTESIAN_POINT ( 'NONE',  ( 20.66250000000000142, -5.773502691896255534, -1.060575238724906372E-15 ) ) ;
#50072 = CARTESIAN_POINT ( 'NONE',  ( 20.93437500061451573, -4.541064518000419881, 2.621784821874995952 ) ) ;
#50073 = CARTESIAN_POINT ( 'NONE',  ( 28.60312500061451502, -4.541064518000417216, -2.621784821875001281 ) ) ;
#50074 = VERTEX_POINT ( 'NONE', #23763 ) ;
#50075 = CARTESIAN_POINT ( 'NONE',  ( 0.000000000000000000, 20.00000000000000000, -33.99999999999999289 ) ) ;
#50076 = CARTESIAN_POINT ( 'NONE',  ( 9.590625000614517504, -3.027376345333614438, 5.243569643749998122 ) ) ;
#50077 = CARTESIAN_POINT ( 'NONE',  ( 6.299999999999999822, -4.330127018922190985, -2.500000000000001332 ) ) ;
#50078 = CARTESIAN_POINT ( 'NONE',  ( 13.88437500061451502, 5.492252693125287522, 3.363034840372157021E-16 ) ) ;
#50079 = CARTESIAN_POINT ( 'NONE',  ( 16.61250000000000426, -5.773502691896255534, -1.060575238724906372E-15 ) ) ;
#50080 = CARTESIAN_POINT ( 'NONE',  ( 23.81250000000000000, -5.773502691896255534, -1.060575238724906372E-15 ) ) ;
#50081 = CARTESIAN_POINT ( 'NONE',  ( 3.557364438369462256, -3.513567738442655131, -3.708418381339127379 ) ) ;
#50082 = CARTESIAN_POINT ( 'NONE',  ( 3.346875000614518036, -3.027376345333614438, 5.243569643749998122 ) ) ;
#50083 = CARTESIAN_POINT ( 'NONE',  ( 28.09687500061451360, -3.027376345333614438, 5.243569643749998122 ) ) ;
#50084 = ORIENTED_EDGE ( 'NONE', *, *, #45040, .F. ) ;
#50085 = CARTESIAN_POINT ( 'NONE',  ( 23.65312500061451573, -4.541064518000417216, -2.621784821875001281 ) ) ;
#50086 = CARTESIAN_POINT ( 'NONE',  ( 25.43437500061451573, -4.541064518000419881, 2.621784821874995952 ) ) ;
#50087 = CARTESIAN_POINT ( 'NONE',  ( -4.243569643749999898, 19.76562500061459104, -32.45002607614398471 ) ) ;
#50088 = CARTESIAN_POINT ( 'NONE',  ( 14.32500000000000107, -4.330127018922194537, 2.499999999999995559 ) ) ;
#50089 = CARTESIAN_POINT ( 'NONE',  ( 11.65312500061451573, 4.541064518000418104, -2.621784821874998173 ) ) ;
#50090 = CARTESIAN_POINT ( 'NONE',  ( 3.787803386340530043, 3.263823755417472050, 3.928545305590518399 ) ) ;
#50091 = CARTESIAN_POINT ( 'NONE',  ( 7.050000000000000711, 0.000000000000000000, 4.999999999999998224 ) ) ;
#50092 = CARTESIAN_POINT ( 'NONE',  ( 25.67812500061451431, 4.541064518000418104, 2.621784821874999949 ) ) ;
#50093 = CARTESIAN_POINT ( 'NONE',  ( 17.10000000122903430, -2.886751345948129988, 4.999999999999997335 ) ) ;
#50094 = CARTESIAN_POINT ( 'NONE',  ( 22.59375000122903288, -2.886751345948126435, -5.000000000000000000 ) ) ;
#50095 = CARTESIAN_POINT ( 'NONE',  ( 15.08437500061451786, -4.119189519843968306, 2.378215178124996054 ) ) ;
#50096 = FACE_OUTER_BOUND ( 'NONE', #49183, .T. ) ;
#50097 = CARTESIAN_POINT ( 'NONE',  ( 21.12187500061451573, 3.027376345333613106, -5.243569643749998122 ) ) ;
#50098 = CARTESIAN_POINT ( 'NONE',  ( 2.121784821874999061, 14.75937500061451679, 26.32496088578401583 ) ) ;
#50099 = EDGE_CURVE ( 'NONE', #48021, #41736, #3385, .T. ) ;
#50100 = CARTESIAN_POINT ( 'NONE',  ( 21.27187500061451786, 3.027376345333611329, 5.243569643749999010 ) ) ;
#50101 = CARTESIAN_POINT ( 'NONE',  ( 28.65937500061451715, -4.541064518000417216, -2.621784821875001281 ) ) ;
#50102 = CARTESIAN_POINT ( 'NONE',  ( 2.121784821875001281, 18.65937500061451715, 33.67503911421598417 ) ) ;
#50103 = CARTESIAN_POINT ( 'NONE',  ( 8.728125000614518569, -4.541064518000419881, 2.621784821874995952 ) ) ;
#50104 = CARTESIAN_POINT ( 'NONE',  ( 8.175000000000002487, 6.123233995736764310E-16, -4.999999999999998224 ) ) ;
#50105 = CARTESIAN_POINT ( 'NONE',  ( 6.384375000614516793, 4.541064518000418104, 2.621784821874999949 ) ) ;
#50106 = CARTESIAN_POINT ( 'NONE',  ( 3.837848076843224376, 3.204827942194517831, -3.837848076843224376 ) ) ;
#50107 = CARTESIAN_POINT ( 'NONE',  ( 7.940625000614518036, -3.027376345333610441, -5.243569643749999898 ) ) ;
#50108 = CARTESIAN_POINT ( 'NONE',  ( 12.23437500061451821, 4.541064518000418104, 2.621784821874999949 ) ) ;
#50109 = CARTESIAN_POINT ( 'NONE',  ( -4.000000000000000000, 19.02499999999999858, 30.00000000000000000 ) ) ;
#50110 = CARTESIAN_POINT ( 'NONE',  ( 20.17500000122903359, 2.886751345948126879, 4.999999999999999112 ) ) ;
#50111 = CARTESIAN_POINT ( 'NONE',  ( 8.296875000614516438, -3.027376345333614438, 5.243569643749998122 ) ) ;
#50112 = CARTESIAN_POINT ( 'NONE',  ( 9.928125000614517859, 4.541064518000418104, 2.621784821874999949 ) ) ;
#50113 = CARTESIAN_POINT ( 'NONE',  ( 6.215625000614517504, 3.027376345333612662, -5.243569643749998122 ) ) ;
#50114 = CARTESIAN_POINT ( 'NONE',  ( 25.25625000122903074, -4.330127018922190985, -2.500000000000001332 ) ) ;
#50115 = CARTESIAN_POINT ( 'NONE',  ( 18.75937500061451857, -4.541064518000417216, -2.621784821875001281 ) ) ;
#50116 = CARTESIAN_POINT ( 'NONE',  ( -2.000000000000000000, 11.48750000122903359, 26.53589838486224650 ) ) ;
#50117 = CARTESIAN_POINT ( 'NONE',  ( 27.55312500061451786, 0.000000000000000000, 5.243569643749999010 ) ) ;
#50118 = CARTESIAN_POINT ( 'NONE',  ( 12.85312500061451502, -4.541064518000417216, -2.621784821875001281 ) ) ;
#50119 = CARTESIAN_POINT ( 'NONE',  ( 28.92187500061451644, 3.027376345333611329, 5.243569643749999010 ) ) ;
#50120 = CARTESIAN_POINT ( 'NONE',  ( 9.001249775931846008E-16, 12.77187500061451786, -25.09994784771203058 ) ) ;
#50121 = CARTESIAN_POINT ( 'NONE',  ( 13.16250000122903430, -4.330127018922190985, -2.500000000000001332 ) ) ;
#50122 = CARTESIAN_POINT ( 'NONE',  ( 4.243569643749999898, 15.49062500061451786, -27.54997392385601529 ) ) ;
#50123 = CARTESIAN_POINT ( 'NONE',  ( 15.07500000122903394, 2.886751345948129099, -4.999999999999998224 ) ) ;
#50124 = CARTESIAN_POINT ( 'NONE',  ( 9.403125000614517504, 4.541064518000418104, -2.621784821874998173 ) ) ;
#50125 = VECTOR ( 'NONE', #57828, 1000.000000000000000 ) ;
#50126 = CARTESIAN_POINT ( 'NONE',  ( 12.78749999999999964, 5.773502691896255534, 3.535250795749688894E-16 ) ) ;
#50127 = CARTESIAN_POINT ( 'NONE',  ( 13.70625000122903359, 4.330127018922192761, -2.499999999999997780 ) ) ;
#50128 = CARTESIAN_POINT ( 'NONE',  ( 22.75312500061451360, -4.541064518000417216, -2.621784821875001281 ) ) ;
#50129 = CARTESIAN_POINT ( 'NONE',  ( 7.621875000614519280, 3.027376345333612662, -5.243569643749998122 ) ) ;
#50130 = CARTESIAN_POINT ( 'NONE',  ( 10.65000000122903323, 5.773502691896255534, 3.535250795749688894E-16 ) ) ;
#50131 = CARTESIAN_POINT ( 'NONE',  ( 17.85000000122903430, 5.773502691896255534, 3.535250795749688894E-16 ) ) ;
#50132 = CARTESIAN_POINT ( 'NONE',  ( 15.40312500061451573, 0.000000000000000000, 5.243569643749999010 ) ) ;
#50133 = CARTESIAN_POINT ( 'NONE',  ( 19.41562500061451146, 3.027376345333611329, 5.243569643749999010 ) ) ;
#50134 = CARTESIAN_POINT ( 'NONE',  ( 25.16250000122903074, 0.000000000000000000, 4.999999999999998224 ) ) ;
#50135 = VECTOR ( 'NONE', #64503, 1000.000000000000000 ) ;
#50136 = CARTESIAN_POINT ( 'NONE',  ( 27.18750000122903288, 6.123233995736764310E-16, -4.999999999999998224 ) ) ;
#50137 = CARTESIAN_POINT ( 'NONE',  ( 21.56250000000000000, -5.773502691896255534, -1.060575238724906372E-15 ) ) ;
#50138 = CARTESIAN_POINT ( 'NONE',  ( 3.756430356250000102, 14.89062499938548356, 30.00000000000000000 ) ) ;
#50139 = VECTOR ( 'NONE', #12149, 1000.000000000000000 ) ;
#50140 = CARTESIAN_POINT ( 'NONE',  ( 25.84687500061451360, -3.027376345333614438, 5.243569643749998122 ) ) ;
#50141 = CARTESIAN_POINT ( 'NONE',  ( 18.18750000122903288, 6.123233995736764310E-16, -4.999999999999998224 ) ) ;
#50142 = EDGE_CURVE ( 'NONE', #19257, #59354, #20400, .T. ) ;
#50143 = CARTESIAN_POINT ( 'NONE',  ( 11.51250000122903216, 4.330127018922192761, -2.499999999999997780 ) ) ;
#50144 = CARTESIAN_POINT ( 'NONE',  ( 28.88437500061451502, 4.541064518000418104, 2.621784821874999949 ) ) ;
#50145 = FACE_OUTER_BOUND ( 'NONE', #8852, .T. ) ;
#50146 = CARTESIAN_POINT ( 'NONE',  ( 4.434375000614519280, 6.421520780324663323E-16, -5.243569643749999010 ) ) ;
#50147 = CARTESIAN_POINT ( 'NONE',  ( 23.99062500061451786, -3.027376345333614438, 5.243569643749998122 ) ) ;
#50148 = CARTESIAN_POINT ( 'NONE',  ( -1.878215178125001827, 13.95312499938548356, 33.25316411605952283 ) ) ;
#50149 = CARTESIAN_POINT ( 'NONE',  ( 10.65937500061451715, -4.541064518000417216, -2.621784821875001281 ) ) ;
#50150 = LINE ( 'NONE', #44620, #44238 ) ;
#50151 = CARTESIAN_POINT ( 'NONE',  ( 29.57812500061451644, 6.421520780324663323E-16, -5.243569643749999010 ) ) ;
#50152 = CARTESIAN_POINT ( 'NONE',  ( 6.946875000614517681, -3.027376345333614438, 5.243569643749998122 ) ) ;
#50153 = CARTESIAN_POINT ( 'NONE',  ( 29.67187500061451644, 3.027376345333613106, -5.243569643749998122 ) ) ;
#50154 = CARTESIAN_POINT ( 'NONE',  ( 29.15625000122903288, 0.000000000000000000, 4.999999999999998224 ) ) ;
#50155 = CARTESIAN_POINT ( 'NONE',  ( 19.34999999999999787, -4.330127018922190985, -2.500000000000001332 ) ) ;
#50156 = ORIENTED_EDGE ( 'NONE', *, *, #7027, .T. ) ;
#50157 = CARTESIAN_POINT ( 'NONE',  ( 27.48749999999999716, -2.886751345948125991, -5.000000000000000000 ) ) ;
#50158 = CARTESIAN_POINT ( 'NONE',  ( 29.29687500061451644, 6.054752690667223547, 3.707466751127219781E-16 ) ) ;
#50159 = ORIENTED_EDGE ( 'NONE', *, *, #50272, .F. ) ;
#50160 = CARTESIAN_POINT ( 'NONE',  ( 18.55312500061451431, 0.000000000000000000, 5.243569643749999010 ) ) ;
#50161 = CARTESIAN_POINT ( 'NONE',  ( 9.028125000614517504, 4.541064518000418104, 2.621784821874999949 ) ) ;
#50162 = CARTESIAN_POINT ( 'NONE',  ( 21.45937500061451075, 2.746126346562645981, -4.756430356249997438 ) ) ;
#50163 = CARTESIAN_POINT ( 'NONE',  ( 5.596875000614516260, -3.027376345333614438, 5.243569643749998122 ) ) ;
#50164 = CARTESIAN_POINT ( 'NONE',  ( 17.51250000122903216, 0.000000000000000000, 4.999999999999998224 ) ) ;
#50165 = VECTOR ( 'NONE', #67546, 1000.000000000000000 ) ;
#50166 = CARTESIAN_POINT ( 'NONE',  ( 2.000000000000001332, 13.85000000000000142, -26.53589838486224650 ) ) ;
#50167 = CARTESIAN_POINT ( 'NONE',  ( 6.571875000614517681, -6.054752690667223547, -1.112240025338166033E-15 ) ) ;
#50168 = CARTESIAN_POINT ( 'NONE',  ( 12.64687500061451608, 6.054752690667223547, 3.707466751127219781E-16 ) ) ;
#50169 = CARTESIAN_POINT ( 'NONE',  ( 21.72187500061451715, 3.027376345333611329, 5.243569643749999010 ) ) ;
#50170 = CARTESIAN_POINT ( 'NONE',  ( 4.000000000000000000, 15.80000000122903181, -27.69059892324149885 ) ) ;
#50171 = EDGE_LOOP ( 'NONE', ( #5056, #50785, #15995, #44840 ) ) ;
#50172 = CARTESIAN_POINT ( 'NONE',  ( 11.55000000000000071, 0.000000000000000000, 4.999999999999998224 ) ) ;
#50173 = AXIS2_PLACEMENT_3D ( 'NONE', #22508, #19031, #45418 ) ;
#50174 = CARTESIAN_POINT ( 'NONE',  ( 6.196875000614515905, -3.027376345333610441, -5.243569643749999898 ) ) ;
#50175 = CARTESIAN_POINT ( 'NONE',  ( 2.655984681222220721E-16, 15.90312499938548108, 25.66244784525396483 ) ) ;
#50176 = CARTESIAN_POINT ( 'NONE',  ( 19.87500000000000000, 6.123233995736764310E-16, -4.999999999999998224 ) ) ;
#50177 = CARTESIAN_POINT ( 'NONE',  ( 17.99062500061451786, 6.054752690667223547, 3.707466751127219781E-16 ) ) ;
#50178 = CARTESIAN_POINT ( 'NONE',  ( -4.000000000000000000, 17.22500000000000142, 30.00000000000000000 ) ) ;
#50179 = ADVANCED_FACE ( 'NONE', ( #50145 ), #64016, .F. ) ;
#50180 = CARTESIAN_POINT ( 'NONE',  ( 22.77187500061451786, -5.492252693125287522, -1.008910452111647106E-15 ) ) ;
#50181 = CARTESIAN_POINT ( 'NONE',  ( 13.37812500061451715, 6.421520780324663323E-16, -5.243569643749999010 ) ) ;
#50182 = CARTESIAN_POINT ( 'NONE',  ( 29.63437500061451502, 6.421520780324663323E-16, -5.243569643749999010 ) ) ;
#50183 = DIRECTION ( 'NONE',  ( -1.000000000000000000, -0.000000000000000000, -0.000000000000000000 ) ) ;
#50184 = CARTESIAN_POINT ( 'NONE',  ( 29.74687500061451217, 6.054752690667223547, 3.707466751127219781E-16 ) ) ;
#50185 = CARTESIAN_POINT ( 'NONE',  ( 10.61250000000000071, 2.886751345948126879, 4.999999999999999112 ) ) ;
#50186 = EDGE_CURVE ( 'NONE', #14890, #23263, #61571, .T. ) ;
#50187 = CARTESIAN_POINT ( 'NONE',  ( -2.000000000000000000, 15.53750000122903430, 26.53589838486224650 ) ) ;
#50189 =( BOUNDED_CURVE ( )  B_SPLINE_CURVE ( 2, ( #9369, #54438, #44823, #30262, #56264, #7728, #6008, #39642, #2196 ),
 .UNSPECIFIED., .F., .F. ) 
 B_SPLINE_CURVE_WITH_KNOTS ( ( 3, 2, 2, 2, 3 ),
 ( 0.6413043478260869179, 0.6449275362318840354, 0.6521739130434782705, 0.6594202898550725056, 0.6630434782608696231 ),
 .UNSPECIFIED. ) 
 CURVE ( )  GEOMETRIC_REPRESENTATION_ITEM ( )  RATIONAL_B_SPLINE_CURVE ( ( 0.9330127018922194093, 0.9330127018922194093, 1.000000000000000000, 0.8660254037844387076, 1.000000000000000000, 0.8660254037844387076, 1.000000000000000000, 0.9330127018922182991, 0.9330127018922192983 ) ) 
 REPRESENTATION_ITEM ( '' )  );
#50188 = CARTESIAN_POINT ( 'NONE',  ( 8.812500001229034652, 4.330127018922192761, -2.499999999999997780 ) ) ;
#50190 = VECTOR ( 'NONE', #7252, 1000.000000000000000 ) ;
#50191 = CARTESIAN_POINT ( 'NONE',  ( 20.93437500061451573, -4.541064518000419881, 2.621784821874995952 ) ) ;
#50192 = CARTESIAN_POINT ( 'NONE',  ( 14.44687500061451679, 6.054752690667223547, 3.707466751127219781E-16 ) ) ;
#50193 = ORIENTED_EDGE ( 'NONE', *, *, #68511, .F. ) ;
#50194 = CARTESIAN_POINT ( 'NONE',  ( 15.44062500061451537, -3.027376345333614438, 5.243569643749998122 ) ) ;
#50195 = AXIS2_PLACEMENT_3D ( 'NONE', #6480, #68902, #7923 ) ;
#50196 = CARTESIAN_POINT ( 'NONE',  ( 25.83750000122903501, 6.123233995736764310E-16, -4.999999999999998224 ) ) ;
#50197 = CARTESIAN_POINT ( 'NONE',  ( 15.15937500061451715, -4.541064518000417216, -2.621784821875001281 ) ) ;
#50198 = CARTESIAN_POINT ( 'NONE',  ( 2.692168354449048895, 9.632460402479562589, -24.63433627171737328 ) ) ;
#50199 = CARTESIAN_POINT ( 'NONE',  ( 17.12812500061451715, 4.541064518000418104, 2.621784821874999949 ) ) ;
#50200 = CARTESIAN_POINT ( 'NONE',  ( 18.00000000122903288, -2.886751345948130876, 4.999999999999996447 ) ) ;
#50201 = CARTESIAN_POINT ( 'NONE',  ( 26.33437500061451431, -4.541064518000419881, 2.621784821874995952 ) ) ;
#50202 = CARTESIAN_POINT ( 'NONE',  ( -4.243569643749999898, 10.76562500061451644, 27.54997392385601529 ) ) ;
#50203 = CARTESIAN_POINT ( 'NONE',  ( 15.68437500061451573, 6.421520780324663323E-16, -5.243569643749999010 ) ) ;
#50204 = CARTESIAN_POINT ( 'NONE',  ( 15.11250000122903359, 4.330127018922192761, -2.499999999999997780 ) ) ;
#50205 = CARTESIAN_POINT ( 'NONE',  ( 9.159375000614515372, 0.000000000000000000, 4.756430356249998326 ) ) ;
#50206 = CARTESIAN_POINT ( 'NONE',  ( 3.348770750331622637, -3.712914550824308879, 3.702605588924299695 ) ) ;
#50207 = CARTESIAN_POINT ( 'NONE',  ( 19.47187500061451360, 3.027376345333611329, 5.243569643749999010 ) ) ;
#50208 = CARTESIAN_POINT ( 'NONE',  ( 19.31250000122903288, 0.000000000000000000, 4.999999999999998224 ) ) ;
#50209 = CARTESIAN_POINT ( 'NONE',  ( 18.04687500061451999, 6.054752690667223547, 3.707466751127219781E-16 ) ) ;
#50210 = CARTESIAN_POINT ( 'NONE',  ( 9.001249775931846008E-16, 11.42187500061451999, 34.90005215228797653 ) ) ;
#50211 = CARTESIAN_POINT ( 'NONE',  ( 18.25312500061451715, -4.541064518000417216, -2.621784821875001281 ) ) ;
#50212 = ORIENTED_EDGE ( 'NONE', *, *, #68849, .T. ) ;
#50213 = ORIENTED_EDGE ( 'NONE', *, *, #6144, .T. ) ;
#50214 = CARTESIAN_POINT ( 'NONE',  ( 19.57500000000000284, 4.330127018922191873, 2.499999999999999556 ) ) ;
#50215 = CARTESIAN_POINT ( 'NONE',  ( 28.12500000122902932, 2.886751345948125103, -5.000000000000004441 ) ) ;
#50216 = CARTESIAN_POINT ( 'NONE',  ( 24.21562500061451573, 3.027376345333613106, -5.243569643749998122 ) ) ;
#50217 = CARTESIAN_POINT ( 'NONE',  ( 4.340625000614515727, -3.027376345333610441, -5.243569643749999898 ) ) ;
#50218 = CARTESIAN_POINT ( 'NONE',  ( 16.98750000122903359, 4.330127018922191873, 2.499999999999999556 ) ) ;
#50219 = CARTESIAN_POINT ( 'NONE',  ( 22.41562500061451502, 3.027376345333613106, -5.243569643749998122 ) ) ;
#50220 = CARTESIAN_POINT ( 'NONE',  ( 21.33749999999999858, 5.773502691896255534, 3.535250795749688894E-16 ) ) ;
#50221 = CARTESIAN_POINT ( 'NONE',  ( 25.60312500061451502, 4.541064518000418104, -2.621784821874998173 ) ) ;
#50222 = CARTESIAN_POINT ( 'NONE',  ( 5.878125000614517148, 4.541064518000418104, 2.621784821874999949 ) ) ;
#50223 = ORIENTED_EDGE ( 'NONE', *, *, #5878, .F. ) ;
#50224 = B_SPLINE_CURVE_WITH_KNOTS ( 'NONE', 3,
 ( #29513, #19868, #12876, #2527, #30961, #7701, #63842, #58661, #52770, #8425, #13233, #36142, #57934, #70120, #52048, #29870, #52408, #63488, #7341, #35409, #13966, #36504, #2172, #24683, #64578, #1452, #13596, #35771, #53497, #1816, #8069, #23958 ),
 .UNSPECIFIED., .F., .F.,
 ( 4, 2, 2, 2, 2, 2, 2, 2, 2, 2, 2, 2, 2, 2, 2, 4 ),
 ( 0.000000000000000000, 0.0007851728441139026876, 0.001570345688227805375, 0.002355518532341708063, 0.003140691376455610750, 0.003925864220569513438, 0.004711037064683416126, 0.005496209908797318813, 0.006281382752911221501, 0.007066555597025125056, 0.007851728441139026876, 0.009422074129366811435, 0.01020724697348069851, 0.01099241981759458385, 0.01177759266170846919, 0.01256276550582235453 ),
 .UNSPECIFIED. ) ;
#50225 = CARTESIAN_POINT ( 'NONE',  ( 26.81250000122903288, 4.330127018922192761, -2.499999999999997780 ) ) ;
#50226 = VECTOR ( 'NONE', #54620, 1000.000000000000000 ) ;
#50227 = CARTESIAN_POINT ( 'NONE',  ( 11.55937500061451928, -4.119189519843965641, -2.378215178125001383 ) ) ;
#50228 = CARTESIAN_POINT ( 'NONE',  ( 2.000000000000001332, 12.95000000000000107, 33.46410161513774995 ) ) ;
#50229 = CARTESIAN_POINT ( 'NONE',  ( 8.484601909799253346E-16, 11.22500000122903607, -25.38119784648299770 ) ) ;
#50230 = CARTESIAN_POINT ( 'NONE',  ( 2.121784821875001281, 19.10937500061451644, -26.32496088578401938 ) ) ;
#50231 = AXIS2_PLACEMENT_3D ( 'NONE', #40717, #63234, #61783 ) ;
#50232 = CARTESIAN_POINT ( 'NONE',  ( 8.812500000000000000, 2.886751345948126879, 4.999999999999999112 ) ) ;
#50234 = CARTESIAN_POINT ( 'NONE',  ( 9.684375000614517504, -4.541064518000419881, 2.621784821874995952 ) ) ;
#50233 = VECTOR ( 'NONE', #30767, 1000.000000000000000 ) ;
#50235 = CARTESIAN_POINT ( 'NONE',  ( 6.037500001229035185, 6.123233995736764310E-16, -4.999999999999998224 ) ) ;
#50236 = CARTESIAN_POINT ( 'NONE',  ( 13.43437500061451750, 6.421520780324663323E-16, -5.243569643749999010 ) ) ;
#50237 = CARTESIAN_POINT ( 'NONE',  ( 30.00000000000000000, 6.123233995736764310E-16, -4.999999999999998224 ) ) ;
#50238 = CARTESIAN_POINT ( 'NONE',  ( 4.696875000614518569, -3.027376345333614438, 5.243569643749998122 ) ) ;
#50239 = CARTESIAN_POINT ( 'NONE',  ( 0.000000000000000000, 20.00000000000000000, -36.00000000000000000 ) ) ;
#50240 = VECTOR ( 'NONE', #66979, 1000.000000000000000 ) ;
#50241 = CARTESIAN_POINT ( 'NONE',  ( 3.504965621013899746, 3.565840152826760256, 3.504965621013765631 ) ) ;
#50242 = CARTESIAN_POINT ( 'NONE',  ( 10.95937500061451964, 0.000000000000000000, 5.243569643749999010 ) ) ;
#50243 = DIRECTION ( 'NONE',  ( 0.000000000000000000, 0.000000000000000000, 1.000000000000000000 ) ) ;
#50244 = CARTESIAN_POINT ( 'NONE',  ( 20.76562500061451644, 3.027376345333611329, 5.243569643749999010 ) ) ;
#50245 = CARTESIAN_POINT ( 'NONE',  ( 4.661467738957716378, -1.808512791952580301, -4.661467738957749241 ) ) ;
#50246 = CARTESIAN_POINT ( 'NONE',  ( -4.243569643749999898, 16.65312500061459744, 30.00000000000000000 ) ) ;
#50247 = CARTESIAN_POINT ( 'NONE',  ( 24.68437500061451573, 6.421520780324663323E-16, -5.243569643749999010 ) ) ;
#50248 = CARTESIAN_POINT ( 'NONE',  ( 2.854733137546939137, -4.104967572847192159, 3.224293301434809411 ) ) ;
#50249 = CARTESIAN_POINT ( 'NONE',  ( 28.87500000122902932, -5.773502691896255534, -1.060575238724906372E-15 ) ) ;
#50250 = CARTESIAN_POINT ( 'NONE',  ( 20.25937500061451502, 2.746126346562643317, 4.756430356249998326 ) ) ;
#50251 = CARTESIAN_POINT ( 'NONE',  ( 24.70312500061451644, 4.541064518000418104, -2.621784821874998173 ) ) ;
#50252 = CARTESIAN_POINT ( 'NONE',  ( 15.62812500061451537, 6.421520780324663323E-16, -5.243569643749999010 ) ) ;
#50253 = CARTESIAN_POINT ( 'NONE',  ( 14.83125000122903359, -4.330127018922194537, 2.499999999999995559 ) ) ;
#50254 = CARTESIAN_POINT ( 'NONE',  ( 13.99687500061451928, 6.054752690667223547, 3.707466751127219781E-16 ) ) ;
#50255 = CARTESIAN_POINT ( 'NONE',  ( 7.471875000614514484, 5.824947211148865298E-16, -4.756430356249998326 ) ) ;
#50256 = CARTESIAN_POINT ( 'NONE',  ( 24.22500000122903430, 2.886751345948126879, 4.999999999999999112 ) ) ;
#50257 = DIRECTION ( 'NONE',  ( 0.000000000000000000, 0.000000000000000000, -1.000000000000000000 ) ) ;
#50258 = CARTESIAN_POINT ( 'NONE',  ( 13.13437500061451857, 4.541064518000418104, 2.621784821874999949 ) ) ;
#50259 = CARTESIAN_POINT ( 'NONE',  ( 4.843974908776027988, -1.239501918800440361, -5.095008608840551290 ) ) ;
#50260 = FACE_OUTER_BOUND ( 'NONE', #51607, .T. ) ;
#50261 = CARTESIAN_POINT ( 'NONE',  ( 25.80937500061451928, 0.000000000000000000, 5.243569643749999010 ) ) ;
#50262 = CARTESIAN_POINT ( 'NONE',  ( 17.59687500061451715, 6.054752690667223547, 3.707466751127219781E-16 ) ) ;
#50263 = CARTESIAN_POINT ( 'NONE',  ( 3.756430356250000102, 16.35312499938548569, 30.00000000000000000 ) ) ;
#50264 = CARTESIAN_POINT ( 'NONE',  ( 28.08749999999999858, 5.773502691896255534, 3.535250795749688894E-16 ) ) ;
#50265 = CARTESIAN_POINT ( 'NONE',  ( 3.675000001229035362, -5.773502691896255534, -1.060575238724906372E-15 ) ) ;
#50266 = CARTESIAN_POINT ( 'NONE',  ( 6.187500000000002665, -2.886751345948129988, 4.999999999999997335 ) ) ;
#50267 = CARTESIAN_POINT ( 'NONE',  ( 29.29687500061451644, 5.492252693125287522, 3.363034840372157021E-16 ) ) ;
#50268 = CARTESIAN_POINT ( 'NONE',  ( 19.49062500061451431, -3.027376345333614438, 5.243569643749998122 ) ) ;
#50269 = CARTESIAN_POINT ( 'NONE',  ( 9.375000000000001776, -4.330127018922194537, 2.499999999999995559 ) ) ;
#50270 = CARTESIAN_POINT ( 'NONE',  ( 15.45000000000000107, 4.330127018922192761, -2.499999999999997780 ) ) ;
#50271 = CARTESIAN_POINT ( 'NONE',  ( 16.94999999999999929, 0.000000000000000000, 4.999999999999998224 ) ) ;
#50272 = EDGE_CURVE ( 'NONE', #19034, #70765, #48250, .T. ) ;
#50273 = CARTESIAN_POINT ( 'NONE',  ( 4.243569643749999010, 13.31562500061451537, 27.54997392385601174 ) ) ;
#50274 = DIRECTION ( 'NONE',  ( -0.000000000000000000, -1.000000000000000000, -0.000000000000000000 ) ) ;
#50275 = CARTESIAN_POINT ( 'NONE',  ( 19.80000000122903359, -2.886751345948129988, 4.999999999999997335 ) ) ;
#50276 = CARTESIAN_POINT ( 'NONE',  ( 5.999957575222543582, 8.000031818581996745, 30.20273605092067726 ) ) ;
#50277 = CARTESIAN_POINT ( 'NONE',  ( 28.35937500061451289, 4.541064518000418104, -2.621784821874998173 ) ) ;
#50278 = ORIENTED_EDGE ( 'NONE', *, *, #21587, .F. ) ;
#50279 = CARTESIAN_POINT ( 'NONE',  ( 17.01562500061451644, 3.027376345333613106, -5.243569643749998122 ) ) ;
#50280 = CARTESIAN_POINT ( 'NONE',  ( 21.29062500061451502, -3.027376345333614438, 5.243569643749998122 ) ) ;
#50281 = CARTESIAN_POINT ( 'NONE',  ( 23.52187500061451786, 3.027376345333611329, 5.243569643749999010 ) ) ;
#50282 = CARTESIAN_POINT ( 'NONE',  ( 5.662500000000000533, 2.886751345948126879, 4.999999999999999112 ) ) ;
#50283 = CARTESIAN_POINT ( 'NONE',  ( 10.41562500061451679, 3.027376345333611329, 5.243569643749999010 ) ) ;
#50284 = CARTESIAN_POINT ( 'NONE',  ( 25.45312500061451644, -4.541064518000417216, -2.621784821875001281 ) ) ;
#50285 = CARTESIAN_POINT ( 'NONE',  ( 13.95937500061451786, 4.541064518000418104, -2.621784821874998173 ) ) ;
#50286 = CARTESIAN_POINT ( 'NONE',  ( 19.13437500061451857, -4.541064518000419881, 2.621784821874995952 ) ) ;
#50287 = CARTESIAN_POINT ( 'NONE',  ( 1.071796769724489895, 12.32990381179670081, -34.00000000000000000 ) ) ;
#50288 = CARTESIAN_POINT ( 'NONE',  ( -4.243569643749999898, 18.90312500061451573, 30.00000000000000000 ) ) ;
#50289 = CARTESIAN_POINT ( 'NONE',  ( 21.41250000122903074, 4.330127018922192761, -2.499999999999997780 ) ) ;
#50290 = CARTESIAN_POINT ( 'NONE',  ( 17.82187500061451502, -5.492252693125287522, -1.008910452111647106E-15 ) ) ;
#50291 = CARTESIAN_POINT ( 'NONE',  ( 12.55312500061451786, 4.541064518000418104, -2.621784821874998173 ) ) ;
#50292 = APPLICATION_CONTEXT ( 'automotive_design' ) ;
#50293 = CARTESIAN_POINT ( 'NONE',  ( 5.221875000614519813, -6.054752690667223547, -1.112240025338166033E-15 ) ) ;
#50294 = CARTESIAN_POINT ( 'NONE',  ( 8.221875000614518925, 3.027376345333611329, 5.243569643749999010 ) ) ;
#50295 = EDGE_CURVE ( 'NONE', #23277, #32974, #66592, .T. ) ;
#50296 = ORIENTED_EDGE ( 'NONE', *, *, #33344, .F. ) ;
#50297 = CARTESIAN_POINT ( 'NONE',  ( 27.87187500061451573, 3.027376345333613106, -5.243569643749998122 ) ) ;
#50298 = CARTESIAN_POINT ( 'NONE',  ( 18.92812500061451431, 4.541064518000418104, 2.621784821874999949 ) ) ;
#50299 = CARTESIAN_POINT ( 'NONE',  ( 28.83750000122903145, -4.330127018922194537, 2.499999999999995559 ) ) ;
#50300 = CARTESIAN_POINT ( 'NONE',  ( 26.80312500061451431, -4.541064518000417216, -2.621784821875001281 ) ) ;
#50301 = CARTESIAN_POINT ( 'NONE',  ( 23.22187500061451715, -6.054752690667223547, -1.112240025338166033E-15 ) ) ;
#50302 = CARTESIAN_POINT ( 'NONE',  ( 20.12812500061451715, 6.421520780324663323E-16, -5.243569643749999010 ) ) ;
#50303 = CARTESIAN_POINT ( 'NONE',  ( -2.000000000000000000, 10.47500000000000142, 26.53589838486224650 ) ) ;
#50304 = CARTESIAN_POINT ( 'NONE',  ( 24.40312500061451573, 0.000000000000000000, 5.243569643749999010 ) ) ;
#50305 = CARTESIAN_POINT ( 'NONE',  ( 4.912500001229034297, 0.000000000000000000, 4.999999999999998224 ) ) ;
#50306 = ORIENTED_EDGE ( 'NONE', *, *, #46542, .F. ) ;
#50307 = CARTESIAN_POINT ( 'NONE',  ( 28.27499999999999858, -4.330127018922194537, 2.499999999999995559 ) ) ;
#50308 = CARTESIAN_POINT ( 'NONE',  ( 8.484601909799253346E-16, 15.16250000000000142, -25.38119784648299770 ) ) ;
#50309 = CARTESIAN_POINT ( 'NONE',  ( 3.756430356250000546, 16.39062499938548356, 27.83122392262697886 ) ) ;
#50310 = CARTESIAN_POINT ( 'NONE',  ( 5.334375000614517859, 6.421520780324663323E-16, -5.243569643749999010 ) ) ;
#50311 = CARTESIAN_POINT ( 'NONE',  ( 12.32812500061451821, -4.541064518000419881, 2.621784821874995952 ) ) ;
#50312 = CARTESIAN_POINT ( 'NONE',  ( 6.009375000614519458, 0.000000000000000000, 5.243569643749999010 ) ) ;
#50313 = CARTESIAN_POINT ( 'NONE',  ( 23.66250000122903430, 4.330127018922192761, -2.499999999999997780 ) ) ;
#50314 = CARTESIAN_POINT ( 'NONE',  ( 13.92187500061451289, 3.027376345333612662, -5.243569643749998122 ) ) ;
#50315 = CARTESIAN_POINT ( 'NONE',  ( 29.76562500061451644, 3.027376345333611329, 5.243569643749999010 ) ) ;
#50316 = CARTESIAN_POINT ( 'NONE',  ( 28.57499999999999929, 4.330127018922191873, 2.499999999999999556 ) ) ;
#50317 = CARTESIAN_POINT ( 'NONE',  ( 25.50937500061451502, -4.541064518000417216, -2.621784821875001281 ) ) ;
#50318 = CARTESIAN_POINT ( 'NONE',  ( 3.290625000614516793, -3.027376345333614438, 5.243569643749998122 ) ) ;
#50319 = CARTESIAN_POINT ( 'NONE',  ( 13.26562500061451644, -6.054752690667223547, -1.112240025338166033E-15 ) ) ;
#50320 = ORIENTED_EDGE ( 'NONE', *, *, #58832, .T. ) ;
#50321 = CARTESIAN_POINT ( 'NONE',  ( 10.19062500061451892, -3.027376345333610441, -5.243569643749999898 ) ) ;
#50322 = CARTESIAN_POINT ( 'NONE',  ( 9.478125000614515017, 4.541064518000418104, 2.621784821874999949 ) ) ;
#50323 = CARTESIAN_POINT ( 'NONE',  ( 19.95937500061451786, 0.000000000000000000, 4.756430356249998326 ) ) ;
#50324 = DIRECTION ( 'NONE',  ( -0.000000000000000000, -1.000000000000000000, -0.000000000000000000 ) ) ;
#50325 = CARTESIAN_POINT ( 'NONE',  ( 16.31250000000000000, 2.886751345948129099, -4.999999999999998224 ) ) ;
#50326 = CARTESIAN_POINT ( 'NONE',  ( 16.92187500061451999, -6.054752690667223547, -1.112240025338166033E-15 ) ) ;
#50327 = CARTESIAN_POINT ( 'NONE',  ( 13.23750000122903359, 6.123233995736764310E-16, -4.999999999999998224 ) ) ;
#50328 = CARTESIAN_POINT ( 'NONE',  ( 19.27500000000000213, -4.330127018922194537, 2.499999999999995559 ) ) ;
#50329 = CARTESIAN_POINT ( 'NONE',  ( 20.55937500061451573, -4.541064518000417216, -2.621784821875001281 ) ) ;
#50330 = CARTESIAN_POINT ( 'NONE',  ( -4.243569643749999898, 15.26562500061451644, -32.45002607614398471 ) ) ;
#50331 = CARTESIAN_POINT ( 'NONE',  ( 21.56250000000000000, -5.773502691896255534, -1.060575238724906372E-15 ) ) ;
#50332 = CARTESIAN_POINT ( 'NONE',  ( 25.35937500061451644, -5.492252693125287522, -1.008910452111647106E-15 ) ) ;
#50333 = CARTESIAN_POINT ( 'NONE',  ( 1.999999999999997335, 15.06874999877096677, 33.46410161513775705 ) ) ;
#50334 = CARTESIAN_POINT ( 'NONE',  ( 27.77812500061451573, 6.421520780324663323E-16, -5.243569643749999010 ) ) ;
#50335 = CARTESIAN_POINT ( 'NONE',  ( 45.00000000000000000, 6.123233995736764310E-16, -4.999999999999998224 ) ) ;
#50336 =( BOUNDED_CURVE ( )  B_SPLINE_CURVE ( 2, ( #55228, #22323, #55948, #61483, #22680, #38219, #5344 ),
 .UNSPECIFIED., .F., .F. ) 
 B_SPLINE_CURVE_WITH_KNOTS ( ( 3, 2, 2, 3 ),
 ( 0.3166666666666666519, 0.3194444444444444198, 0.3222222222222222432, 0.3250000000000000111 ),
 .UNSPECIFIED. ) 
 CURVE ( )  GEOMETRIC_REPRESENTATION_ITEM ( )  RATIONAL_B_SPLINE_CURVE ( ( 1.000000000000000000, 0.8660254037844387076, 1.000000000000000000, 0.8660254037844387076, 1.000000000000000000, 0.8660254037844387076, 1.000000000000000000 ) ) 
 REPRESENTATION_ITEM ( '' )  );
#50337 = CARTESIAN_POINT ( 'NONE',  ( 26.84999999999999787, 0.000000000000000000, 4.999999999999998224 ) ) ;
#50338 = CARTESIAN_POINT ( 'NONE',  ( 10.07812500061451644, -4.541064518000419881, 2.621784821874995952 ) ) ;
#50339 = CARTESIAN_POINT ( 'NONE',  ( 28.17187500061451289, 5.824947211148865298E-16, -4.756430356249998326 ) ) ;
#50340 = CARTESIAN_POINT ( 'NONE',  ( 20.63437500061451857, 6.421520780324663323E-16, -5.243569643749999010 ) ) ;
#50341 = CARTESIAN_POINT ( 'NONE',  ( 14.63437500061451502, -2.746126346562641984, -4.756430356249999214 ) ) ;
#50342 = CARTESIAN_POINT ( 'NONE',  ( 5.315625000614516260, 3.027376345333613106, -5.243569643749998122 ) ) ;
#50343 = CARTESIAN_POINT ( 'NONE',  ( 10.77187500061451786, 3.027376345333613106, -5.243569643749998122 ) ) ;
#50344 = VERTEX_POINT ( 'NONE', #63294 ) ;
#50345 = CARTESIAN_POINT ( 'NONE',  ( 22.35937500061451644, -4.541064518000417216, -2.621784821875001281 ) ) ;
#50346 = CARTESIAN_POINT ( 'NONE',  ( 0.1378111602261695712, 5.000000000000000000, -26.00000000000000000 ) ) ;
#50347 = CARTESIAN_POINT ( 'NONE',  ( 28.87499999999999645, 6.123233995736764310E-16, -4.999999999999998224 ) ) ;
#50348 = CARTESIAN_POINT ( 'NONE',  ( 5.737499999999998934, -2.886751345948129988, 4.999999999999997335 ) ) ;
#50349 = CARTESIAN_POINT ( 'NONE',  ( 15.52500000122903323, 2.886751345948129099, -4.999999999999998224 ) ) ;
#50350 = CARTESIAN_POINT ( 'NONE',  ( 17.25000000000000000, 4.330127018922192761, -2.499999999999997780 ) ) ;
#50351 = ORIENTED_EDGE ( 'NONE', *, *, #16407, .F. ) ;
#50352 = CARTESIAN_POINT ( 'NONE',  ( 12.67499999999999893, 6.123233995736764310E-16, -4.999999999999998224 ) ) ;
#50353 = CARTESIAN_POINT ( 'NONE',  ( 17.13749999999999929, -2.886751345948125991, -5.000000000000000000 ) ) ;
#50354 = CARTESIAN_POINT ( 'NONE',  ( 10.87500000122903288, -5.773502691896255534, -1.060575238724906372E-15 ) ) ;
#50355 = CARTESIAN_POINT ( 'NONE',  ( 9.403125000614517504, 4.541064518000418104, -2.621784821874998173 ) ) ;
#50356 = EDGE_CURVE ( 'NONE', #13938, #55464, #18028, .T. ) ;
#50357 = CARTESIAN_POINT ( 'NONE',  ( 8.062500000000000000, -5.773502691896255534, -1.060575238724906372E-15 ) ) ;
#50358 = CARTESIAN_POINT ( 'NONE',  ( 3.617702362022032325, -3.451409801779584008, 3.617702362022032325 ) ) ;
#50359 = CARTESIAN_POINT ( 'NONE',  ( -4.243569643749999898, 14.90937500061451715, -30.00000000000000000 ) ) ;
#50360 = CARTESIAN_POINT ( 'NONE',  ( 27.22500000122903430, 2.886751345948129099, -4.999999999999998224 ) ) ;
#50361 = CARTESIAN_POINT ( 'NONE',  ( 2.655984681222220721E-16, 14.55312499938548321, 25.66244784525396483 ) ) ;
#50362 = CARTESIAN_POINT ( 'NONE',  ( 6.337499999999998579, -2.886751345948125991, -5.000000000000000000 ) ) ;
#50363 = DIRECTION ( 'NONE',  ( 1.000000000000000000, 0.000000000000000000, 0.000000000000000000 ) ) ;
#50364 = ORIENTED_EDGE ( 'NONE', *, *, #48242, .T. ) ;
#50365 = CARTESIAN_POINT ( 'NONE',  ( 25.37812500061451715, -4.541064518000419881, 2.621784821874995952 ) ) ;
#50366 = CARTESIAN_POINT ( 'NONE',  ( 1.626862140677534273E-15, 13.36250000000000071, -26.00000000000000355 ) ) ;
#50367 = VECTOR ( 'NONE', #22627, 1000.000000000000000 ) ;
#50368 = CARTESIAN_POINT ( 'NONE',  ( 28.99687500061451573, -3.027376345333614438, 5.243569643749998122 ) ) ;
#50369 = CARTESIAN_POINT ( 'NONE',  ( 22.17187500061451644, 3.027376345333611329, 5.243569643749999010 ) ) ;
#50370 = CARTESIAN_POINT ( 'NONE',  ( 15.70312500061451644, 4.541064518000418104, -2.621784821874998173 ) ) ;
#50371 = CARTESIAN_POINT ( 'NONE',  ( -3.000416591977282496E-16, 12.04062500061459495, -34.90005215228797653 ) ) ;
#50372 = CARTESIAN_POINT ( 'NONE',  ( 7.415625000614516793, -6.054752690667223547, -1.112240025338166033E-15 ) ) ;
#50373 = CARTESIAN_POINT ( 'NONE',  ( 28.80000000122903003, -2.886751345948129988, 4.999999999999997335 ) ) ;
#50374 = CARTESIAN_POINT ( 'NONE',  ( 24.27187500061451786, 2.746126346562645981, -4.756430356249997438 ) ) ;
#50375 = CARTESIAN_POINT ( 'NONE',  ( 18.77812500061451573, 6.421520780324663323E-16, -5.243569643749999010 ) ) ;
#50376 = CARTESIAN_POINT ( 'NONE',  ( -3.137519842735245283E-14, 11.22500000122903430, -26.00000000000000711 ) ) ;
#50377 = CARTESIAN_POINT ( 'NONE',  ( 1.878215178125000495, 19.46562499938548640, 26.74683588394047007 ) ) ;
#50378 = CARTESIAN_POINT ( 'NONE',  ( 14.67187500061451821, -6.054752690667223547, -1.112240025338166033E-15 ) ) ;
#50379 = CARTESIAN_POINT ( 'NONE',  ( 15.53437500061451715, -4.541064518000419881, 2.621784821874995952 ) ) ;
#50380 = CARTESIAN_POINT ( 'NONE',  ( 23.14687500061451786, -3.027376345333614438, 5.243569643749998122 ) ) ;
#50381 = ORIENTED_EDGE ( 'NONE', *, *, #42162, .F. ) ;
#50382 = CARTESIAN_POINT ( 'NONE',  ( -5.810221930991193690E-16, 14.60000000122903252, -34.00000000000000000 ) ) ;
#50383 = CARTESIAN_POINT ( 'NONE',  ( 27.06562500061451004, 3.027376345333611329, 5.243569643749999010 ) ) ;
#50384 = CARTESIAN_POINT ( 'NONE',  ( 25.79062500061451502, -3.027376345333614438, 5.243569643749998122 ) ) ;
#50385 = CARTESIAN_POINT ( 'NONE',  ( 7.706250001229031810, -4.330127018922190985, -2.500000000000001332 ) ) ;
#50386 = CARTESIAN_POINT ( 'NONE',  ( 8.484601909799253346E-16, 16.51249999999999929, 34.61880215351700230 ) ) ;
#50387 = CARTESIAN_POINT ( 'NONE',  ( 4.584375000614516971, 4.541064518000418104, 2.621784821874999949 ) ) ;
#50388 = CARTESIAN_POINT ( 'NONE',  ( 11.92500000122903181, 2.886751345948129099, -4.999999999999998224 ) ) ;
#50389 = CARTESIAN_POINT ( 'NONE',  ( 6.112500001229034474, 4.330127018922192761, -2.499999999999997780 ) ) ;
#50390 = CARTESIAN_POINT ( 'NONE',  ( 2.840625000614518392, -3.027376345333614438, 5.243569643749998122 ) ) ;
#50391 = CARTESIAN_POINT ( 'NONE',  ( -4.000000000000000000, 18.96874999877096357, 30.00000000000000000 ) ) ;
#50392 = CARTESIAN_POINT ( 'NONE',  ( 18.73125000122903216, 4.330127018922191873, 2.499999999999999556 ) ) ;
#50393 = CARTESIAN_POINT ( 'NONE',  ( 11.48437500061451644, -4.541064518000419881, 2.621784821874995952 ) ) ;
#50394 = CARTESIAN_POINT ( 'NONE',  ( 29.53125000122903288, 4.330127018922191873, 2.499999999999999556 ) ) ;
#50395 = ORIENTED_EDGE ( 'NONE', *, *, #5393, .F. ) ;
#50396 = CARTESIAN_POINT ( 'NONE',  ( 19.71562500061451928, 3.027376345333613106, -5.243569643749998122 ) ) ;
#50397 = CARTESIAN_POINT ( 'NONE',  ( 13.77187500061451786, -6.054752690667223547, -1.112240025338166033E-15 ) ) ;
#50398 = CARTESIAN_POINT ( 'NONE',  ( 5.053125000614517859, 0.000000000000000000, 5.243569643749999010 ) ) ;
#50399 = CARTESIAN_POINT ( 'NONE',  ( 23.25937500061451857, -4.541064518000417216, -2.621784821875001281 ) ) ;
#50400 = CARTESIAN_POINT ( 'NONE',  ( 9.309375000614517504, -4.541064518000417216, -2.621784821875001281 ) ) ;
#50401 = CARTESIAN_POINT ( 'NONE',  ( 4.265625000614517326, -6.054752690667223547, -1.112240025338166033E-15 ) ) ;
#50402 = DIRECTION ( 'NONE',  ( 0.000000000000000000, 0.000000000000000000, 1.000000000000000000 ) ) ;
#50403 = CARTESIAN_POINT ( 'NONE',  ( 5.025000001229035895, -5.773502691896255534, -1.060575238724906372E-15 ) ) ;
#50404 =( BOUNDED_CURVE ( )  B_SPLINE_CURVE ( 2, ( #1104, #41344, #7716, #63854, #23611, #6640, #52782 ),
 .UNSPECIFIED., .F., .F. ) 
 B_SPLINE_CURVE_WITH_KNOTS ( ( 3, 2, 2, 3 ),
 ( 0.06000000000000003941, 0.06333333333333336645, 0.06666666666666667962, 0.07000000000000000666 ),
 .UNSPECIFIED. ) 
 CURVE ( )  GEOMETRIC_REPRESENTATION_ITEM ( )  RATIONAL_B_SPLINE_CURVE ( ( 0.9999999999999983347, 0.8660254037844403729, 1.000000000000000000, 0.8660254037844387076, 1.000000000000000000, 0.8660254037844387076, 1.000000000000000000 ) ) 
 REPRESENTATION_ITEM ( '' )  );
#50405 = CARTESIAN_POINT ( 'NONE',  ( 21.02812500061451573, 6.421520780324663323E-16, -5.243569643749999010 ) ) ;
#50406 = CARTESIAN_POINT ( 'NONE',  ( 7.162500001229032520, 0.000000000000000000, 4.999999999999998224 ) ) ;
#50407 = CARTESIAN_POINT ( 'NONE',  ( 17.72812500061451502, -4.541064518000419881, 2.621784821874995952 ) ) ;
#50408 = CARTESIAN_POINT ( 'NONE',  ( 16.41562500061451857, -6.054752690667223547, -1.112240025338166033E-15 ) ) ;
#50409 = CARTESIAN_POINT ( 'NONE',  ( 27.15937500061451360, 0.000000000000000000, 4.756430356249998326 ) ) ;
#50410 = CARTESIAN_POINT ( 'NONE',  ( 15.63749999999999751, -2.886751345948129988, 4.999999999999997335 ) ) ;
#50411 = CARTESIAN_POINT ( 'NONE',  ( 9.900000001229033231, -2.886751345948129988, 4.999999999999997335 ) ) ;
#50412 = CARTESIAN_POINT ( 'NONE',  ( 6.815625000614517148, 3.027376345333611329, 5.243569643749999010 ) ) ;
#50413 = ADVANCED_FACE ( 'NONE', ( #1620 ), #24129, .F. ) ;
#50414 = CARTESIAN_POINT ( 'NONE',  ( 20.47500000122903074, 2.886751345948129099, -4.999999999999998224 ) ) ;
#50415 = CARTESIAN_POINT ( 'NONE',  ( 27.07499999999999929, 6.123233995736764310E-16, -4.999999999999998224 ) ) ;
#50416 = CARTESIAN_POINT ( 'NONE',  ( -4.243569643749999898, 10.82187500061451857, -32.45002607614398471 ) ) ;
#50417 = CARTESIAN_POINT ( 'NONE',  ( 3.756430356250000102, 12.64062499938548356, 30.00000000000000000 ) ) ;
#50418 = CARTESIAN_POINT ( 'NONE',  ( 3.421875000614516882, -6.054752690667223547, -1.112240025338166033E-15 ) ) ;
#50419 = CARTESIAN_POINT ( 'NONE',  ( 21.68437500061451573, 4.541064518000418104, 2.621784821874999949 ) ) ;
#50420 = CARTESIAN_POINT ( 'NONE',  ( 5.100000000000000533, 4.330127018922192761, -2.499999999999997780 ) ) ;
#50421 = CARTESIAN_POINT ( 'NONE',  ( 15.29062500061451679, 6.054752690667223547, 3.707466751127219781E-16 ) ) ;
#50422 = CARTESIAN_POINT ( 'NONE',  ( 12.84375000122903288, 5.773502691896255534, 3.535250795749688894E-16 ) ) ;
#50423 = CARTESIAN_POINT ( 'NONE',  ( 23.09999999999999787, 4.330127018922192761, -2.499999999999997780 ) ) ;
#50424 = CARTESIAN_POINT ( 'NONE',  ( 13.96875000122903465, -5.773502691896255534, -1.060575238724906372E-15 ) ) ;
#50425 = CARTESIAN_POINT ( 'NONE',  ( 29.70937500061451431, 4.541064518000418104, -2.621784821874998173 ) ) ;
#50426 = CARTESIAN_POINT ( 'NONE',  ( 21.30937500061451217, -5.492252693125287522, -1.008910452111647106E-15 ) ) ;
#50427 = CARTESIAN_POINT ( 'NONE',  ( 11.76562500061451644, 3.027376345333611329, 5.243569643749999010 ) ) ;
#50428 = CARTESIAN_POINT ( 'NONE',  ( 11.40937500061451892, 0.000000000000000000, 5.243569643749999010 ) ) ;
#50429 = ORIENTED_EDGE ( 'NONE', *, *, #52646, .F. ) ;
#50430 = CARTESIAN_POINT ( 'NONE',  ( -1.071796769724491005, 14.05759618943233669, -34.00000000000000000 ) ) ;
#50431 = CARTESIAN_POINT ( 'NONE',  ( 22.64062500061451644, -3.027376345333614438, 5.243569643749998122 ) ) ;
#50432 = CARTESIAN_POINT ( 'NONE',  ( 1.999999999999998668, 13.21250000122903501, -33.46410161513775705 ) ) ;
#50433 = ADVANCED_FACE ( 'NONE', ( #17850 ), #62929, .T. ) ;
#50434 = CARTESIAN_POINT ( 'NONE',  ( 20.54999999999999716, 0.000000000000000000, 4.999999999999998224 ) ) ;
#50435 = CARTESIAN_POINT ( 'NONE',  ( 12.93750000000000178, -2.886751345948129988, 4.999999999999997335 ) ) ;
#50436 = CARTESIAN_POINT ( 'NONE',  ( 21.97500000122903074, 2.886751345948126879, 4.999999999999999112 ) ) ;
#50437 = CARTESIAN_POINT ( 'NONE',  ( 17.31562500061451715, -6.054752690667223547, -1.112240025338166033E-15 ) ) ;
#50438 = CARTESIAN_POINT ( 'NONE',  ( 13.69687500061451679, -4.119189519843965641, -2.378215178125001383 ) ) ;
#50439 = VERTEX_POINT ( 'NONE', #70299 ) ;
#50440 = CARTESIAN_POINT ( 'NONE',  ( 19.27500000000000213, -4.330127018922194537, 2.499999999999995559 ) ) ;
#50441 = CARTESIAN_POINT ( 'NONE',  ( 23.66250000000000142, 2.886751345948126879, 4.999999999999999112 ) ) ;
#50442 = CARTESIAN_POINT ( 'NONE',  ( 20.44687500061451857, -3.027376345333614438, 5.243569643749998122 ) ) ;
#50443 = CARTESIAN_POINT ( 'NONE',  ( 26.50312500061451360, 4.541064518000418104, -2.621784821874998173 ) ) ;
#50444 = ORIENTED_EDGE ( 'NONE', *, *, #23135, .F. ) ;
#50445 = CARTESIAN_POINT ( 'NONE',  ( 45.00000000000000000, 7.332543590861163807, 5.218601775200022885 ) ) ;
#50446 = CARTESIAN_POINT ( 'NONE',  ( 7.865625000614516971, -6.054752690667223547, -1.112240025338166033E-15 ) ) ;
#50447 = CARTESIAN_POINT ( 'NONE',  ( 17.36250000122903359, 4.330127018922192761, -2.499999999999997780 ) ) ;
#50448 = CARTESIAN_POINT ( 'NONE',  ( 18.18750000000000000, 5.773502691896255534, 3.535250795749688894E-16 ) ) ;
#50449 = CARTESIAN_POINT ( 'NONE',  ( 4.209375000614516971, 0.000000000000000000, 5.243569643749999010 ) ) ;
#50450 = CARTESIAN_POINT ( 'NONE',  ( 29.63437500061451502, 6.421520780324663323E-16, -5.243569643749999010 ) ) ;
#50451 = VERTEX_POINT ( 'NONE', #3067 ) ;
#50452 = CARTESIAN_POINT ( 'NONE',  ( 23.95312500061451289, 0.000000000000000000, 5.243569643749999010 ) ) ;
#50453 = CARTESIAN_POINT ( 'NONE',  ( 25.65937500061451715, 4.541064518000418104, -2.621784821874998173 ) ) ;
#50454 = CARTESIAN_POINT ( 'NONE',  ( -2.121784821874996840, 18.52812500061459389, -26.32496088578401583 ) ) ;
#50455 = CARTESIAN_POINT ( 'NONE',  ( 12.52500000000000213, -4.330127018922194537, 2.499999999999995559 ) ) ;
#50456 = CARTESIAN_POINT ( 'NONE',  ( 8.765625000614518214, -6.054752690667223547, -1.112240025338166033E-15 ) ) ;
#50457 = CARTESIAN_POINT ( 'NONE',  ( 30.00000000000000000, 0.000000000000000000, 4.999999999999998224 ) ) ;
#50458 = CARTESIAN_POINT ( 'NONE',  ( 25.52812500061451573, 6.421520780324663323E-16, -5.243569643749999010 ) ) ;
#50459 = CARTESIAN_POINT ( 'NONE',  ( 29.63437500061451857, 5.492252693125287522, 3.363034840372157021E-16 ) ) ;
#50460 = CARTESIAN_POINT ( 'NONE',  ( 14.40937500061451715, 4.119189519843966529, -2.378215178124998275 ) ) ;
#50461 = CARTESIAN_POINT ( 'NONE',  ( 3.965625000614515727, 3.027376345333613106, -5.243569643749998122 ) ) ;
#50462 = CARTESIAN_POINT ( 'NONE',  ( 19.32187500061451857, 3.027376345333613106, -5.243569643749998122 ) ) ;
#50463 = CARTESIAN_POINT ( 'NONE',  ( 4.243569643749999010, 15.62187500061451928, 27.54997392385601174 ) ) ;
#50464 = CARTESIAN_POINT ( 'NONE',  ( 22.13437500061451502, 4.541064518000418104, 2.621784821874999949 ) ) ;
#50466 = EDGE_CURVE ( 'NONE', #23337, #59218, #62038, .T. ) ;
#50465 = CARTESIAN_POINT ( 'NONE',  ( 3.374999999999999556, 4.330127018922191873, 2.499999999999999556 ) ) ;
#50467 = CARTESIAN_POINT ( 'NONE',  ( 10.22812500061451679, 6.421520780324663323E-16, -5.243569643749999010 ) ) ;
#50468 = CARTESIAN_POINT ( 'NONE',  ( 1.592000809091587073E-14, 15.05000000122903714, 26.00000000000000000 ) ) ;
#50469 = CARTESIAN_POINT ( 'NONE',  ( 7.471875000614519813, -6.054752690667223547, -1.112240025338166033E-15 ) ) ;
#50470 = CARTESIAN_POINT ( 'NONE',  ( 7.462500001229035007, 4.330127018922192761, -2.499999999999997780 ) ) ;
#50471 = CARTESIAN_POINT ( 'NONE',  ( 7.003125000614518036, -4.541064518000417216, -2.621784821875001281 ) ) ;
#50472 = CARTESIAN_POINT ( 'NONE',  ( 12.90937500061451537, -4.541064518000417216, -2.621784821875001281 ) ) ;
#50473 =( LENGTH_UNIT ( ) NAMED_UNIT ( * ) SI_UNIT ( .MILLI., .METRE. ) );
#50474 = CARTESIAN_POINT ( 'NONE',  ( 19.01250000122903216, -4.330127018922190985, -2.500000000000001332 ) ) ;
#50475 = CARTESIAN_POINT ( 'NONE',  ( 8.559375000614515727, 4.541064518000418104, -2.621784821874998173 ) ) ;
#50476 = CARTESIAN_POINT ( 'NONE',  ( 9.328125000614518214, 6.421520780324663323E-16, -5.243569643749999010 ) ) ;
#50477 = CARTESIAN_POINT ( 'NONE',  ( 4.978125000614518569, 4.541064518000418104, 2.621784821874999949 ) ) ;
#50478 = CARTESIAN_POINT ( 'NONE',  ( 25.63125000122903074, -4.330127018922194537, 2.499999999999995559 ) ) ;
#50479 = CARTESIAN_POINT ( 'NONE',  ( 18.19687500061451502, -3.027376345333614438, 5.243569643749998122 ) ) ;
#50480 = CARTESIAN_POINT ( 'NONE',  ( 0.000000000000000000, 4.999999999999998224, 0.000000000000000000 ) ) ;
#50481 = CARTESIAN_POINT ( 'NONE',  ( 27.40312500061451573, 4.541064518000418104, -2.621784821874998173 ) ) ;
#50482 = CARTESIAN_POINT ( 'NONE',  ( 11.09062500061451573, -3.027376345333610441, -5.243569643749999898 ) ) ;
#50483 = AXIS2_PLACEMENT_3D ( 'NONE', #5472, #12458, #67535 ) ;
#50484 = CARTESIAN_POINT ( 'NONE',  ( 28.88437500061451502, 4.541064518000418104, 2.621784821874999949 ) ) ;
#50485 = CARTESIAN_POINT ( 'NONE',  ( 2.121784821875001281, 12.35937500061451821, -26.32496088578401938 ) ) ;
#50486 = CARTESIAN_POINT ( 'NONE',  ( 13.46250000122903323, 0.000000000000000000, 4.999999999999998224 ) ) ;
#50487 = CARTESIAN_POINT ( 'NONE',  ( 27.55312500061451786, 0.000000000000000000, 5.243569643749999010 ) ) ;
#50488 = CARTESIAN_POINT ( 'NONE',  ( 4.243569643749999898, 15.52812500061451750, -30.00000000000000000 ) ) ;
#50489 = CARTESIAN_POINT ( 'NONE',  ( 14.21250000122903323, 4.330127018922192761, -2.499999999999997780 ) ) ;
#50490 = CARTESIAN_POINT ( 'NONE',  ( 12.48750000000000249, -2.886751345948129988, 4.999999999999997335 ) ) ;
#50491 = CARTESIAN_POINT ( 'NONE',  ( -1.071796769724488563, 13.79240381056766829, 34.00000000000000000 ) ) ;
#50492 = CARTESIAN_POINT ( 'NONE',  ( 22.94062500061451715, 6.054752690667223547, 3.707466751127219781E-16 ) ) ;
#50493 = CARTESIAN_POINT ( 'NONE',  ( 7.284375000614518036, 4.541064518000418104, 2.621784821874999949 ) ) ;
#50494 = CARTESIAN_POINT ( 'NONE',  ( 8.137500001229033941, -4.330127018922194537, 2.499999999999995559 ) ) ;
#50495 = CARTESIAN_POINT ( 'NONE',  ( 15.00000000122903465, -2.886751345948125991, -5.000000000000000000 ) ) ;
#50496 = CARTESIAN_POINT ( 'NONE',  ( 13.60312500061451679, 0.000000000000000000, 5.243569643749999010 ) ) ;
#50497 = CARTESIAN_POINT ( 'NONE',  ( 19.26562500061451644, 3.027376345333613106, -5.243569643749998122 ) ) ;
#50498 = CARTESIAN_POINT ( 'NONE',  ( 25.27500000122903145, -5.773502691896255534, -1.060575238724906372E-15 ) ) ;
#50499 = CARTESIAN_POINT ( 'NONE',  ( 28.05000000122903359, -2.886751345948125991, -5.000000000000000000 ) ) ;
#50500 = CARTESIAN_POINT ( 'NONE',  ( 23.58749999999999858, 5.773502691896255534, 3.535250795749688894E-16 ) ) ;
#50501 = CARTESIAN_POINT ( 'NONE',  ( 24.98437500061451644, -4.541064518000419881, 2.621784821874995952 ) ) ;
#50502 = CARTESIAN_POINT ( 'NONE',  ( 1.071796769724491893, 13.75759618943233420, 34.00000000000000000 ) ) ;
#50503 = CARTESIAN_POINT ( 'NONE',  ( 10.83750000122903501, -4.330127018922194537, 2.499999999999995559 ) ) ;
#50504 = CARTESIAN_POINT ( 'NONE',  ( 26.89687500061451431, -3.027376345333610441, -5.243569643749999898 ) ) ;
#50505 = EDGE_CURVE ( 'NONE', #30573, #59457, #1012, .T. ) ;
#50506 = CARTESIAN_POINT ( 'NONE',  ( 13.91250000000000142, -5.773502691896255534, -1.060575238724906372E-15 ) ) ;
#50507 = CARTESIAN_POINT ( 'NONE',  ( 5.371875000614516615, 3.027376345333613106, -5.243569643749998122 ) ) ;
#50508 = CARTESIAN_POINT ( 'NONE',  ( 22.97812500061451857, 4.541064518000418104, 2.621784821874999949 ) ) ;
#50509 = CARTESIAN_POINT ( 'NONE',  ( 3.756430356250000102, 15.00312499938548427, 30.00000000000000000 ) ) ;
#50510 = CARTESIAN_POINT ( 'NONE',  ( -1.071796769724486120, 15.46115380933863293, 34.00000000000000000 ) ) ;
#50511 = CARTESIAN_POINT ( 'NONE',  ( 10.58437500061451964, -4.541064518000419881, 2.621784821874995952 ) ) ;
#50512 = LINE ( 'NONE', #46054, #72589 ) ;
#50513 = CARTESIAN_POINT ( 'NONE',  ( 29.80312500061451431, 0.000000000000000000, 5.243569643749999010 ) ) ;
#50514 = CARTESIAN_POINT ( 'NONE',  ( 5.746875000614517504, -3.027376345333610441, -5.243569643749999898 ) ) ;
#50515 = CARTESIAN_POINT ( 'NONE',  ( 27.57187500061451857, 3.027376345333611329, 5.243569643749999010 ) ) ;
#50516 = CARTESIAN_POINT ( 'NONE',  ( 4.243569643749999010, 10.16562500061459495, 27.54997392385601174 ) ) ;
#50517 = CARTESIAN_POINT ( 'NONE',  ( 19.42499999999999716, 6.123233995736764310E-16, -4.999999999999998224 ) ) ;
#50518 = VERTEX_POINT ( 'NONE', #43330 ) ;
#50519 = CARTESIAN_POINT ( 'NONE',  ( 27.78749999999999787, -2.886751345948129988, 4.999999999999997335 ) ) ;
#50520 = CARTESIAN_POINT ( 'NONE',  ( 29.22187500061451715, 3.027376345333613106, -5.243569643749998122 ) ) ;
#50521 = VERTEX_POINT ( 'NONE', #8976 ) ;
#50522 = CARTESIAN_POINT ( 'NONE',  ( 15.14062500061451644, -3.027376345333610441, -5.243569643749999898 ) ) ;
#50523 = CARTESIAN_POINT ( 'NONE',  ( 9.328125000614518214, 6.421520780324663323E-16, -5.243569643749999010 ) ) ;
#50524 = CARTESIAN_POINT ( 'NONE',  ( 20.78437500061451360, -2.746126346562646425, 4.756430356249996549 ) ) ;
#50525 = CARTESIAN_POINT ( 'NONE',  ( 3.609375000614516882, 4.541064518000418104, -2.621784821874998173 ) ) ;
#50526 = CARTESIAN_POINT ( 'NONE',  ( 18.67500000122903714, 2.886751345948129099, -4.999999999999998224 ) ) ;
#50527 = CARTESIAN_POINT ( 'NONE',  ( 24.14999999999999858, 0.000000000000000000, 4.999999999999998224 ) ) ;
#50528 = CARTESIAN_POINT ( 'NONE',  ( 1.071796769724488785, 19.60759618943233562, 34.00000000000000000 ) ) ;
#50529 = CARTESIAN_POINT ( 'NONE',  ( 7.021875000614518747, -6.054752690667223547, -1.112240025338166033E-15 ) ) ;
#50530 = CARTESIAN_POINT ( 'NONE',  ( 10.73437500061451644, 6.421520780324663323E-16, -5.243569643749999010 ) ) ;
#50531 = CARTESIAN_POINT ( 'NONE',  ( 21.94687500061451857, -3.027376345333610441, -5.243569643749999898 ) ) ;
#50532 = CARTESIAN_POINT ( 'NONE',  ( 1.626862140677534273E-15, 11.11250000000000071, 34.00000000000000000 ) ) ;
#50533 = ORIENTED_EDGE ( 'NONE', *, *, #64551, .F. ) ;
#50534 = CARTESIAN_POINT ( 'NONE',  ( 4.246875000614519280, -3.027376345333614438, 5.243569643749998122 ) ) ;
#50535 = CARTESIAN_POINT ( 'NONE',  ( 10.35000000000000142, -4.330127018922190985, -2.500000000000001332 ) ) ;
#50536 = CARTESIAN_POINT ( 'NONE',  ( 6.721875000614518925, 3.027376345333613106, -5.243569643749998122 ) ) ;
#50537 = CARTESIAN_POINT ( 'NONE',  ( 21.75000000000000000, 4.330127018922192761, -2.499999999999997780 ) ) ;
#50538 = CARTESIAN_POINT ( 'NONE',  ( 15.44062500061451537, -3.027376345333614438, 5.243569643749998122 ) ) ;
#50539 = CARTESIAN_POINT ( 'NONE',  ( -8.484601909799255319E-16, 18.23750000000000071, 34.61880215351700940 ) ) ;
#50540 = CARTESIAN_POINT ( 'NONE',  ( -3.999999999999999112, 19.96250000000000213, 27.69059892324149885 ) ) ;
#50541 = CARTESIAN_POINT ( 'NONE',  ( 22.20937500061451431, 0.000000000000000000, 4.756430356249998326 ) ) ;
#50542 = CARTESIAN_POINT ( 'NONE',  ( 8.878125000614515372, 6.421520780324663323E-16, -5.243569643749999010 ) ) ;
#50543 = CARTESIAN_POINT ( 'NONE',  ( 27.30937500061451573, -4.541064518000417216, -2.621784821875001281 ) ) ;
#50544 = CARTESIAN_POINT ( 'NONE',  ( 12.78749999999999787, 5.773502691896255534, 3.535250795749688401E-16 ) ) ;
#50545 = CARTESIAN_POINT ( 'NONE',  ( 28.62187500061451573, -6.054752690667223547, -1.112240025338166033E-15 ) ) ;
#50546 = CARTESIAN_POINT ( 'NONE',  ( 9.074999999999999289, 6.123233995736764310E-16, -4.999999999999998224 ) ) ;
#50547 = CARTESIAN_POINT ( 'NONE',  ( -3.999999999999999556, 14.67500000122903536, 27.69059892324149530 ) ) ;
#50548 = CARTESIAN_POINT ( 'NONE',  ( 9.300000001229035362, 5.773502691896255534, 3.535250795749688894E-16 ) ) ;
#50549 = CARTESIAN_POINT ( 'NONE',  ( 19.02187500061451786, 3.027376345333611329, 5.243569643749999010 ) ) ;
#50550 = CARTESIAN_POINT ( 'NONE',  ( 13.47187500061451537, 3.027376345333613106, -5.243569643749998122 ) ) ;
#50551 = CARTESIAN_POINT ( 'NONE',  ( 9.262500001229033941, 4.330127018922192761, -2.499999999999997780 ) ) ;
#50552 = ORIENTED_EDGE ( 'NONE', *, *, #24944, .T. ) ;
#50553 = CARTESIAN_POINT ( 'NONE',  ( 13.82812500061451466, 6.421520780324663323E-16, -5.243569643749999010 ) ) ;
#50554 = CARTESIAN_POINT ( 'NONE',  ( 25.68750000122903288, -4.330127018922194537, 2.499999999999995559 ) ) ;
#50555 = CARTESIAN_POINT ( 'NONE',  ( 15.30937500061451750, 4.541064518000418104, -2.621784821874998173 ) ) ;
#50556 = CARTESIAN_POINT ( 'NONE',  ( 2.154264117376507581, 9.766972526336937577, -24.39663440989477294 ) ) ;
#50557 = CARTESIAN_POINT ( 'NONE',  ( 17.24062500061451786, -3.027376345333614438, 5.243569643749998122 ) ) ;
#50558 = DIRECTION ( 'NONE',  ( -0.000000000000000000, 6.195440985631455317E-17, 1.000000000000000000 ) ) ;
#50559 = EDGE_CURVE ( 'NONE', #53550, #33928, #33911, .T. ) ;
#50560 = CARTESIAN_POINT ( 'NONE',  ( 26.63437500061451857, 4.541064518000418104, 2.621784821874999949 ) ) ;
#50561 = CARTESIAN_POINT ( 'NONE',  ( -3.000416591977282496E-16, 11.14062500061451644, 25.09994784771203058 ) ) ;
#50562 = CARTESIAN_POINT ( 'NONE',  ( 14.67187500061451821, -6.054752690667223547, -1.112240025338166033E-15 ) ) ;
#50563 = CARTESIAN_POINT ( 'NONE',  ( 15.03750000122903252, 6.123233995736764310E-16, -4.999999999999998224 ) ) ;
#50564 = CARTESIAN_POINT ( 'NONE',  ( 7.996875000614519280, -2.746126346562641984, -4.756430356249999214 ) ) ;
#50565 = CARTESIAN_POINT ( 'NONE',  ( 4.243569643749999010, 19.22187500061452070, -32.45002607614398471 ) ) ;
#50566 = CARTESIAN_POINT ( 'NONE',  ( 21.42187500061451644, -6.054752690667223547, -1.112240025338166033E-15 ) ) ;
#50567 = CARTESIAN_POINT ( 'NONE',  ( 21.26250000122903572, -4.330127018922190985, -2.500000000000001332 ) ) ;
#50568 = CARTESIAN_POINT ( 'NONE',  ( 13.73437500061451821, -4.541064518000419881, 2.621784821874995952 ) ) ;
#50569 = CARTESIAN_POINT ( 'NONE',  ( -4.243569643749999898, 11.75937500061451857, 30.00000000000000000 ) ) ;
#50570 = CARTESIAN_POINT ( 'NONE',  ( 21.90000000122903145, 5.773502691896255534, 3.535250795749688894E-16 ) ) ;
#50571 = CARTESIAN_POINT ( 'NONE',  ( 16.34062500061451573, -3.027376345333614438, 5.243569643749998122 ) ) ;
#50572 = EDGE_LOOP ( 'NONE', ( #71713, #66317, #64277, #20882 ) ) ;
#50573 = VERTEX_POINT ( 'NONE', #31133 ) ;
#50574 = CARTESIAN_POINT ( 'NONE',  ( 21.22500000000000142, 6.123233995736764310E-16, -4.999999999999998224 ) ) ;
#50575 = CARTESIAN_POINT ( 'NONE',  ( 45.00000000000000000, 0.000000000000000000, 0.000000000000000000 ) ) ;
#50576 = CARTESIAN_POINT ( 'NONE',  ( 25.34062500061451217, -3.027376345333614438, 5.243569643749998122 ) ) ;
#50577 = CARTESIAN_POINT ( 'NONE',  ( 2.679675080847534030, 4.226630133448147753, 32.98013821123856104 ) ) ;
#50578 = CARTESIAN_POINT ( 'NONE',  ( 17.92500000122903359, 2.886751345948126879, 4.999999999999999112 ) ) ;
#50579 = CARTESIAN_POINT ( 'NONE',  ( 23.42812500061451786, 4.541064518000418104, 2.621784821874999949 ) ) ;
#50580 = CARTESIAN_POINT ( 'NONE',  ( 24.51562500061451289, -6.054752690667223547, -1.112240025338166033E-15 ) ) ;
#50581 = CARTESIAN_POINT ( 'NONE',  ( 5.840625000614516615, 6.054752690667223547, 3.707466751127219781E-16 ) ) ;
#50582 = EDGE_LOOP ( 'NONE', ( #49133, #1276, #644, #34246 ) ) ;
#50583 = CARTESIAN_POINT ( 'NONE',  ( 29.13749999999999929, -2.886751345948129988, 4.999999999999997335 ) ) ;
#50584 = CARTESIAN_POINT ( 'NONE',  ( 2.878125000614517592, -4.541064518000419881, 2.621784821874995952 ) ) ;
#50585 = CARTESIAN_POINT ( 'NONE',  ( 11.48437500061451644, -4.119189519843968306, 2.378215178124996054 ) ) ;
#50586 = DIRECTION ( 'NONE',  ( 0.000000000000000000, 0.000000000000000000, -1.000000000000000000 ) ) ;
#50587 = CARTESIAN_POINT ( 'NONE',  ( -3.999999999999997335, 11.15000000122903323, -27.69059892324149175 ) ) ;
#50588 = CARTESIAN_POINT ( 'NONE',  ( -4.243569643749999898, 18.05937500061451928, -30.00000000000000000 ) ) ;
#50589 =( BOUNDED_CURVE ( )  B_SPLINE_CURVE ( 2, ( #15979, #5641, #107, #45164, #67695, #5995, #28525, #35152, #46242 ),
 .UNSPECIFIED., .F., .F. ) 
 B_SPLINE_CURVE_WITH_KNOTS ( ( 3, 2, 2, 2, 3 ),
 ( 0.7065217391304348116, 0.7101449275362319291, 0.7173913043478260532, 0.7246376811594202882, 0.7282608695652174058 ),
 .UNSPECIFIED. ) 
 CURVE ( )  GEOMETRIC_REPRESENTATION_ITEM ( )  RATIONAL_B_SPLINE_CURVE ( ( 0.9330127018922194093, 0.9330127018922194093, 1.000000000000000000, 0.8660254037844387076, 1.000000000000000000, 0.8660254037844387076, 1.000000000000000000, 0.9330127018922194093, 0.9330127018922194093 ) ) 
 REPRESENTATION_ITEM ( '' )  );
#50590 = EDGE_CURVE ( 'NONE', #40294, #10190, #23649, .T. ) ;
#50591 = CARTESIAN_POINT ( 'NONE',  ( 7.500000000000000000, 0.000000000000000000, 4.999999999999998224 ) ) ;
#50592 = CARTESIAN_POINT ( 'NONE',  ( 4.800000001229032698, 5.773502691896255534, 3.535250795749688894E-16 ) ) ;
#50593 = CARTESIAN_POINT ( 'NONE',  ( 11.55937500061451928, -4.541064518000417216, -2.621784821875001281 ) ) ;
#50594 = CARTESIAN_POINT ( 'NONE',  ( 23.77500000122902790, 2.886751345948161074, 4.999999999999941380 ) ) ;
#50595 = CARTESIAN_POINT ( 'NONE',  ( 3.796875000614517326, -3.027376345333614438, 5.243569643749998122 ) ) ;
#50596 = CARTESIAN_POINT ( 'NONE',  ( 29.58750000122903501, 4.330127018922191873, 2.499999999999999556 ) ) ;
#50597 = CARTESIAN_POINT ( 'NONE',  ( 10.73437500061451644, 6.421520780324663323E-16, -5.243569643749999010 ) ) ;
#50598 = CARTESIAN_POINT ( 'NONE',  ( 4.000000000000000000, 12.50000000000000000, 30.00000000000000000 ) ) ;
#50599 = CARTESIAN_POINT ( 'NONE',  ( 19.34062500061451573, 6.054752690667223547, 3.707466751127219781E-16 ) ) ;
#50600 = CARTESIAN_POINT ( 'NONE',  ( -2.121784821874996840, 17.62812500061459176, 33.67503911421598417 ) ) ;
#50601 = CARTESIAN_POINT ( 'NONE',  ( 22.47187500061451715, 3.027376345333613106, -5.243569643749998122 ) ) ;
#50602 = CYLINDRICAL_SURFACE ( 'NONE', #2511, 4.999999999999998224 ) ;
#50603 =( BOUNDED_CURVE ( )  B_SPLINE_CURVE ( 2, ( #52188, #1590, #18180, #24100, #41113, #40749, #51107 ),
 .UNSPECIFIED., .F., .F. ) 
 B_SPLINE_CURVE_WITH_KNOTS ( ( 3, 2, 2, 3 ),
 ( 0.3800000000000000044, 0.3833333333333333592, 0.3866666666666666585, 0.3900000000000000133 ),
 .UNSPECIFIED. ) 
 CURVE ( )  GEOMETRIC_REPRESENTATION_ITEM ( )  RATIONAL_B_SPLINE_CURVE ( ( 1.000000000000000000, 0.8660254037844387076, 1.000000000000000000, 0.8660254037844387076, 1.000000000000000000, 0.8660254037844387076, 1.000000000000000000 ) ) 
 REPRESENTATION_ITEM ( '' )  );
#50604 = CARTESIAN_POINT ( 'NONE',  ( 28.35000000122903430, -2.886751345948129988, 4.999999999999997335 ) ) ;
#50605 = CARTESIAN_POINT ( 'NONE',  ( 19.62187500061451573, 5.824947211148865298E-16, -4.756430356249998326 ) ) ;
#50606 = CARTESIAN_POINT ( 'NONE',  ( 25.30312500061451431, 0.000000000000000000, 5.243569643749999010 ) ) ;
#50607 = CARTESIAN_POINT ( 'NONE',  ( 14.76562500061451821, 3.027376345333613106, -5.243569643749998122 ) ) ;
#50608 = CARTESIAN_POINT ( 'NONE',  ( 15.24375000122903323, -2.886751345948129988, 4.999999999999997335 ) ) ;
#50609 = CARTESIAN_POINT ( 'NONE',  ( 12.30937500061451573, 0.000000000000000000, 5.243569643749999010 ) ) ;
#50610 = CARTESIAN_POINT ( 'NONE',  ( 28.16249999999999787, 2.886751345948126879, 4.999999999999999112 ) ) ;
#50611 = CARTESIAN_POINT ( 'NONE',  ( 26.06250000122903288, 0.000000000000000000, 4.999999999999998224 ) ) ;
#50612 = CYLINDRICAL_SURFACE ( 'NONE', #8392, 4.000000000000000000 ) ;
#50613 = CARTESIAN_POINT ( 'NONE',  ( 14.52187500061451608, 3.027376345333611329, 5.243569643749999010 ) ) ;
#50614 = CARTESIAN_POINT ( 'NONE',  ( 28.73437500061451644, 6.421520780324663323E-16, -5.243569643749999010 ) ) ;
#50615 = DIRECTION ( 'NONE',  ( -1.000000000000000000, -0.000000000000000000, -0.000000000000000000 ) ) ;
#50616 = CARTESIAN_POINT ( 'NONE',  ( 15.80625000122903145, -4.330127018922190985, -2.500000000000001332 ) ) ;
#50617 = CARTESIAN_POINT ( 'NONE',  ( 24.30937500061451573, 4.541064518000418104, -2.621784821874998173 ) ) ;
#50618 = CARTESIAN_POINT ( 'NONE',  ( 15.00937500061451679, 0.000000000000000000, 5.243569643749999010 ) ) ;
#50619 = CARTESIAN_POINT ( 'NONE',  ( -3.756430356249999214, 16.54062499938548569, 27.83122392262697531 ) ) ;
#50620 = CARTESIAN_POINT ( 'NONE',  ( 28.27499999999999858, -4.330127018922194537, 2.499999999999995559 ) ) ;
#50621 = CARTESIAN_POINT ( 'NONE',  ( 3.375000001229033320, 2.886751345948129099, -4.999999999999998224 ) ) ;
#50622 = CARTESIAN_POINT ( 'NONE',  ( 7.471875000614514484, 5.824947211148865298E-16, -4.756430356249998326 ) ) ;
#50623 = CARTESIAN_POINT ( 'NONE',  ( 18.36562500061451431, 3.027376345333613106, -5.243569643749998122 ) ) ;
#50624 = CARTESIAN_POINT ( 'NONE',  ( 8.362500000000002487, 2.886751345948126879, 4.999999999999999112 ) ) ;
#50625 = CARTESIAN_POINT ( 'NONE',  ( 0.000000000000000000, 20.00000000000000000, -30.00000000000000000 ) ) ;
#50626 = CARTESIAN_POINT ( 'NONE',  ( 16.12500000000000000, -4.330127018922194537, 2.499999999999995559 ) ) ;
#50627 = CARTESIAN_POINT ( 'NONE',  ( 4.243569643749999898, 13.72812500061451679, 30.00000000000000000 ) ) ;
#50628 = B_SPLINE_CURVE_WITH_KNOTS ( 'NONE', 3,
 ( #56118, #39864, #5510, #23207, #68296, #57186, #50936, #28048, #17656, #23574, #50577, #40216, #332, #29129, #22842, #73104, #46119, #63096, #12497, #45036, #67571, #16936, #39491, #45394, #67930, #62376, #70467, #25023, #2865, #70095, #69736, #64182, #69019, #40949, #30211, #31304, #46481, #8403 ),
 .UNSPECIFIED., .F., .F.,
 ( 4, 2, 2, 2, 2, 2, 2, 2, 2, 2, 2, 2, 2, 2, 2, 2, 2, 2, 4 ),
 ( 0.01305910913008846361, 0.01347211191627388852, 0.01388511470245931169, 0.01471112027483015630, 0.01553712584720099918, 0.01636313141957184206, 0.01801514256431353128, 0.01884114813668436722, 0.01925415092286978519, 0.01966715370905520316, 0.02008015649524062113, 0.02049315928142603910, 0.02131916485379688891, 0.02214517042616773179, 0.02297117599853857467, 0.02379718157090942449, 0.02462318714328026736, 0.02544919271565111371, 0.02627519828802195659 ),
 .UNSPECIFIED. ) ;
#50629 = CARTESIAN_POINT ( 'NONE',  ( 20.92500000122903714, 2.886751345948129099, -4.999999999999998224 ) ) ;
#50630 = CARTESIAN_POINT ( 'NONE',  ( 5.789369777004291784, 8.154036291478783838, 31.58818119731339635 ) ) ;
#50631 =( BOUNDED_CURVE ( )  B_SPLINE_CURVE ( 2, ( #5875, #28408, #43591, #66113, #38404, #15492, #55036 ),
 .UNSPECIFIED., .F., .F. ) 
 B_SPLINE_CURVE_WITH_KNOTS ( ( 3, 2, 2, 3 ),
 ( 0.6833333333333333481, 0.6861111111111111160, 0.6888888888888888840, 0.6916666666666666519 ),
 .UNSPECIFIED. ) 
 CURVE ( )  GEOMETRIC_REPRESENTATION_ITEM ( )  RATIONAL_B_SPLINE_CURVE ( ( 1.000000000000000000, 0.8660254037844387076, 1.000000000000000000, 0.8660254037844387076, 1.000000000000000000, 0.8660254037844387076, 1.000000000000000000 ) ) 
 REPRESENTATION_ITEM ( '' )  );
#50632 = CARTESIAN_POINT ( 'NONE',  ( 27.57187500061451857, 3.027376345333611329, 5.243569643749999010 ) ) ;
#50633 = ORIENTED_EDGE ( 'NONE', *, *, #16791, .T. ) ;
#50634 = CARTESIAN_POINT ( 'NONE',  ( 14.99062500061451786, -3.027376345333614438, 5.243569643749998122 ) ) ;
#50635 = CARTESIAN_POINT ( 'NONE',  ( 22.67812500061451431, -4.541064518000419881, 2.621784821874995952 ) ) ;
#50636 = CARTESIAN_POINT ( 'NONE',  ( 21.83437500061451786, -4.541064518000419881, 2.621784821874995952 ) ) ;
#50637 = CARTESIAN_POINT ( 'NONE',  ( 6.712500000000000355, -5.773502691896255534, -1.060575238724906372E-15 ) ) ;
#50638 = CARTESIAN_POINT ( 'NONE',  ( 9.853125000614516793, 4.541064518000418104, -2.621784821874998173 ) ) ;
#50639 = CARTESIAN_POINT ( 'NONE',  ( 24.25312500061451715, 4.541064518000418104, -2.621784821874998173 ) ) ;
#50640 = CARTESIAN_POINT ( 'NONE',  ( 14.14687500061451786, -3.027376345333614438, 5.243569643749998122 ) ) ;
#50641 = CARTESIAN_POINT ( 'NONE',  ( 18.15937500061451715, 0.000000000000000000, 5.243569643749999010 ) ) ;
#50642 = CARTESIAN_POINT ( 'NONE',  ( 15.48750000122903359, 6.123233995736764310E-16, -4.999999999999998224 ) ) ;
#50643 = CARTESIAN_POINT ( 'NONE',  ( 9.001249775931846008E-16, 18.56562500061451715, 34.90005215228797653 ) ) ;
#50644 = CARTESIAN_POINT ( 'NONE',  ( 21.93750000122903288, 4.330127018922191873, 2.499999999999999556 ) ) ;
#50645 = CARTESIAN_POINT ( 'NONE',  ( 14.14687500061451786, -2.746126346562646425, 4.756430356249996549 ) ) ;
#50646 = CARTESIAN_POINT ( 'NONE',  ( 12.81562500061451537, -6.054752690667223547, -1.112240025338166033E-15 ) ) ;
#50647 = CARTESIAN_POINT ( 'NONE',  ( 6.609375000614519102, -4.541064518000417216, -2.621784821875001281 ) ) ;
#50648 = CARTESIAN_POINT ( 'NONE',  ( 5.634375000614519458, -4.541064518000419881, 2.621784821874995952 ) ) ;
#50649 = ORIENTED_EDGE ( 'NONE', *, *, #22559, .F. ) ;
#50650 = CARTESIAN_POINT ( 'NONE',  ( 26.93437500061451573, 6.421520780324663323E-16, -5.243569643749999010 ) ) ;
#50651 = CARTESIAN_POINT ( 'NONE',  ( 19.45312500061451644, 0.000000000000000000, 5.243569643749999010 ) ) ;
#50652 = CARTESIAN_POINT ( 'NONE',  ( 27.48750000122903359, -4.330127018922194537, 2.499999999999995559 ) ) ;
#50653 = CARTESIAN_POINT ( 'NONE',  ( 28.19062500061451715, -3.027376345333610441, -5.243569643749999898 ) ) ;
#50654 = CARTESIAN_POINT ( 'NONE',  ( 25.43437500061451573, -4.541064518000419881, 2.621784821874995952 ) ) ;
#50655 = CARTESIAN_POINT ( 'NONE',  ( 17.42812500061451786, 6.421520780324663323E-16, -5.243569643749999010 ) ) ;
#50656 = CARTESIAN_POINT ( 'NONE',  ( -3.999999999999999556, 10.06250000000000178, 27.69059892324149530 ) ) ;
#50657 = CARTESIAN_POINT ( 'NONE',  ( 25.56562500061452070, 3.027376345333613106, -5.243569643749998122 ) ) ;
#50658 = CARTESIAN_POINT ( 'NONE',  ( 4.837500001229035895, 4.330127018922191873, 2.499999999999999556 ) ) ;
#50659 = ORIENTED_EDGE ( 'NONE', *, *, #36974, .F. ) ;
#50660 = CARTESIAN_POINT ( 'NONE',  ( 28.80000000000000071, -4.330127018922190985, -2.500000000000001332 ) ) ;
#50661 = CARTESIAN_POINT ( 'NONE',  ( -2.828200636599751609E-16, 14.48750000000000071, -34.61880215351700230 ) ) ;
#50662 = CARTESIAN_POINT ( 'NONE',  ( -3.756430356249999214, 16.54062499938548569, 27.83122392262697531 ) ) ;
#50663 = CARTESIAN_POINT ( 'NONE',  ( 4.546875000614517326, 6.054752690667223547, 3.707466751127219781E-16 ) ) ;
#50664 = CARTESIAN_POINT ( 'NONE',  ( 10.11562500061451608, -6.054752690667223547, -1.112240025338166033E-15 ) ) ;
#50665 = CARTESIAN_POINT ( 'NONE',  ( 5.971875000614516260, 3.027376345333611329, 5.243569643749999010 ) ) ;
#50666 = CARTESIAN_POINT ( 'NONE',  ( 25.05000000122903714, 5.773502691896255534, 3.535250795749688894E-16 ) ) ;
#50667 = CARTESIAN_POINT ( 'NONE',  ( 14.44687500061451679, 6.054752690667223547, 3.707466751127219781E-16 ) ) ;
#50668 = CARTESIAN_POINT ( 'NONE',  ( 28.90312500061451217, 0.000000000000000000, 5.243569643749999010 ) ) ;
#50669 = CARTESIAN_POINT ( 'NONE',  ( 28.08749999999999858, 5.773502691896255534, 3.535250795749688894E-16 ) ) ;
#50670 = CARTESIAN_POINT ( 'NONE',  ( 26.70937500061451431, 0.000000000000000000, 5.243569643749999010 ) ) ;
#50671 = CARTESIAN_POINT ( 'NONE',  ( 3.515625000614516882, 3.027376345333613106, -5.243569643749998122 ) ) ;
#50672 = CARTESIAN_POINT ( 'NONE',  ( 12.96562500061451750, 3.027376345333613106, -5.243569643749998122 ) ) ;
#50673 = VERTEX_POINT ( 'NONE', #37412 ) ;
#50674 = CARTESIAN_POINT ( 'NONE',  ( 9.628125000614517148, -4.541064518000419881, 2.621784821874995952 ) ) ;
#50675 = CARTESIAN_POINT ( 'NONE',  ( 5.240625000614516971, -3.027376345333610441, -5.243569643749999898 ) ) ;
#50676 = CARTESIAN_POINT ( 'NONE',  ( 18.79687500061451644, -2.746126346562642428, -4.756430356249999214 ) ) ;
#50677 = CARTESIAN_POINT ( 'NONE',  ( 13.91250000122903252, 0.000000000000000000, 4.999999999999998224 ) ) ;
#50678 = CARTESIAN_POINT ( 'NONE',  ( 14.73749999999999893, -2.886751345948129988, 4.999999999999997335 ) ) ;
#50679 = EDGE_CURVE ( 'NONE', #14695, #31243, #48685, .T. ) ;
#50680 = CARTESIAN_POINT ( 'NONE',  ( 16.95937500061451786, -4.541064518000417216, -2.621784821875001281 ) ) ;
#50681 = CARTESIAN_POINT ( 'NONE',  ( 10.42500000122903536, -5.773502691896255534, -1.060575238724906372E-15 ) ) ;
#50682 = CARTESIAN_POINT ( 'NONE',  ( 18.89999999999999858, -4.330127018922190985, -2.500000000000001332 ) ) ;
#50683 = CARTESIAN_POINT ( 'NONE',  ( 20.59687500061451360, -3.027376345333610441, -5.243569643749999898 ) ) ;
#50684 = CARTESIAN_POINT ( 'NONE',  ( 4.243569643749999898, 13.72812500061451679, -30.00000000000000000 ) ) ;
#50685 = CARTESIAN_POINT ( 'NONE',  ( -1.999999999999999112, 19.84999999999999787, 26.53589838486224650 ) ) ;
#50686 = CARTESIAN_POINT ( 'NONE',  ( 24.79687500061451644, 0.000000000000000000, 4.756430356249998326 ) ) ;
#50687 = CARTESIAN_POINT ( 'NONE',  ( 20.62499999999999645, -4.330127018922194537, 2.499999999999995559 ) ) ;
#50688 = CARTESIAN_POINT ( 'NONE',  ( 25.67812500061451431, 4.541064518000418104, 2.621784821874999949 ) ) ;
#50689 = CARTESIAN_POINT ( 'NONE',  ( 5.362500001229033586, 0.000000000000000000, 4.999999999999998224 ) ) ;
#50690 = CARTESIAN_POINT ( 'NONE',  ( 29.85937500061451644, 0.000000000000000000, 5.243569643749999010 ) ) ;
#50691 = CARTESIAN_POINT ( 'NONE',  ( 23.32499999999999929, -4.330127018922194537, 2.499999999999995559 ) ) ;
#50692 = CARTESIAN_POINT ( 'NONE',  ( 9.740625000614516082, -3.027376345333610441, -5.243569643749999898 ) ) ;
#50693 = CARTESIAN_POINT ( 'NONE',  ( 27.90937500061451715, 2.746126346562643317, 4.756430356249998326 ) ) ;
#50694 = CARTESIAN_POINT ( 'NONE',  ( 20.07187500061451857, -6.054752690667223547, -1.112240025338166033E-15 ) ) ;
#50695 = CARTESIAN_POINT ( 'NONE',  ( 12.30937500061451573, -5.492252693125287522, -1.008910452111647106E-15 ) ) ;
#50696 = CARTESIAN_POINT ( 'NONE',  ( 4.190625000614518925, -3.027376345333614438, 5.243569643749998122 ) ) ;
#50697 = CARTESIAN_POINT ( 'NONE',  ( 11.67187500061451821, 3.027376345333613106, -5.243569643749998122 ) ) ;
#50698 = ORIENTED_EDGE ( 'NONE', *, *, #64830, .T. ) ;
#50699 = CARTESIAN_POINT ( 'NONE',  ( 21.53437500061451715, 6.421520780324663323E-16, -5.243569643749999010 ) ) ;
#50700 = CARTESIAN_POINT ( 'NONE',  ( 0.000000000000000000, 20.00000000000000000, 26.00000000000000000 ) ) ;
#50701 = CARTESIAN_POINT ( 'NONE',  ( 28.57499999999999929, 4.330127018922191873, 2.499999999999999556 ) ) ;
#50702 = CARTESIAN_POINT ( 'NONE',  ( 5.812500000000001776, -5.773502691896255534, -1.060575238724906372E-15 ) ) ;
#50703 = CARTESIAN_POINT ( 'NONE',  ( 14.92500000122903181, -5.773502691896255534, -1.060575238724906372E-15 ) ) ;
#50704 = CARTESIAN_POINT ( 'NONE',  ( 3.999999999999999112, 15.27500000000000036, -30.00000000000000000 ) ) ;
#50705 = DIRECTION ( 'NONE',  ( -1.000000000000000000, -0.000000000000000000, -0.000000000000000000 ) ) ;
#50706 = ORIENTED_EDGE ( 'NONE', *, *, #163, .F. ) ;
#50707 = CARTESIAN_POINT ( 'NONE',  ( 12.37500000000000000, 4.330127018922191873, 2.499999999999999556 ) ) ;
#50708 = CARTESIAN_POINT ( 'NONE',  ( 26.54062500061451146, 6.054752690667223547, 3.707466751127219781E-16 ) ) ;
#50709 = CARTESIAN_POINT ( 'NONE',  ( 16.50000000000000000, 0.000000000000000000, 4.999999999999998224 ) ) ;
#50710 = CARTESIAN_POINT ( 'NONE',  ( 10.23750000122903359, 4.330127018922191873, 2.499999999999999556 ) ) ;
#50711 = CARTESIAN_POINT ( 'NONE',  ( 8.690625000614515372, -3.027376345333614438, 5.243569643749998122 ) ) ;
#50712 = B_SPLINE_CURVE_WITH_KNOTS ( 'NONE', 3,
 ( #1271, #914, #12699, #69944, #45969, #28977, #51515, #23778, #58477, #68865 ),
 .UNSPECIFIED., .F., .F.,
 ( 4, 3, 3, 4 ),
 ( 1.663831787158942381E-16, 2.812505563865755982E-05, 5.721718141143529657E-05, 8.630979428994332348E-05 ),
 .UNSPECIFIED. ) ;
#50713 = CARTESIAN_POINT ( 'NONE',  ( 9.600000000000001421, 4.330127018922192761, -2.499999999999997780 ) ) ;
#50714 = LINE ( 'NONE', #68070, #35958 ) ;
#50715 = CARTESIAN_POINT ( 'NONE',  ( 4.243569643749999010, 14.72187500061451715, -32.45002607614398471 ) ) ;
#50716 = CARTESIAN_POINT ( 'NONE',  ( 27.78750000122903074, 4.330127018922191873, 2.499999999999999556 ) ) ;
#50717 = CARTESIAN_POINT ( 'NONE',  ( -3.756430356249999214, 13.72812499938548392, 27.83122392262697176 ) ) ;
#50718 = CARTESIAN_POINT ( 'NONE',  ( 7.350000000000002309, 4.330127018922192761, -2.499999999999997780 ) ) ;
#50719 = LINE ( 'NONE', #28543, #50367 ) ;
#50720 = ORIENTED_EDGE ( 'NONE', *, *, #46859, .F. ) ;
#50721 = CARTESIAN_POINT ( 'NONE',  ( 24.36562500061451786, 3.027376345333611329, 5.243569643749999010 ) ) ;
#50722 = CARTESIAN_POINT ( 'NONE',  ( 14.58750000122903323, 6.123233995736764310E-16, -4.999999999999998224 ) ) ;
#50723 = CARTESIAN_POINT ( 'NONE',  ( 3.381234057738627730, -3.683476499272080318, -3.635624298366154861 ) ) ;
#50724 = CARTESIAN_POINT ( 'NONE',  ( 28.65937500061451715, -4.541064518000417216, -2.621784821875001281 ) ) ;
#50725 = CARTESIAN_POINT ( 'NONE',  ( 19.99687500061451573, -3.027376345333614438, 5.243569643749998122 ) ) ;
#50726 = CARTESIAN_POINT ( 'NONE',  ( 17.12812500061451715, 4.541064518000418104, 2.621784821874999949 ) ) ;
#50727 = CARTESIAN_POINT ( 'NONE',  ( -3.000416591977282496E-16, 12.49062500061459424, -34.90005215228797653 ) ) ;
#50728 = CARTESIAN_POINT ( 'NONE',  ( 7.078125000614516438, 6.421520780324663323E-16, -5.243569643749999010 ) ) ;
#50729 = CARTESIAN_POINT ( 'NONE',  ( 28.23750000122903359, 4.330127018922191873, 2.499999999999999556 ) ) ;
#50730 = CARTESIAN_POINT ( 'NONE',  ( 23.93437500061451573, 4.119189519843966529, 2.378215178124999607 ) ) ;
#50731 = CARTESIAN_POINT ( 'NONE',  ( 19.82812500061451644, 4.541064518000418104, 2.621784821874999949 ) ) ;
#50732 = CYLINDRICAL_SURFACE ( 'NONE', #24443, 4.000000000000000000 ) ;
#50733 = CARTESIAN_POINT ( 'NONE',  ( 3.756430356249998770, 18.90312499938548640, 32.16877607737302469 ) ) ;
#50734 = CARTESIAN_POINT ( 'NONE',  ( 13.62187500061451750, 3.027376345333611329, 5.243569643749999010 ) ) ;
#50735 = CARTESIAN_POINT ( 'NONE',  ( 11.78437500061451892, 4.541064518000418104, 2.621784821874999949 ) ) ;
#50736 = CARTESIAN_POINT ( 'NONE',  ( 21.30937500061451573, 0.000000000000000000, 5.243569643749999010 ) ) ;
#50737 = EDGE_LOOP ( 'NONE', ( #34265, #413, #47200, #70421 ) ) ;
#50738 = CARTESIAN_POINT ( 'NONE',  ( -1.487416814333745711E-14, 14.82500000122903572, -26.00000000000000000 ) ) ;
#50739 = CARTESIAN_POINT ( 'NONE',  ( 25.49062500061451786, -3.027376345333610441, -5.243569643749999898 ) ) ;
#50740 = CARTESIAN_POINT ( 'NONE',  ( 26.91562500061451146, 3.027376345333613106, -5.243569643749998122 ) ) ;
#50741 = CARTESIAN_POINT ( 'NONE',  ( 15.13125000122903252, 4.330127018922191873, 2.499999999999999556 ) ) ;
#50742 = CARTESIAN_POINT ( 'NONE',  ( 1.999999999999998668, 17.60000000000000142, 26.53589838486224650 ) ) ;
#50743 = CARTESIAN_POINT ( 'NONE',  ( 4.659375000614518925, 0.000000000000000000, 5.243569643749999010 ) ) ;
#50744 = CARTESIAN_POINT ( 'NONE',  ( 11.66250000122903430, 0.000000000000000000, 4.999999999999998224 ) ) ;
#50745 = CARTESIAN_POINT ( 'NONE',  ( 7.050000001229036251, 5.773502691896255534, 3.535250795749688894E-16 ) ) ;
#50746 = CARTESIAN_POINT ( 'NONE',  ( 2.803125000614518747, 0.000000000000000000, 5.243569643749999010 ) ) ;
#50747 = CARTESIAN_POINT ( 'NONE',  ( 4.000000000000000000, 17.84374999877096712, 30.00000000000000000 ) ) ;
#50748 = CARTESIAN_POINT ( 'NONE',  ( 15.99375000122903323, 5.773502691896255534, 3.535250795749688894E-16 ) ) ;
#50749 = CARTESIAN_POINT ( 'NONE',  ( 11.44687500061451857, -3.027376345333614438, 5.243569643749998122 ) ) ;
#50750 = CARTESIAN_POINT ( 'NONE',  ( 4.000000000000000000, 12.95000000000000107, 30.00000000000000000 ) ) ;
#50751 = CARTESIAN_POINT ( 'NONE',  ( 19.79062500061451502, 6.054752690667223547, 3.707466751127219781E-16 ) ) ;
#50752 = CARTESIAN_POINT ( 'NONE',  ( 12.60937500061451821, 4.541064518000418104, -2.621784821874998173 ) ) ;
#50753 = CARTESIAN_POINT ( 'NONE',  ( 6.065625000614516260, -6.054752690667223547, -1.112240025338166033E-15 ) ) ;
#50754 = CARTESIAN_POINT ( 'NONE',  ( 22.65937500061451715, 0.000000000000000000, 5.243569643749999010 ) ) ;
#50755 = CARTESIAN_POINT ( 'NONE',  ( 9.759375000614516793, -4.541064518000417216, -2.621784821875001281 ) ) ;
#50756 = CARTESIAN_POINT ( 'NONE',  ( 4.753125000614515372, -4.541064518000417216, -2.621784821875001281 ) ) ;
#50757 = CARTESIAN_POINT ( 'NONE',  ( 5.887500000000000178, -2.886751345948126435, -5.000000000000000000 ) ) ;
#50758 = CARTESIAN_POINT ( 'NONE',  ( 5.925000001229033586, -5.773502691896255534, -1.060575238724906372E-15 ) ) ;
#50759 = CARTESIAN_POINT ( 'NONE',  ( 20.01562500061451644, -6.054752690667223547, -1.112240025338166033E-15 ) ) ;
#50760 = CARTESIAN_POINT ( 'NONE',  ( 6.975000001229032520, 2.886751345948129099, -4.999999999999998224 ) ) ;
#50761 = CARTESIAN_POINT ( 'NONE',  ( 18.14062500061451644, -3.027376345333614438, 5.243569643749998122 ) ) ;
#50762 = CARTESIAN_POINT ( 'NONE',  ( 14.20312500061451644, -4.541064518000417216, -2.621784821875001281 ) ) ;
#50763 = CARTESIAN_POINT ( 'NONE',  ( 26.97187500061451360, 2.746126346562645981, -4.756430356249997438 ) ) ;
#50764 = CARTESIAN_POINT ( 'NONE',  ( 13.12500000000000178, 6.123233995736764310E-16, -4.999999999999998224 ) ) ;
#50765 = CARTESIAN_POINT ( 'NONE',  ( 9.637500001229033941, 6.123233995736764310E-16, -4.999999999999998224 ) ) ;
#50766 = CARTESIAN_POINT ( 'NONE',  ( 4.828125000614518214, 6.421520780324663323E-16, -5.243569643749999010 ) ) ;
#50767 =( BOUNDED_CURVE ( )  B_SPLINE_CURVE ( 2, ( #3257, #59750, #71210, #49057, #21325, #71585, #70485 ),
 .UNSPECIFIED., .F., .F. ) 
 B_SPLINE_CURVE_WITH_KNOTS ( ( 3, 2, 2, 3 ),
 ( 0.6666666666666666297, 0.6694444444444443976, 0.6722222222222222765, 0.6750000000000000444 ),
 .UNSPECIFIED. ) 
 CURVE ( )  GEOMETRIC_REPRESENTATION_ITEM ( )  RATIONAL_B_SPLINE_CURVE ( ( 1.000000000000000000, 0.8660254037844387076, 1.000000000000000000, 0.8660254037844387076, 1.000000000000000000, 0.8660254037844387076, 1.000000000000000000 ) ) 
 REPRESENTATION_ITEM ( '' )  );
#50768 = ADVANCED_FACE ( 'NONE', ( #59563 ), #3444, .T. ) ;
#50769 = CARTESIAN_POINT ( 'NONE',  ( 21.71250000122903501, -4.330127018922190985, -2.500000000000001332 ) ) ;
#50770 = CARTESIAN_POINT ( 'NONE',  ( 27.41250000000000142, -5.773502691896255534, -1.060575238724906372E-15 ) ) ;
#50771 = CARTESIAN_POINT ( 'NONE',  ( -2.121784821874999949, 11.68437500061451750, -33.67503911421598417 ) ) ;
#50772 = CYLINDRICAL_SURFACE ( 'NONE', #59527, 4.000000000000000000 ) ;
#50773 = CARTESIAN_POINT ( 'NONE',  ( 2.812500001229033320, -4.330127018922190985, -2.500000000000001332 ) ) ;
#50774 = CARTESIAN_POINT ( 'NONE',  ( 50.00000000000000000, -1.494782592887582195, 8.875000000000014211 ) ) ;
#50775 = CARTESIAN_POINT ( 'NONE',  ( 21.42187500061451644, -6.054752690667223547, -1.112240025338166033E-15 ) ) ;
#50776 = CARTESIAN_POINT ( 'NONE',  ( -5.810221930991193690E-16, 14.15000000122903145, -34.00000000000000000 ) ) ;
#50777 = CARTESIAN_POINT ( 'NONE',  ( 16.45312500061451289, -4.541064518000417216, -2.621784821875001281 ) ) ;
#50778 = CARTESIAN_POINT ( 'NONE',  ( 11.34375000122903465, -2.886751345948125991, -5.000000000000000000 ) ) ;
#50779 = CARTESIAN_POINT ( 'NONE',  ( 13.23750000000000071, 5.773502691896255534, 3.535250795749688401E-16 ) ) ;
#50780 = CARTESIAN_POINT ( 'NONE',  ( -1.071796769724488563, 15.59240381056766722, 34.00000000000000000 ) ) ;
#50781 = CARTESIAN_POINT ( 'NONE',  ( 28.99687500061451573, -3.027376345333614438, 5.243569643749998122 ) ) ;
#50782 = CARTESIAN_POINT ( 'NONE',  ( 21.57187500061451146, 4.119189519843966529, 2.378215178124999607 ) ) ;
#50783 = CARTESIAN_POINT ( 'NONE',  ( 11.57812500061451644, 6.421520780324663323E-16, -5.243569643749999010 ) ) ;
#50784 = CARTESIAN_POINT ( 'NONE',  ( 10.92187500061451644, 3.027376345333611329, 5.243569643749999010 ) ) ;
#50785 = ORIENTED_EDGE ( 'NONE', *, *, #68132, .T. ) ;
#50786 = CARTESIAN_POINT ( 'NONE',  ( 29.42812500061451431, -4.541064518000419881, 2.621784821874995952 ) ) ;
#50787 = CARTESIAN_POINT ( 'NONE',  ( 23.01562500061451644, 3.027376345333611329, 5.243569643749999010 ) ) ;
#50788 = CARTESIAN_POINT ( 'NONE',  ( 27.82499999999999929, -4.330127018922194537, 2.499999999999995559 ) ) ;
#50789 = CARTESIAN_POINT ( 'NONE',  ( 3.242103837493086330E-14, 11.33750000000000213, 26.00000000000000711 ) ) ;
#50790 = CARTESIAN_POINT ( 'NONE',  ( 12.97499999999999964, -4.330127018922194537, 2.499999999999995559 ) ) ;
#50791 = CARTESIAN_POINT ( 'NONE',  ( 21.82500000122903572, 2.886751345948129099, -4.999999999999998224 ) ) ;
#50792 = CARTESIAN_POINT ( 'NONE',  ( 15.74062500061451608, 6.054752690667223547, 3.707466751127219781E-16 ) ) ;
#50793 = CARTESIAN_POINT ( 'NONE',  ( 12.08437500061451608, 5.492252693125287522, 3.363034840372157021E-16 ) ) ;
#50794 = VERTEX_POINT ( 'NONE', #36315 ) ;
#50795 = CARTESIAN_POINT ( 'NONE',  ( 19.76250000000000639, -5.773502691896255534, -1.060575238724906372E-15 ) ) ;
#50796 = CARTESIAN_POINT ( 'NONE',  ( 24.86250000000000071, 2.886751345948129099, -4.999999999999998224 ) ) ;
#50797 = CARTESIAN_POINT ( 'NONE',  ( 21.98437500061451644, 6.421520780324663323E-16, -5.243569643749999010 ) ) ;
#50798 = CARTESIAN_POINT ( 'NONE',  ( 26.27812500061451573, -4.541064518000419881, 2.621784821874995952 ) ) ;
#50799 = EDGE_LOOP ( 'NONE', ( #19042, #36110, #21698, #4198 ) ) ;
#50800 = DIRECTION ( 'NONE',  ( 1.000000000000000000, 0.000000000000000000, 0.000000000000000000 ) ) ;
#50801 = CARTESIAN_POINT ( 'NONE',  ( 9.440625000614517148, 6.054752690667223547, 3.707466751127219781E-16 ) ) ;
#50802 = DIRECTION ( 'NONE',  ( -0.000000000000000000, -1.000000000000000000, -0.000000000000000000 ) ) ;
#50803 = CARTESIAN_POINT ( 'NONE',  ( 14.77500000000000036, -4.330127018922194537, 2.499999999999995559 ) ) ;
#50804 = CARTESIAN_POINT ( 'NONE',  ( -2.121784821874996840, 18.52812500061451928, 33.67503911421598417 ) ) ;
#50805 = CARTESIAN_POINT ( 'NONE',  ( 4.359375000614517326, -4.541064518000417216, -2.621784821875001281 ) ) ;
#50806 = B_SPLINE_CURVE_WITH_KNOTS ( 'NONE', 3,
 ( #6606, #6236, #67936, #1073, #18027, #13216, #63823, #705, #40584, #63104 ),
 .UNSPECIFIED., .F., .F.,
 ( 4, 3, 3, 4 ),
 ( 0.000000000000000000, 5.625111044264893015E-05, 0.0001079408190112657892, 0.0001596376222420049817 ),
 .UNSPECIFIED. ) ;
#50807 = CARTESIAN_POINT ( 'NONE',  ( 25.02187500061451431, -6.054752690667223547, -1.112240025338166033E-15 ) ) ;
#50808 = ORIENTED_EDGE ( 'NONE', *, *, #6209, .T. ) ;
#50809 = CARTESIAN_POINT ( 'NONE',  ( 24.55312500061451786, -4.541064518000417216, -2.621784821875001281 ) ) ;
#50810 = CARTESIAN_POINT ( 'NONE',  ( 25.69687500061451502, 6.054752690667223547, 3.707466751127219781E-16 ) ) ;
#50811 = CARTESIAN_POINT ( 'NONE',  ( -3.000416591977282496E-16, 17.89062500061459104, -34.90005215228797653 ) ) ;
#50812 = CARTESIAN_POINT ( 'NONE',  ( 10.61250000000000071, 2.886751345948126879, 4.999999999999999112 ) ) ;
#50813 = CARTESIAN_POINT ( 'NONE',  ( 9.890625000614516438, 6.054752690667223547, 3.707466751127219781E-16 ) ) ;
#50814 = DIRECTION ( 'NONE',  ( -1.000000000000000000, -0.000000000000000000, -0.000000000000000000 ) ) ;
#50815 = CARTESIAN_POINT ( 'NONE',  ( 13.38750000000000107, -2.886751345948130876, 4.999999999999996447 ) ) ;
#50816 = CARTESIAN_POINT ( 'NONE',  ( 26.12812500061451360, 4.541064518000418104, 2.621784821874999949 ) ) ;
#50817 = CARTESIAN_POINT ( 'NONE',  ( 12.04687500061451821, -2.746126346562642428, -4.756430356249999214 ) ) ;
#50818 = CARTESIAN_POINT ( 'NONE',  ( 3.928125000614516527, 6.421520780324663323E-16, -5.243569643749999010 ) ) ;
#50819 = CARTESIAN_POINT ( 'NONE',  ( 20.55937500061451573, -4.541064518000417216, -2.621784821875001281 ) ) ;
#50820 = CARTESIAN_POINT ( 'NONE',  ( 4.243569643749999898, 15.54687500061451644, 32.45002607614398471 ) ) ;
#50821 = CARTESIAN_POINT ( 'NONE',  ( 20.82187500061451857, 3.027376345333611329, 5.243569643749999010 ) ) ;
#50822 = CARTESIAN_POINT ( 'NONE',  ( 3.300000000000000711, 4.330127018922192761, -2.499999999999997780 ) ) ;
#50823 = CARTESIAN_POINT ( 'NONE',  ( -2.121784821874999949, 19.33437500061451786, 26.32496088578401938 ) ) ;
#50824 = CARTESIAN_POINT ( 'NONE',  ( 10.52812500061451750, -4.541064518000419881, 2.621784821874995952 ) ) ;
#50826 =( BOUNDED_CURVE ( )  B_SPLINE_CURVE ( 2, ( #38826, #44737, #33627, #60232, #61341, #32180, #27737 ),
 .UNSPECIFIED., .F., .F. ) 
 B_SPLINE_CURVE_WITH_KNOTS ( ( 3, 2, 2, 3 ),
 ( 0.6600000000000000311, 0.6633333333333333304, 0.6666666666666666297, 0.6700000000000000400 ),
 .UNSPECIFIED. ) 
 CURVE ( )  GEOMETRIC_REPRESENTATION_ITEM ( )  RATIONAL_B_SPLINE_CURVE ( ( 1.000000000000000000, 0.8660254037844387076, 1.000000000000000000, 0.8660254037844387076, 1.000000000000000000, 0.8660254037844387076, 1.000000000000000000 ) ) 
 REPRESENTATION_ITEM ( '' )  );
#50825 = CARTESIAN_POINT ( 'NONE',  ( 7.950000000000001954, 0.000000000000000000, 4.999999999999998224 ) ) ;
#50827 = ADVANCED_FACE ( 'NONE', ( #58830 ), #25963, .F. ) ;
#50828 = CARTESIAN_POINT ( 'NONE',  ( 7.996875000614519280, -3.027376345333610441, -5.243569643749999898 ) ) ;
#50829 = CARTESIAN_POINT ( 'NONE',  ( -3.999999999999999112, 16.02500000122903501, -32.30940107675850470 ) ) ;
#50830 = ADVANCED_FACE ( 'NONE', ( #2336 ), #65852, .F. ) ;
#50831 = CARTESIAN_POINT ( 'NONE',  ( 8.015625000614518214, 3.027376345333613106, -5.243569643749998122 ) ) ;
#50832 = CARTESIAN_POINT ( 'NONE',  ( 11.37187500061451750, 3.027376345333611329, 5.243569643749999010 ) ) ;
#50833 = CARTESIAN_POINT ( 'NONE',  ( 18.11250000122903359, -4.330127018922190985, -2.500000000000001332 ) ) ;
#50834 = CARTESIAN_POINT ( 'NONE',  ( 8.671875000614518214, 3.027376345333611329, 5.243569643749999010 ) ) ;
#50835 = CARTESIAN_POINT ( 'NONE',  ( 10.45312500061451644, 0.000000000000000000, 5.243569643749999010 ) ) ;
#50836 = CARTESIAN_POINT ( 'NONE',  ( 5.915625000614515905, 3.027376345333611329, 5.243569643749999010 ) ) ;
#50837 = CARTESIAN_POINT ( 'NONE',  ( 26.08125000122903003, -4.330127018922194537, 2.499999999999995559 ) ) ;
#50838 = CARTESIAN_POINT ( 'NONE',  ( 20.03437500061451715, -4.541064518000419881, 2.621784821874995952 ) ) ;
#50839 = CARTESIAN_POINT ( 'NONE',  ( 4.555452590171750415, 2.061616698417762628, 4.786020548300175648 ) ) ;
#50840 = CARTESIAN_POINT ( 'NONE',  ( 26.46562500061451573, 3.027376345333613106, -5.243569643749998122 ) ) ;
#50841 = CARTESIAN_POINT ( 'NONE',  ( 12.47812500061451502, 6.421520780324663323E-16, -5.243569643749999010 ) ) ;
#50842 = CARTESIAN_POINT ( 'NONE',  ( 29.07187500061451502, -6.054752690667223547, -1.112240025338166033E-15 ) ) ;
#50843 = CARTESIAN_POINT ( 'NONE',  ( -4.243569643749999898, 9.959375000614517859, -30.00000000000000000 ) ) ;
#50844 = EDGE_CURVE ( 'NONE', #38197, #29431, #25591, .T. ) ;
#50845 = CARTESIAN_POINT ( 'NONE',  ( 12.75000000122903643, -2.886751345948125991, -5.000000000000000000 ) ) ;
#50846 = CARTESIAN_POINT ( 'NONE',  ( 27.32812500061451644, 6.421520780324663323E-16, -5.243569643749999010 ) ) ;
#50847 = CARTESIAN_POINT ( 'NONE',  ( -2.121784821874999949, 14.77812500061451750, -33.67503911421598417 ) ) ;
#50848 = CARTESIAN_POINT ( 'NONE',  ( 14.70000000122903394, 5.773502691896255534, 3.535250795749688894E-16 ) ) ;
#50849 = CARTESIAN_POINT ( 'NONE',  ( 12.18750000000000000, -2.886751345948125991, -5.000000000000000000 ) ) ;
#50850 = CARTESIAN_POINT ( 'NONE',  ( 21.66562500061451502, 3.027376345333611329, 5.243569643749999010 ) ) ;
#50851 = CARTESIAN_POINT ( 'NONE',  ( 8.221875000614518925, 3.027376345333611329, 5.243569643749999010 ) ) ;
#50852 = EDGE_CURVE ( 'NONE', #19210, #28191, #39246, .T. ) ;
#50853 = CARTESIAN_POINT ( 'NONE',  ( 8.025000001229035007, 2.886751345948126879, 4.999999999999999112 ) ) ;
#50854 = CARTESIAN_POINT ( 'NONE',  ( 17.17500000122903359, -5.773502691896255534, -1.060575238724906372E-15 ) ) ;
#50855 = CARTESIAN_POINT ( 'NONE',  ( 13.00312500061451537, 4.541064518000418104, -2.621784821874998173 ) ) ;
#50856 = CIRCLE ( 'NONE', #28424, 4.000000000000003553 ) ;
#50857 = CARTESIAN_POINT ( 'NONE',  ( 16.26562500061451289, 3.027376345333611329, 5.243569643749999010 ) ) ;
#50858 = CARTESIAN_POINT ( 'NONE',  ( 28.65000000122903145, 5.773502691896255534, 3.535250795749688894E-16 ) ) ;
#50859 = CARTESIAN_POINT ( 'NONE',  ( 21.97500000000000142, -4.330127018922194537, 2.499999999999995559 ) ) ;
#50860 = CARTESIAN_POINT ( 'NONE',  ( 22.28437500061451715, -4.541064518000419881, 2.621784821874995952 ) ) ;
#50861 = CARTESIAN_POINT ( 'NONE',  ( 4.000000000000000000, 13.88750000000000107, 27.69059892324149885 ) ) ;
#50862 = CARTESIAN_POINT ( 'NONE',  ( 10.20000000122903572, 5.773502691896255534, 3.535250795749688894E-16 ) ) ;
#50863 = CARTESIAN_POINT ( 'NONE',  ( 28.77187500061451431, 3.027376345333613106, -5.243569643749998122 ) ) ;
#50864 = CARTESIAN_POINT ( 'NONE',  ( 5.221875000614519813, -6.054752690667223547, -1.112240025338166033E-15 ) ) ;
#50865 = CARTESIAN_POINT ( 'NONE',  ( 24.70312500061451644, 4.541064518000418104, -2.621784821874998173 ) ) ;
#50866 = CARTESIAN_POINT ( 'NONE',  ( -3.756430356249999214, 14.74062499938548676, 27.83122392262697176 ) ) ;
#50867 = CARTESIAN_POINT ( 'NONE',  ( 26.11875000122902790, -5.773502691896255534, -1.060575238724906372E-15 ) ) ;
#50868 = CARTESIAN_POINT ( 'NONE',  ( 10.50937500061451679, 0.000000000000000000, 5.243569643749999010 ) ) ;
#50869 = CARTESIAN_POINT ( 'NONE',  ( 0.000000000000000000, 20.00000000000000000, -30.00000000000000000 ) ) ;
#50870 = CARTESIAN_POINT ( 'NONE',  ( 29.24062500061451431, 6.054752690667223547, 3.707466751127219781E-16 ) ) ;
#50871 = CARTESIAN_POINT ( 'NONE',  ( 7.434375000614519280, -4.541064518000419881, 2.621784821874995952 ) ) ;
#50872 = DIRECTION ( 'NONE',  ( -0.000000000000000000, -1.000000000000000000, -0.000000000000000000 ) ) ;
#50873 = CARTESIAN_POINT ( 'NONE',  ( 25.32187500061451857, 3.027376345333611329, 5.243569643749999010 ) ) ;
#50874 = CARTESIAN_POINT ( 'NONE',  ( 9.001249775931846008E-16, 10.91562500061459495, 34.90005215228797653 ) ) ;
#50875 = CARTESIAN_POINT ( 'NONE',  ( 18.59999999999999787, 4.330127018922192761, -2.499999999999997780 ) ) ;
#50876 = ORIENTED_EDGE ( 'NONE', *, *, #420, .F. ) ;
#50877 = CARTESIAN_POINT ( 'NONE',  ( 27.56250000000000000, 2.886751345948129099, -4.999999999999998224 ) ) ;
#50878 = CARTESIAN_POINT ( 'NONE',  ( 29.03437500061451715, -4.541064518000419881, 2.621784821874995952 ) ) ;
#50879 = VERTEX_POINT ( 'NONE', #38884 ) ;
#50880 = CARTESIAN_POINT ( 'NONE',  ( 15.92812500061451608, -4.541064518000419881, 2.621784821874995952 ) ) ;
#50881 = CARTESIAN_POINT ( 'NONE',  ( 7.790625000614518569, -3.027376345333614438, 5.243569643749998122 ) ) ;
#50882 = CARTESIAN_POINT ( 'NONE',  ( 17.97187500061451360, 4.119189519843966529, 2.378215178124999607 ) ) ;
#50883 = CARTESIAN_POINT ( 'NONE',  ( 4.396875000614516971, -3.027376345333610441, -5.243569643749999898 ) ) ;
#50884 = CARTESIAN_POINT ( 'NONE',  ( 17.17500000122903359, -5.773502691896255534, -1.060575238724906372E-15 ) ) ;
#50885 = CARTESIAN_POINT ( 'NONE',  ( 22.08749999999999858, -2.886751345948125991, -5.000000000000000000 ) ) ;
#50886 = CARTESIAN_POINT ( 'NONE',  ( 15.78749999999999964, -2.886751345948126435, -5.000000000000000000 ) ) ;
#50887 = CARTESIAN_POINT ( 'NONE',  ( 6.346875000614517148, 6.054752690667223547, 3.707466751127219781E-16 ) ) ;
#50888 = CARTESIAN_POINT ( 'NONE',  ( 10.80937500061451928, 4.541064518000418104, -2.621784821874998173 ) ) ;
#50889 = CARTESIAN_POINT ( 'NONE',  ( 21.90937500061451715, -4.541064518000417216, -2.621784821875001281 ) ) ;
#50890 = LINE ( 'NONE', #5463, #51326 ) ;
#50891 = ORIENTED_EDGE ( 'NONE', *, *, #20037, .F. ) ;
#50892 = CARTESIAN_POINT ( 'NONE',  ( 5.334375000614517859, 6.421520780324663323E-16, -5.243569643749999010 ) ) ;
#50893 = CARTESIAN_POINT ( 'NONE',  ( 6.871875000614517504, 3.027376345333611329, 5.243569643749999010 ) ) ;
#50894 = CARTESIAN_POINT ( 'NONE',  ( 19.65000000000000213, 0.000000000000000000, 4.999999999999998224 ) ) ;
#50895 = CARTESIAN_POINT ( 'NONE',  ( 16.82812500061451644, -4.541064518000419881, 2.621784821874995952 ) ) ;
#50896 = CARTESIAN_POINT ( 'NONE',  ( -2.000000000000001776, 17.30000000000000071, 33.46410161513775705 ) ) ;
#50897 = CARTESIAN_POINT ( 'NONE',  ( 18.26249999999999929, 2.886751345948126879, 4.999999999999998224 ) ) ;
#50898 = CARTESIAN_POINT ( 'NONE',  ( 19.17187500061451999, -5.492252693125287522, -1.008910452111647106E-15 ) ) ;
#50899 = CARTESIAN_POINT ( 'NONE',  ( 11.01562500061451821, -6.054752690667223547, -1.112240025338166033E-15 ) ) ;
#50900 = CARTESIAN_POINT ( 'NONE',  ( 27.87187500061451573, 3.027376345333613106, -5.243569643749998122 ) ) ;
#50901 = LINE ( 'NONE', #11740, #18325 ) ;
#50902 = CARTESIAN_POINT ( 'NONE',  ( 28.05937500061451573, 0.000000000000000000, 5.243569643749999010 ) ) ;
#50903 = CARTESIAN_POINT ( 'NONE',  ( 9.825000000000001066, -4.330127018922194537, 2.499999999999995559 ) ) ;
#50904 = CARTESIAN_POINT ( 'NONE',  ( 8.484601909799253346E-16, 16.17500000122903003, 34.61880215351700230 ) ) ;
#50905 = CARTESIAN_POINT ( 'NONE',  ( 9.075000001229033941, -5.773502691896255534, -1.060575238724906372E-15 ) ) ;
#50906 = EDGE_CURVE ( 'NONE', #1518, #31518, #63352, .T. ) ;
#50907 = CARTESIAN_POINT ( 'NONE',  ( 19.88437500061451857, 4.541064518000418104, 2.621784821874999949 ) ) ;
#50908 = CARTESIAN_POINT ( 'NONE',  ( 13.02187500061451608, 3.027376345333613106, -5.243569643749998122 ) ) ;
#50909 = CARTESIAN_POINT ( 'NONE',  ( -0.6909613911670684505, 4.953869264242466208, -33.94222170460632526 ) ) ;
#50910 = ORIENTED_EDGE ( 'NONE', *, *, #39400, .F. ) ;
#50911 = CARTESIAN_POINT ( 'NONE',  ( 14.54062500061451679, -3.027376345333614438, 5.243569643749998122 ) ) ;
#50912 = CARTESIAN_POINT ( 'NONE',  ( 26.77500000122903145, 2.886751345948129099, -4.999999999999998224 ) ) ;
#50913 = CARTESIAN_POINT ( 'NONE',  ( 14.52187500061451608, 3.027376345333611329, 5.243569643749999010 ) ) ;
#50914 = CARTESIAN_POINT ( 'NONE',  ( 2.915625000614516793, -6.054752690667223547, -1.112240025338166033E-15 ) ) ;
#50915 = CARTESIAN_POINT ( 'NONE',  ( 17.46562500061451217, 3.027376345333613106, -5.243569643749998122 ) ) ;
#50916 = EDGE_CURVE ( 'NONE', #27263, #55447, #66586, .T. ) ;
#50917 = CARTESIAN_POINT ( 'NONE',  ( 45.00000000000000000, 2.500000000000000444, 3.499999999999999112 ) ) ;
#50918 = CARTESIAN_POINT ( 'NONE',  ( 26.18437500061451573, 4.541064518000418104, 2.621784821874999949 ) ) ;
#50919 = CARTESIAN_POINT ( 'NONE',  ( 4.243569643749999898, 10.57812500061451821, 30.00000000000000000 ) ) ;
#50920 = CARTESIAN_POINT ( 'NONE',  ( 14.55937500061451573, 0.000000000000000000, 5.243569643749999010 ) ) ;
#50921 = CARTESIAN_POINT ( 'NONE',  ( 13.05000000122903536, -2.886751345948129988, 4.999999999999997335 ) ) ;
#50922 = CARTESIAN_POINT ( 'NONE',  ( 8.071875000614518569, 2.746126346562645981, -4.756430356249997438 ) ) ;
#50923 = CARTESIAN_POINT ( 'NONE',  ( -4.243569643749998122, 18.54687500061451644, -27.54997392385601174 ) ) ;
#50924 = EDGE_CURVE ( 'NONE', #46789, #56113, #67681, .T. ) ;
#50925 = CARTESIAN_POINT ( 'NONE',  ( 19.09687500061451360, -3.027376345333614438, 5.243569643749998122 ) ) ;
#50926 = CARTESIAN_POINT ( 'NONE',  ( 20.55000000122903359, 5.773502691896255534, 3.535250795749688894E-16 ) ) ;
#50927 = CARTESIAN_POINT ( 'NONE',  ( 15.57187500061451679, -6.054752690667223547, -1.112240025338166033E-15 ) ) ;
#50928 = CARTESIAN_POINT ( 'NONE',  ( 2.121784821875001281, 11.45937500061451786, 33.67503911421598417 ) ) ;
#50929 = CARTESIAN_POINT ( 'NONE',  ( 21.33750000122903145, 6.123233995736764310E-16, -4.999999999999998224 ) ) ;
#50930 = CARTESIAN_POINT ( 'NONE',  ( 15.66562500061451857, 3.027376345333613106, -5.243569643749998122 ) ) ;
#50931 = CARTESIAN_POINT ( 'NONE',  ( 28.79062500061451502, 6.054752690667223547, 3.707466751127219781E-16 ) ) ;
#50932 = ORIENTED_EDGE ( 'NONE', *, *, #26912, .F. ) ;
#50933 = ORIENTED_EDGE ( 'NONE', *, *, #53086, .F. ) ;
#50934 = CARTESIAN_POINT ( 'NONE',  ( 20.28750000000000142, -2.886751345948125991, -5.000000000000000000 ) ) ;
#50935 = CYLINDRICAL_SURFACE ( 'NONE', #3156, 4.999999999999998224 ) ;
#50936 = CARTESIAN_POINT ( 'NONE',  ( 1.347985686992487997, 4.821799686897913162, 33.77548493594544965 ) ) ;
#50937 = CARTESIAN_POINT ( 'NONE',  ( 15.56250000122903465, 4.330127018922192761, -2.499999999999997780 ) ) ;
#50938 = CARTESIAN_POINT ( 'NONE',  ( 20.57812500061451644, 6.421520780324663323E-16, -5.243569643749999010 ) ) ;
#50939 = CARTESIAN_POINT ( 'NONE',  ( 26.57812500061451644, 4.541064518000418104, 2.621784821874999949 ) ) ;
#50940 = CARTESIAN_POINT ( 'NONE',  ( 6.028125000614517504, -4.541064518000419881, 2.621784821874995952 ) ) ;
#50941 = CARTESIAN_POINT ( 'NONE',  ( 29.43750000000000000, 5.773502691896255534, 3.535250795749688894E-16 ) ) ;
#50942 = CARTESIAN_POINT ( 'NONE',  ( 11.43750000122903465, 6.123233995736764310E-16, -4.999999999999998224 ) ) ;
#50943 = CARTESIAN_POINT ( 'NONE',  ( 10.05937500061451750, 0.000000000000000000, 4.756430356249998326 ) ) ;
#50944 = CARTESIAN_POINT ( 'NONE',  ( 29.85937500061451644, 0.000000000000000000, 5.243569643749999010 ) ) ;
#50945 = CARTESIAN_POINT ( 'NONE',  ( -2.828200636599751609E-16, 11.45000000122903394, -34.61880215351700230 ) ) ;
#50946 = CARTESIAN_POINT ( 'NONE',  ( 4.243569643749999898, 18.69687500061451857, -27.54997392385601529 ) ) ;
#50947 = EDGE_CURVE ( 'NONE', #60892, #13717, #5333, .T. ) ;
#50948 = CARTESIAN_POINT ( 'NONE',  ( 6.675000001229034474, 2.886751345948126879, 4.999999999999999112 ) ) ;
#50949 = PRODUCT_DEFINITION_FORMATION_WITH_SPECIFIED_SOURCE ( 'ANY', '', #45592, .NOT_KNOWN. ) ;
#50950 = CARTESIAN_POINT ( 'NONE',  ( 8.025000000000000355, -4.330127018922194537, 2.499999999999995559 ) ) ;
#50951 = CARTESIAN_POINT ( 'NONE',  ( 3.075000001229035718, 2.886751345948126879, 4.999999999999999112 ) ) ;
#50952 = CARTESIAN_POINT ( 'NONE',  ( 12.94687500061451857, -3.027376345333610441, -5.243569643749999898 ) ) ;
#50953 = CARTESIAN_POINT ( 'NONE',  ( 4.734375000614518214, -4.541064518000419881, 2.621784821874995952 ) ) ;
#50954 = CARTESIAN_POINT ( 'NONE',  ( 0.000000000000000000, 27.50000000000000000, 30.00000000000000000 ) ) ;
#50955 = CARTESIAN_POINT ( 'NONE',  ( 24.24375000122903145, -2.886751345948143310, 4.999999999999972466 ) ) ;
#50956 = CARTESIAN_POINT ( 'NONE',  ( 9.421875000614519990, 3.027376345333613106, -5.243569643749998122 ) ) ;
#50957 = PLANE ( 'NONE',  #50173 ) ;
#50958 = CARTESIAN_POINT ( 'NONE',  ( 4.537500001229034297, -4.330127018922194537, 2.499999999999995559 ) ) ;
#50959 = CARTESIAN_POINT ( 'NONE',  ( 4.243569643749999898, 16.87812500061459176, 30.00000000000000000 ) ) ;
#50960 = CARTESIAN_POINT ( 'NONE',  ( 21.38437500061451502, -4.541064518000419881, 2.621784821874995952 ) ) ;
#50961 =( BOUNDED_CURVE ( )  B_SPLINE_CURVE ( 2, ( #38258, #53801, #3564, #32728, #21264, #26455, #48995 ),
 .UNSPECIFIED., .F., .F. ) 
 B_SPLINE_CURVE_WITH_KNOTS ( ( 3, 2, 2, 3 ),
 ( 0.5600000000000000533, 0.5633333333333333526, 0.5666666666666667629, 0.5700000000000000622 ),
 .UNSPECIFIED. ) 
 CURVE ( )  GEOMETRIC_REPRESENTATION_ITEM ( )  RATIONAL_B_SPLINE_CURVE ( ( 1.000000000000000000, 0.8660254037844387076, 1.000000000000000000, 0.8660254037844387076, 1.000000000000000000, 0.8660254037844342667, 1.000000000000004441 ) ) 
 REPRESENTATION_ITEM ( '' )  );
#50962 = CARTESIAN_POINT ( 'NONE',  ( 2.733878782416514941, -4.186395442746991158, 2.733878782416514941 ) ) ;
#50963 = CARTESIAN_POINT ( 'NONE',  ( 27.18750000122903288, 6.123233995736764310E-16, -4.999999999999998224 ) ) ;
#50964 = CARTESIAN_POINT ( 'NONE',  ( 17.18437500061451573, -2.746126346562646425, 4.756430356249996549 ) ) ;
#50965 = CARTESIAN_POINT ( 'NONE',  ( 21.92812500061451431, 6.421520780324663323E-16, -5.243569643749999010 ) ) ;
#50966 = CARTESIAN_POINT ( 'NONE',  ( 15.96562500061451573, -6.054752690667223547, -1.112240025338166033E-15 ) ) ;
#50967 = CARTESIAN_POINT ( 'NONE',  ( 27.00937500061451502, 2.746126346562643317, 4.756430356249998326 ) ) ;
#50968 = CARTESIAN_POINT ( 'NONE',  ( 11.33437500061451608, 4.541064518000418104, 2.621784821874999949 ) ) ;
#50969 = CARTESIAN_POINT ( 'NONE',  ( 27.82499999999999929, -4.330127018922194537, 2.499999999999995559 ) ) ;
#50970 = CARTESIAN_POINT ( 'NONE',  ( 24.82500000122902861, -5.773502691896255534, -1.060575238724906372E-15 ) ) ;
#50971 = CARTESIAN_POINT ( 'NONE',  ( 3.496875000614518836, -3.027376345333610441, -5.243569643749999898 ) ) ;
#50972 = CARTESIAN_POINT ( 'NONE',  ( 13.73437500061451821, -4.541064518000419881, 2.621784821874995952 ) ) ;
#50973 = CARTESIAN_POINT ( 'NONE',  ( 28.58437500061451786, -4.541064518000419881, 2.621784821874995952 ) ) ;
#50974 = CARTESIAN_POINT ( 'NONE',  ( 15.65625000122903465, 0.000000000000000000, 4.999999999999998224 ) ) ;
#50975 = CARTESIAN_POINT ( 'NONE',  ( 22.88437500061451857, 6.421520780324663323E-16, -5.243569643749999010 ) ) ;
#50976 = CARTESIAN_POINT ( 'NONE',  ( 14.97187500061451892, 3.027376345333611329, 5.243569643749999010 ) ) ;
#50977 = CARTESIAN_POINT ( 'NONE',  ( -1.878215178125001827, 16.65312499938548285, 33.25316411605952283 ) ) ;
#50978 = CARTESIAN_POINT ( 'NONE',  ( 26.73749999999999716, 5.773502691896255534, 3.535250795749688894E-16 ) ) ;
#50979 = CARTESIAN_POINT ( 'NONE',  ( 2.812500001229033320, -4.330127018922190985, -2.500000000000001332 ) ) ;
#50980 = CARTESIAN_POINT ( 'NONE',  ( 29.85937500061451644, 0.000000000000000000, 4.756430356249998326 ) ) ;
#50981 = CARTESIAN_POINT ( 'NONE',  ( 16.30312500061451786, 0.000000000000000000, 5.243569643749999010 ) ) ;
#50982 = CARTESIAN_POINT ( 'NONE',  ( 6.187500000000002665, -2.886751345948129988, 4.999999999999997335 ) ) ;
#50983 = CARTESIAN_POINT ( 'NONE',  ( -5.810221930991193690E-16, 11.78749999999999964, -34.00000000000000000 ) ) ;
#50984 = CARTESIAN_POINT ( 'NONE',  ( 18.07499999999999929, 6.123233995736764310E-16, -4.999999999999998224 ) ) ;
#50985 = CARTESIAN_POINT ( 'NONE',  ( -4.243569643749999898, 13.50312500061451715, 30.00000000000000000 ) ) ;
#50986 = CARTESIAN_POINT ( 'NONE',  ( 0.6522905807966048464, 20.75364847883808395, 33.69936292076899065 ) ) ;
#50987 = CARTESIAN_POINT ( 'NONE',  ( 21.22500000122903074, -5.773502691896255534, -1.060575238724906372E-15 ) ) ;
#50988 = CARTESIAN_POINT ( 'NONE',  ( 2.516621263038625322, 9.679961675009989719, 24.54971018585778353 ) ) ;
#50989 = CARTESIAN_POINT ( 'NONE',  ( 26.22187500061451715, 3.027376345333611329, 5.243569643749999010 ) ) ;
#50990 = ORIENTED_EDGE ( 'NONE', *, *, #25676, .T. ) ;
#50991 = CARTESIAN_POINT ( 'NONE',  ( 21.81562500061451004, -6.054752690667223547, -1.112240025338166033E-15 ) ) ;
#50992 = CARTESIAN_POINT ( 'NONE',  ( 21.38437500061451502, -4.541064518000419881, 2.621784821874995952 ) ) ;
#50993 = CARTESIAN_POINT ( 'NONE',  ( 5.400000000000002132, -4.330127018922190985, -2.500000000000001332 ) ) ;
#50994 = CARTESIAN_POINT ( 'NONE',  ( 9.778125000614517504, 6.421520780324663323E-16, -5.243569643749999010 ) ) ;
#50995 = CARTESIAN_POINT ( 'NONE',  ( 23.50312500061451360, 0.000000000000000000, 5.243569643749999010 ) ) ;
#50996 = CARTESIAN_POINT ( 'NONE',  ( 13.05937500061451750, 4.541064518000418104, -2.621784821874998173 ) ) ;
#50997 = CARTESIAN_POINT ( 'NONE',  ( 15.72187500061451892, 3.027376345333613106, -5.243569643749998122 ) ) ;
#50998 = CARTESIAN_POINT ( 'NONE',  ( 20.66250000122903074, 0.000000000000000000, 4.999999999999998224 ) ) ;
#50999 = CARTESIAN_POINT ( 'NONE',  ( 4.243569643749999898, 16.42812500061451786, 30.00000000000000000 ) ) ;
#51000 = CARTESIAN_POINT ( 'NONE',  ( 20.25000000122903288, -2.886751345948129988, 4.999999999999997335 ) ) ;
#51001 = CARTESIAN_POINT ( 'NONE',  ( 14.52187500061451786, 2.746126346562643317, 4.756430356249998326 ) ) ;
#51002 = CARTESIAN_POINT ( 'NONE',  ( 11.50312500061451892, -4.541064518000417216, -2.621784821875001281 ) ) ;
#51003 = CARTESIAN_POINT ( 'NONE',  ( 5.746875000614517504, -3.027376345333610441, -5.243569643749999898 ) ) ;
#51004 = CARTESIAN_POINT ( 'NONE',  ( 5.859375000614519102, 4.541064518000418104, -2.621784821874998173 ) ) ;
#51005 = ORIENTED_EDGE ( 'NONE', *, *, #14215, .T. ) ;
#51006 = EDGE_CURVE ( 'NONE', #41736, #58199, #27978, .T. ) ;
#51007 = CARTESIAN_POINT ( 'NONE',  ( 25.77187500061451075, 3.027376345333611329, 5.243569643749999010 ) ) ;
#51008 = CARTESIAN_POINT ( 'NONE',  ( 16.19062500061451715, 6.054752690667223547, 3.707466751127219781E-16 ) ) ;
#51009 = CARTESIAN_POINT ( 'NONE',  ( 26.92500000122903359, 2.886751345948126879, 4.999999999999999112 ) ) ;
#51010 = CARTESIAN_POINT ( 'NONE',  ( 26.69062500061451715, -3.027376345333614438, 5.243569643749998122 ) ) ;
#51011 = AXIS2_PLACEMENT_3D ( 'NONE', #59262, #8671, #58530 ) ;
#51012 = CARTESIAN_POINT ( 'NONE',  ( 21.64687500061451786, 6.054752690667223547, 3.707466751127219781E-16 ) ) ;
#51013 = CARTESIAN_POINT ( 'NONE',  ( 16.26562500061451289, 3.027376345333611329, 5.243569643749999010 ) ) ;
#51014 = CARTESIAN_POINT ( 'NONE',  ( 4.000000000000000000, 10.73750000000000071, 32.30940107675849049 ) ) ;
#51015 = CARTESIAN_POINT ( 'NONE',  ( 21.02812500061451573, 6.421520780324663323E-16, -5.243569643749999010 ) ) ;
#51016 = CARTESIAN_POINT ( 'NONE',  ( 3.862500001229035362, 4.330127018922192761, -2.499999999999997780 ) ) ;
#51017 = ORIENTED_EDGE ( 'NONE', *, *, #40621, .T. ) ;
#51018 = CARTESIAN_POINT ( 'NONE',  ( 28.87499999999999645, 6.123233995736764310E-16, -4.999999999999998224 ) ) ;
#51019 = CARTESIAN_POINT ( 'NONE',  ( -3.999999999999997335, 11.93750000000000355, -27.69059892324149175 ) ) ;
#51020 = CARTESIAN_POINT ( 'NONE',  ( 3.756430356249998770, 16.31562499938548427, 32.16877607737302469 ) ) ;
#51021 = CARTESIAN_POINT ( 'NONE',  ( 3.121875000614518836, 3.027376345333613106, -5.243569643749998122 ) ) ;
#51022 = CARTESIAN_POINT ( 'NONE',  ( 10.19062500061451892, -3.027376345333610441, -5.243569643749999898 ) ) ;
#51023 = CARTESIAN_POINT ( 'NONE',  ( 21.11250000122903359, 0.000000000000000000, 4.999999999999998224 ) ) ;
#51024 =( BOUNDED_CURVE ( )  B_SPLINE_CURVE ( 2, ( #4664, #67454, #39009 ),
 .UNSPECIFIED., .F., .F. ) 
 B_SPLINE_CURVE_WITH_KNOTS ( ( 3, 3 ),
 ( 0.9861111111111111605, 0.9876227203420996359 ),
 .UNSPECIFIED. ) 
 CURVE ( )  GEOMETRIC_REPRESENTATION_ITEM ( )  RATIONAL_B_SPLINE_CURVE ( ( 0.9330127018922194093, 0.9330127018922197424, 0.9401540307732418889 ) ) 
 REPRESENTATION_ITEM ( '' )  );
#51025 = CARTESIAN_POINT ( 'NONE',  ( 13.69687500061451679, -3.027376345333614438, 5.243569643749998122 ) ) ;
#51026 = CARTESIAN_POINT ( 'NONE',  ( 27.10312500061451502, 0.000000000000000000, 5.243569643749999010 ) ) ;
#51027 = CARTESIAN_POINT ( 'NONE',  ( 28.61249999999999716, 2.886751345948126879, 4.999999999999999112 ) ) ;
#51028 = CARTESIAN_POINT ( 'NONE',  ( 8.484601909799253346E-16, 18.87500000122903643, -25.38119784648299770 ) ) ;
#51029 = CARTESIAN_POINT ( 'NONE',  ( 2.393811435568372112E-14, 17.28124999877096712, 34.00000000000000000 ) ) ;
#51030 = CARTESIAN_POINT ( 'NONE',  ( 12.17812500061451608, 4.541064518000418104, 2.621784821874999949 ) ) ;
#51031 = EDGE_LOOP ( 'NONE', ( #39353, #51160, #20296, #55811 ) ) ;
#51032 = CARTESIAN_POINT ( 'NONE',  ( 10.56562500061451715, -6.054752690667223547, -1.112240025338166033E-15 ) ) ;
#51033 = CARTESIAN_POINT ( 'NONE',  ( 6.853125000614516793, 0.000000000000000000, 5.243569643749999010 ) ) ;
#51034 = CARTESIAN_POINT ( 'NONE',  ( 16.58437500061451786, 5.824947211148865298E-16, -4.756430356249998326 ) ) ;
#51035 = CARTESIAN_POINT ( 'NONE',  ( 14.68125000122903323, 4.330127018922191873, 2.499999999999999556 ) ) ;
#51036 = CARTESIAN_POINT ( 'NONE',  ( 16.46249999999999503, 2.886751345948126879, 4.999999999999999112 ) ) ;
#51037 =( BOUNDED_CURVE ( )  B_SPLINE_CURVE ( 2, ( #42381, #47924, #24285, #70453, #52729, #47191, #14293 ),
 .UNSPECIFIED., .F., .F. ) 
 B_SPLINE_CURVE_WITH_KNOTS ( ( 3, 2, 2, 3 ),
 ( 0.9083333333333334370, 0.9111111111111112049, 0.9138888888888888618, 0.9166666666666666297 ),
 .UNSPECIFIED. ) 
 CURVE ( )  GEOMETRIC_REPRESENTATION_ITEM ( )  RATIONAL_B_SPLINE_CURVE ( ( 0.9999999999999946709, 0.8660254037844440367, 1.000000000000000000, 0.8660254037844387076, 1.000000000000000000, 0.8660254037844387076, 1.000000000000000000 ) ) 
 REPRESENTATION_ITEM ( '' )  );
#51038 = CARTESIAN_POINT ( 'NONE',  ( 17.07187500061451502, 3.027376345333613106, -5.243569643749998122 ) ) ;
#51039 = CARTESIAN_POINT ( 'NONE',  ( 10.91250000122903252, -4.330127018922190985, -2.500000000000001332 ) ) ;
#51040 = CARTESIAN_POINT ( 'NONE',  ( 19.32187500061451857, 3.027376345333613106, -5.243569643749998122 ) ) ;
#51041 = CARTESIAN_POINT ( 'NONE',  ( 18.71249999999999858, 2.886751345948126879, 4.999999999999999112 ) ) ;
#51042 = CARTESIAN_POINT ( 'NONE',  ( 19.77187500061451786, 3.027376345333613106, -5.243569643749998122 ) ) ;
#51043 = CARTESIAN_POINT ( 'NONE',  ( 4.243569643749999898, 15.07812500061451644, -30.00000000000000000 ) ) ;
#51044 = CARTESIAN_POINT ( 'NONE',  ( 0.000000000000000000, 20.00000000000000000, 30.00000000000000000 ) ) ;
#51045 = CARTESIAN_POINT ( 'NONE',  ( 26.03437500061451360, 5.492252693125287522, 3.363034840372157021E-16 ) ) ;
#51046 = CARTESIAN_POINT ( 'NONE',  ( 4.155299848256742479, 2.780943907573066198, 4.445394570867353679 ) ) ;
#51047 = ADVANCED_FACE ( 'NONE', ( #27433 ), #11163, .F. ) ;
#51048 = CARTESIAN_POINT ( 'NONE',  ( 26.72812500061451502, -4.541064518000419881, 2.621784821874995952 ) ) ;
#51049 = CARTESIAN_POINT ( 'NONE',  ( 29.37187500061451928, 3.027376345333611329, 5.243569643749999010 ) ) ;
#51050 = CARTESIAN_POINT ( 'NONE',  ( 25.23749999999999716, -2.886751345948125991, -5.000000000000000000 ) ) ;
#51051 = CARTESIAN_POINT ( 'NONE',  ( 8.278125000614515727, -4.541064518000419881, 2.621784821874995952 ) ) ;
#51052 = AXIS2_PLACEMENT_3D ( 'NONE', #43972, #72398, #15874 ) ;
#51053 = CARTESIAN_POINT ( 'NONE',  ( 24.98437500061451289, -2.746126346562642428, -4.756430356249999214 ) ) ;
#51054 =( BOUNDED_CURVE ( )  B_SPLINE_CURVE ( 2, ( #15021, #37926, #32756, #26482, #37559, #71918, #49023 ),
 .UNSPECIFIED., .F., .F. ) 
 B_SPLINE_CURVE_WITH_KNOTS ( ( 3, 2, 2, 3 ),
 ( 0.1499999999999999389, 0.1527777777777777624, 0.1555555555555555858, 0.1583333333333333814 ),
 .UNSPECIFIED. ) 
 CURVE ( )  GEOMETRIC_REPRESENTATION_ITEM ( )  RATIONAL_B_SPLINE_CURVE ( ( 1.000000000000002665, 0.8660254037844360431, 1.000000000000000000, 0.8660254037844387076, 1.000000000000000000, 0.8660254037844360431, 1.000000000000002665 ) ) 
 REPRESENTATION_ITEM ( '' )  );
#51055 = CARTESIAN_POINT ( 'NONE',  ( 19.35937500061451644, 4.541064518000418104, -2.621784821874998173 ) ) ;
#51056 = CARTESIAN_POINT ( 'NONE',  ( 11.22187500061451537, 4.119189519843966529, 2.378215178124999607 ) ) ;
#51057 = CARTESIAN_POINT ( 'NONE',  ( 6.403125000614517504, 0.000000000000000000, 5.243569643749999010 ) ) ;
#51058 = CARTESIAN_POINT ( 'NONE',  ( 10.17187500061451999, -6.054752690667223547, -1.112240025338166033E-15 ) ) ;
#51059 = ORIENTED_EDGE ( 'NONE', *, *, #30907, .F. ) ;
#51060 = CARTESIAN_POINT ( 'NONE',  ( 21.98437500061451644, 6.421520780324663323E-16, -5.243569643749999010 ) ) ;
#51061 = CARTESIAN_POINT ( 'NONE',  ( 45.00000000000000000, 2.500000000000000444, 5.500000000000000000 ) ) ;
#51062 = CARTESIAN_POINT ( 'NONE',  ( 3.149999999999999911, -4.330127018922190985, -2.500000000000001332 ) ) ;
#51063 = CARTESIAN_POINT ( 'NONE',  ( 15.30000000122903359, -2.886751345948129988, 4.999999999999997335 ) ) ;
#51064 = CARTESIAN_POINT ( 'NONE',  ( 18.09375000122903288, -2.886751345948126435, -5.000000000000000000 ) ) ;
#51065 = CARTESIAN_POINT ( 'NONE',  ( 18.63749999999999929, 5.773502691896255534, 3.535250795749688401E-16 ) ) ;
#51066 = ORIENTED_EDGE ( 'NONE', *, *, #33488, .F. ) ;
#51067 = CARTESIAN_POINT ( 'NONE',  ( 13.27500000000000213, 4.330127018922191873, 2.499999999999999556 ) ) ;
#51068 = CARTESIAN_POINT ( 'NONE',  ( 23.61562500061451431, -6.054752690667223547, -1.112240025338166033E-15 ) ) ;
#51069 = CARTESIAN_POINT ( 'NONE',  ( 15.00000000000000000, 4.330127018922192761, -2.499999999999997780 ) ) ;
#51070 = CARTESIAN_POINT ( 'NONE',  ( 9.412500001229034297, 0.000000000000000000, 4.999999999999998224 ) ) ;
#51071 = CARTESIAN_POINT ( 'NONE',  ( 7.865625000614516971, -6.054752690667223547, -1.112240025338166033E-15 ) ) ;
#51072 = CARTESIAN_POINT ( 'NONE',  ( 9.975000000000001421, 6.123233995736764310E-16, -4.999999999999998224 ) ) ;
#51073 = DIRECTION ( 'NONE',  ( 0.000000000000000000, 0.000000000000000000, 1.000000000000000000 ) ) ;
#51074 = CARTESIAN_POINT ( 'NONE',  ( -2.121784821874999949, 14.83437500061451786, -33.67503911421598417 ) ) ;
#51075 = CARTESIAN_POINT ( 'NONE',  ( 26.85000000122903430, 5.773502691896255534, 3.535250795749688894E-16 ) ) ;
#51076 = CARTESIAN_POINT ( 'NONE',  ( 3.756430356250000546, 17.62812499938548427, 27.83122392262697886 ) ) ;
#51077 = CARTESIAN_POINT ( 'NONE',  ( 7.275000000000000355, 6.123233995736764310E-16, -4.999999999999998224 ) ) ;
#51078 = LINE ( 'NONE', #9556, #62116 ) ;
#51079 = ORIENTED_EDGE ( 'NONE', *, *, #56586, .T. ) ;
#51080 = CARTESIAN_POINT ( 'NONE',  ( 22.86562500061451431, 3.027376345333613106, -5.243569643749998122 ) ) ;
#51081 = CARTESIAN_POINT ( 'NONE',  ( 28.41562500061451502, 3.027376345333611329, 5.243569643749999010 ) ) ;
#51082 = CARTESIAN_POINT ( 'NONE',  ( 29.85937500061451644, 0.000000000000000000, 5.243569643749999010 ) ) ;
#51083 = CARTESIAN_POINT ( 'NONE',  ( 19.77187500061451786, 3.027376345333613106, -5.243569643749998122 ) ) ;
#51084 = CARTESIAN_POINT ( 'NONE',  ( 16.56562500061451715, 3.027376345333613106, -5.243569643749998122 ) ) ;
#51085 = EDGE_CURVE ( 'NONE', #19994, #47876, #39729, .T. ) ;
#51086 = CARTESIAN_POINT ( 'NONE',  ( 2.121784821874999061, 12.45312500061459460, -33.67503911421598417 ) ) ;
#51087 = CARTESIAN_POINT ( 'NONE',  ( 6.140625000614516438, -3.027376345333610441, -5.243569643749999898 ) ) ;
#51088 = CARTESIAN_POINT ( 'NONE',  ( 28.87500000122902932, -5.773502691896255534, -1.060575238724906372E-15 ) ) ;
#51089 = CARTESIAN_POINT ( 'NONE',  ( 21.64687500061451786, 5.492252693125287522, 3.363034840372157021E-16 ) ) ;
#51090 = CARTESIAN_POINT ( 'NONE',  ( 18.66562500061451502, -6.054752690667223547, -1.112240025338166033E-15 ) ) ;
#51091 = CARTESIAN_POINT ( 'NONE',  ( 24.95625000122903003, 4.330127018922192761, -2.499999999999997780 ) ) ;
#51092 = CARTESIAN_POINT ( 'NONE',  ( 3.262500001229035718, -4.330127018922190985, -2.500000000000001332 ) ) ;
#51093 = CARTESIAN_POINT ( 'NONE',  ( 12.38437500061451857, -4.541064518000419881, 2.621784821874995952 ) ) ;
#51094 = CARTESIAN_POINT ( 'NONE',  ( 12.42187500061451821, -6.054752690667223547, -1.112240025338166033E-15 ) ) ;
#51095 = CARTESIAN_POINT ( 'NONE',  ( 19.95937500061451786, 0.000000000000000000, 5.243569643749999010 ) ) ;
#51096 = ORIENTED_EDGE ( 'NONE', *, *, #13387, .T. ) ;
#51097 = CARTESIAN_POINT ( 'NONE',  ( 20.10000000000000142, 0.000000000000000000, 4.999999999999998224 ) ) ;
#51098 = CARTESIAN_POINT ( 'NONE',  ( 24.21562500061451573, 3.027376345333613106, -5.243569643749998122 ) ) ;
#51099 = EDGE_CURVE ( 'NONE', #54799, #49995, #57373, .T. ) ;
#51100 = CARTESIAN_POINT ( 'NONE',  ( 18.08437500061451431, 4.541064518000418104, 2.621784821874999949 ) ) ;
#51101 = CARTESIAN_POINT ( 'NONE',  ( 24.47812500061451502, -4.541064518000419881, 2.621784821874995952 ) ) ;
#51102 = CARTESIAN_POINT ( 'NONE',  ( 27.15000000000000213, 4.330127018922192761, -2.499999999999997780 ) ) ;
#51103 = CARTESIAN_POINT ( 'NONE',  ( -3.999999999999997335, 15.98750000000000249, 32.30940107675850470 ) ) ;
#51104 = CARTESIAN_POINT ( 'NONE',  ( 5.296875000614518214, -3.027376345333610441, -5.243569643749999898 ) ) ;
#51105 = CARTESIAN_POINT ( 'NONE',  ( 11.43750000122903465, 6.123233995736764310E-16, -4.999999999999998224 ) ) ;
#51106 = CARTESIAN_POINT ( 'NONE',  ( 7.462500001229035007, 4.330127018922192761, -2.499999999999997780 ) ) ;
#51107 = CARTESIAN_POINT ( 'NONE',  ( 21.22500000000000142, 6.123233995736764310E-16, -4.999999999999998224 ) ) ;
#51108 = CARTESIAN_POINT ( 'NONE',  ( 27.52500000122903145, -5.773502691896255534, -1.060575238724906372E-15 ) ) ;
#51109 = CARTESIAN_POINT ( 'NONE',  ( 1.999999999999997335, 17.76874999877096428, 33.46410161513775705 ) ) ;
#51110 = CARTESIAN_POINT ( 'NONE',  ( 15.58125000122903181, 4.330127018922191873, 2.499999999999999556 ) ) ;
#51111 = CARTESIAN_POINT ( 'NONE',  ( 11.93437500061451573, -4.541064518000419881, 2.621784821874995952 ) ) ;
#51112 = CARTESIAN_POINT ( 'NONE',  ( 1.626862140677534470E-15, 12.83750000000000213, 34.00000000000000000 ) ) ;
#51113 = CARTESIAN_POINT ( 'NONE',  ( 16.41562500061451857, -6.054752690667223547, -1.112240025338166033E-15 ) ) ;
#51114 = CARTESIAN_POINT ( 'NONE',  ( 13.28437500061451715, -4.541064518000419881, 2.621784821874995952 ) ) ;
#51115 = CARTESIAN_POINT ( 'NONE',  ( 5.728125000614515905, 6.421520780324663323E-16, -5.243569643749999010 ) ) ;
#51116 = CARTESIAN_POINT ( 'NONE',  ( 19.58437500061451786, -4.541064518000419881, 2.621784821874995952 ) ) ;
#51117 = CARTESIAN_POINT ( 'NONE',  ( 9.871875000614517504, 3.027376345333613106, -5.243569643749998122 ) ) ;
#51118 = CARTESIAN_POINT ( 'NONE',  ( 3.853125000614517681, -4.541064518000417216, -2.621784821875001281 ) ) ;
#51119 = FACE_OUTER_BOUND ( 'NONE', #20389, .T. ) ;
#51120 = CARTESIAN_POINT ( 'NONE',  ( 5.175000001229033586, 2.886751345948129099, -4.999999999999998224 ) ) ;
#51121 = CARTESIAN_POINT ( 'NONE',  ( 21.29062500061451502, -3.027376345333614438, 5.243569643749998122 ) ) ;
#51122 = ORIENTED_EDGE ( 'NONE', *, *, #15050, .F. ) ;
#51123 = CARTESIAN_POINT ( 'NONE',  ( 8.250000001229034652, -2.886751345948125991, -5.000000000000000000 ) ) ;
#51124 = CARTESIAN_POINT ( 'NONE',  ( 16.97812500061451502, 6.421520780324663323E-16, -5.243569643749999010 ) ) ;
#51125 = CARTESIAN_POINT ( 'NONE',  ( 14.12812500061451715, -4.541064518000419881, 2.621784821874995952 ) ) ;
#51126 = CARTESIAN_POINT ( 'NONE',  ( 25.35937500061451644, 0.000000000000000000, 4.756430356249998326 ) ) ;
#51127 = CARTESIAN_POINT ( 'NONE',  ( 13.50000000000000178, -4.330127018922190985, -2.500000000000001332 ) ) ;
#51128 = CARTESIAN_POINT ( 'NONE',  ( 9.862500001229033586, 0.000000000000000000, 4.999999999999998224 ) ) ;
#51129 = CARTESIAN_POINT ( 'NONE',  ( 6.628125000614517148, 6.421520780324663323E-16, -5.243569643749999010 ) ) ;
#51130 = CARTESIAN_POINT ( 'NONE',  ( 19.35000000122903430, -2.886751345948129988, 4.999999999999997335 ) ) ;
#51131 = CARTESIAN_POINT ( 'NONE',  ( 27.33750000000000213, -2.886751345948129988, 4.999999999999997335 ) ) ;
#51132 = CARTESIAN_POINT ( 'NONE',  ( -3.000416591977282496E-16, 11.64687500061451786, -34.90005215228797653 ) ) ;
#51133 = CARTESIAN_POINT ( 'NONE',  ( 4.512434258951183885, -2.153965711245202197, 4.548138340231743904 ) ) ;
#51134 = DIRECTION ( 'NONE',  ( -1.000000000000000000, -0.000000000000000000, -0.000000000000000000 ) ) ;
#51135 = CARTESIAN_POINT ( 'NONE',  ( 0.000000000000000000, 27.50000000000000000, 30.00000000000000000 ) ) ;
#51136 = CARTESIAN_POINT ( 'NONE',  ( 20.22187500061451715, 3.027376345333613106, -5.243569643749998122 ) ) ;
#51137 = DIRECTION ( 'NONE',  ( 0.000000000000000000, 0.000000000000000000, 1.000000000000000000 ) ) ;
#51138 = CARTESIAN_POINT ( 'NONE',  ( 16.11562500061451786, 3.027376345333613106, -5.243569643749998122 ) ) ;
#51139 = CARTESIAN_POINT ( 'NONE',  ( 11.56875000122903252, 2.886751345948126879, 4.999999999999999112 ) ) ;
#51140 = DIRECTION ( 'NONE',  ( -0.000000000000000000, -1.000000000000000000, -0.000000000000000000 ) ) ;
#51141 = CARTESIAN_POINT ( 'NONE',  ( 28.58437500061451786, -4.541064518000419881, 2.621784821874995952 ) ) ;
#51142 = CARTESIAN_POINT ( 'NONE',  ( 26.78437500061451360, -4.541064518000419881, 2.621784821874995952 ) ) ;
#51143 = CARTESIAN_POINT ( 'NONE',  ( 19.28437500061451360, 5.492252693125287522, 3.363034840372157021E-16 ) ) ;
#51144 = CARTESIAN_POINT ( 'NONE',  ( 12.14062500061451821, 6.054752690667223547, 3.707466751127219781E-16 ) ) ;
#51145 = CARTESIAN_POINT ( 'NONE',  ( 11.63437500061451857, 6.421520780324663323E-16, -5.243569643749999010 ) ) ;
#51146 = VERTEX_POINT ( 'NONE', #33688 ) ;
#51147 = CARTESIAN_POINT ( 'NONE',  ( 9.525000000000002132, 6.123233995736764310E-16, -4.999999999999998224 ) ) ;
#51148 = CARTESIAN_POINT ( 'NONE',  ( 19.15312500061451573, -4.541064518000417216, -2.621784821875001281 ) ) ;
#51149 = CARTESIAN_POINT ( 'NONE',  ( 27.93749999999999645, -2.886751345948112224, -5.000000000000023981 ) ) ;
#51150 = CARTESIAN_POINT ( 'NONE',  ( 3.242103837493086330E-14, 12.80000000122903536, 26.00000000000000711 ) ) ;
#51151 = CARTESIAN_POINT ( 'NONE',  ( 11.84999999999999964, 4.330127018922192761, -2.499999999999997780 ) ) ;
#51152 = CARTESIAN_POINT ( 'NONE',  ( 21.52500000122903145, 2.886751345948126879, 4.999999999999999112 ) ) ;
#51153 = CARTESIAN_POINT ( 'NONE',  ( 15.40312500061451573, 0.000000000000000000, 5.243569643749999010 ) ) ;
#51154 = CARTESIAN_POINT ( 'NONE',  ( 13.24687500061451750, -4.119189519843965641, -2.378215178125001383 ) ) ;
#51155 = EDGE_LOOP ( 'NONE', ( #49973, #13148, #65438, #49826 ) ) ;
#51156 = CARTESIAN_POINT ( 'NONE',  ( 19.65000000000000213, 0.000000000000000000, 4.999999999999998224 ) ) ;
#51157 = CARTESIAN_POINT ( 'NONE',  ( 21.75000000000000000, 4.330127018922192761, -2.499999999999997780 ) ) ;
#51158 = CARTESIAN_POINT ( 'NONE',  ( 20.48437500061451289, -4.541064518000419881, 2.621784821874995952 ) ) ;
#51159 = CARTESIAN_POINT ( 'NONE',  ( 24.77812500061451217, 4.541064518000418104, 2.621784821874999949 ) ) ;
#51160 = ORIENTED_EDGE ( 'NONE', *, *, #8691, .T. ) ;
#51161 = ADVANCED_FACE ( 'NONE', ( #28161 ), #71777, .T. ) ;
#51162 = CARTESIAN_POINT ( 'NONE',  ( 13.68750000000000000, 5.773502691896255534, 3.535250795749688401E-16 ) ) ;
#51163 = CARTESIAN_POINT ( 'NONE',  ( 8.690625000614515372, -3.027376345333614438, 5.243569643749998122 ) ) ;
#51164 = CARTESIAN_POINT ( 'NONE',  ( -5.810221930991193690E-16, 12.23750000000000071, 26.00000000000000355 ) ) ;
#51165 = CARTESIAN_POINT ( 'NONE',  ( 14.51250000000000107, 2.886751345948129099, -4.999999999999998224 ) ) ;
#51166 = CARTESIAN_POINT ( 'NONE',  ( -2.121784821874996840, 17.62812500061451715, 33.67503911421598417 ) ) ;
#51167 = CARTESIAN_POINT ( 'NONE',  ( 28.60312500061451502, -4.541064518000417216, -2.621784821875001281 ) ) ;
#51168 = CARTESIAN_POINT ( 'NONE',  ( 27.12187500061451573, 3.027376345333611329, 5.243569643749999010 ) ) ;
#51169 = ORIENTED_EDGE ( 'NONE', *, *, #5968, .T. ) ;
#51170 = CARTESIAN_POINT ( 'NONE',  ( 22.86562500061451431, 3.027376345333613106, -5.243569643749998122 ) ) ;
#51171 = CARTESIAN_POINT ( 'NONE',  ( 25.39687500061451431, -3.027376345333614438, 5.243569643749998122 ) ) ;
#51172 = CARTESIAN_POINT ( 'NONE',  ( -3.000416591977282496E-16, 18.34062500061459389, -34.90005215228797653 ) ) ;
#51173 = CARTESIAN_POINT ( 'NONE',  ( 11.55000000000000071, 0.000000000000000000, 4.999999999999998224 ) ) ;
#51174 = CARTESIAN_POINT ( 'NONE',  ( 8.578125000614518214, 4.541064518000418104, 2.621784821874999949 ) ) ;
#51175 = CARTESIAN_POINT ( 'NONE',  ( 29.40937500061451715, 0.000000000000000000, 4.756430356249998326 ) ) ;
#51176 = CARTESIAN_POINT ( 'NONE',  ( 4.000000000000000000, 11.18750000000000178, 32.30940107675849760 ) ) ;
#51177 = CARTESIAN_POINT ( 'NONE',  ( 27.36562500061451786, 3.027376345333612662, -5.243569643749998122 ) ) ;
#51178 = CARTESIAN_POINT ( 'NONE',  ( -1.071796769724487453, 18.10759618943233207, 26.00000000000000000 ) ) ;
#51179 = CARTESIAN_POINT ( 'NONE',  ( 11.70937500061451608, 4.119189519843966529, -2.378215178124998275 ) ) ;
#51180 = CARTESIAN_POINT ( 'NONE',  ( 18.45937500061451431, 4.541064518000418104, -2.621784821874998173 ) ) ;
#51181 = CARTESIAN_POINT ( 'NONE',  ( -4.243569643749999898, 13.55937500061451750, 30.00000000000000000 ) ) ;
#51182 = CARTESIAN_POINT ( 'NONE',  ( 18.30937500061451928, -4.541064518000417216, -2.621784821875001281 ) ) ;
#51183 = CARTESIAN_POINT ( 'NONE',  ( 27.72187500061451715, -6.054752690667223547, -1.112240025338166033E-15 ) ) ;
#51184 = CARTESIAN_POINT ( 'NONE',  ( -2.121784821874999949, 17.08437500061451786, 26.32496088578401938 ) ) ;
#51185 = CARTESIAN_POINT ( 'NONE',  ( 9.253125000614517148, -4.541064518000417216, -2.621784821875001281 ) ) ;
#51186 = FACE_OUTER_BOUND ( 'NONE', #60234, .T. ) ;
#51187 = EDGE_CURVE ( 'NONE', #39431, #36820, #31207, .T. ) ;
#51188 = CARTESIAN_POINT ( 'NONE',  ( 5.109375000614518214, 0.000000000000000000, 5.243569643749999010 ) ) ;
#51189 = CARTESIAN_POINT ( 'NONE',  ( 11.83125000122903181, 6.123233995736764310E-16, -4.999999999999998224 ) ) ;
#51190 = CARTESIAN_POINT ( 'NONE',  ( 8.503125000614515372, 4.541064518000418104, -2.621784821874998173 ) ) ;
#51191 = CARTESIAN_POINT ( 'NONE',  ( 12.42187500061451821, -6.054752690667223547, -1.112240025338166033E-15 ) ) ;
#51192 =( NAMED_UNIT ( * ) SI_UNIT ( $, .STERADIAN. ) SOLID_ANGLE_UNIT ( ) );
#51193 = CARTESIAN_POINT ( 'NONE',  ( 19.87500000122903288, -5.773502691896255534, -1.060575238724906372E-15 ) ) ;
#51194 = CARTESIAN_POINT ( 'NONE',  ( 5.746875000614517504, -3.027376345333610441, -5.243569643749999898 ) ) ;
#51195 = CARTESIAN_POINT ( 'NONE',  ( 7.640625000614517326, 6.054752690667223547, 3.707466751127219781E-16 ) ) ;
#51196 = CARTESIAN_POINT ( 'NONE',  ( 4.162500001229033408, -4.330127018922190985, -2.500000000000001332 ) ) ;
#51197 = CARTESIAN_POINT ( 'NONE',  ( 22.40625000122903288, 0.000000000000000000, 4.999999999999998224 ) ) ;
#51198 = CARTESIAN_POINT ( 'NONE',  ( 20.22187500061451715, 3.027376345333613106, -5.243569643749998122 ) ) ;
#51199 = CARTESIAN_POINT ( 'NONE',  ( -1.999999999999997113, 11.63750000122903394, 33.46410161513775705 ) ) ;
#51200 = ORIENTED_EDGE ( 'NONE', *, *, #19674, .T. ) ;
#51201 = CARTESIAN_POINT ( 'NONE',  ( 24.44062500061451715, -3.027376345333614438, 5.243569643749998122 ) ) ;
#51202 = CARTESIAN_POINT ( 'NONE',  ( 11.80312500061451608, 0.000000000000000000, 5.243569643749999010 ) ) ;
#51203 = CARTESIAN_POINT ( 'NONE',  ( 29.37187500061451928, 3.027376345333611329, 5.243569643749999010 ) ) ;
#51204 = CARTESIAN_POINT ( 'NONE',  ( 11.87812500061451537, -4.541064518000419881, 2.621784821874995952 ) ) ;
#51205 = CARTESIAN_POINT ( 'NONE',  ( 4.492182058117979437, -2.195518243313848039, -4.590536574672159809 ) ) ;
#51206 = ADVANCED_FACE ( 'NONE', ( #56214 ), #28143, .F. ) ;
#51207 =( BOUNDED_CURVE ( )  B_SPLINE_CURVE ( 2, ( #68032, #81, #39595, #17402, #4886, #68390, #50677 ),
 .UNSPECIFIED., .F., .F. ) 
 B_SPLINE_CURVE_WITH_KNOTS ( ( 3, 2, 2, 3 ),
 ( 0.5749999999999999556, 0.5777777777777777235, 0.5805555555555557135, 0.5833333333333334814 ),
 .UNSPECIFIED. ) 
 CURVE ( )  GEOMETRIC_REPRESENTATION_ITEM ( )  RATIONAL_B_SPLINE_CURVE ( ( 1.000000000000000000, 0.8660254037844387076, 1.000000000000000000, 0.8660254037844387076, 1.000000000000000000, 0.8660254037844333785, 1.000000000000005329 ) ) 
 REPRESENTATION_ITEM ( '' )  );
#51208 = CARTESIAN_POINT ( 'NONE',  ( 11.96250000122903501, 4.330127018922192761, -2.499999999999997780 ) ) ;
#51209 = CARTESIAN_POINT ( 'NONE',  ( 27.25312500061451360, -4.541064518000417216, -2.621784821875001281 ) ) ;
#51210 = CARTESIAN_POINT ( 'NONE',  ( -4.243569643749999898, 13.01562500061451999, -32.45002607614398471 ) ) ;
#51211 = CARTESIAN_POINT ( 'NONE',  ( 15.15000000122903323, 5.773502691896255534, 3.535250795749688894E-16 ) ) ;
#51212 = CARTESIAN_POINT ( 'NONE',  ( 10.80000000000000071, -4.330127018922190985, -2.500000000000001332 ) ) ;
#51213 = CARTESIAN_POINT ( 'NONE',  ( 21.06562500061451715, 3.027376345333613106, -5.243569643749998122 ) ) ;
#51214 = CARTESIAN_POINT ( 'NONE',  ( 8.371875000614515727, -6.054752690667223547, -1.112240025338166033E-15 ) ) ;
#51215 = CARTESIAN_POINT ( 'NONE',  ( 7.087500001229034119, 4.330127018922191873, 2.499999999999999556 ) ) ;
#51216 = CARTESIAN_POINT ( 'NONE',  ( 17.21250000122903145, -4.330127018922190985, -2.500000000000001332 ) ) ;
#51217 = CARTESIAN_POINT ( 'NONE',  ( 13.97812500061451679, 4.541064518000418104, 2.621784821874999949 ) ) ;
#51218 = CARTESIAN_POINT ( 'NONE',  ( 15.81562500061451537, 3.027376345333611329, 5.243569643749999010 ) ) ;
#51219 = CARTESIAN_POINT ( 'NONE',  ( 25.05000000122903714, 5.773502691896255534, 3.535250795749688894E-16 ) ) ;
#51220 = CARTESIAN_POINT ( 'NONE',  ( 20.92500000000000071, 4.330127018922191873, 2.499999999999999556 ) ) ;
#51221 = CARTESIAN_POINT ( 'NONE',  ( 22.80937500061451573, -4.541064518000417216, -2.621784821875001281 ) ) ;
#51222 = FACE_OUTER_BOUND ( 'NONE', #67159, .T. ) ;
#51223 = CARTESIAN_POINT ( 'NONE',  ( 9.712500001229033231, 4.330127018922192761, -2.499999999999997780 ) ) ;
#51224 = CARTESIAN_POINT ( 'NONE',  ( 27.42187500061451644, 3.027376345333613106, -5.243569643749998122 ) ) ;
#51225 = CARTESIAN_POINT ( 'NONE',  ( 45.00000000000000000, 0.000000000000000000, 0.000000000000000000 ) ) ;
#51226 = CARTESIAN_POINT ( 'NONE',  ( 23.61562500061451431, -6.054752690667223547, -1.112240025338166033E-15 ) ) ;
#51227 = CARTESIAN_POINT ( 'NONE',  ( 2.655984681222220721E-16, 15.11562499938548321, 25.66244784525396483 ) ) ;
#51228 = CARTESIAN_POINT ( 'NONE',  ( -1.071796769724489229, 14.11115380933862973, 34.00000000000000000 ) ) ;
#51229 = CARTESIAN_POINT ( 'NONE',  ( 8.671875000614518214, 3.027376345333611329, 5.243569643749999010 ) ) ;
#51230 = CARTESIAN_POINT ( 'NONE',  ( 16.01250000000000284, 2.886751345948060266, 5.000000000000114575 ) ) ;
#51231 = CARTESIAN_POINT ( 'NONE',  ( 27.40312500061451573, 4.541064518000418104, -2.621784821874998173 ) ) ;
#51232 = CARTESIAN_POINT ( 'NONE',  ( 6.496875000614517504, -3.027376345333614438, 5.243569643749998122 ) ) ;
#51233 = CARTESIAN_POINT ( 'NONE',  ( -1.487416814333745711E-14, 16.62500000122903288, -26.00000000000000000 ) ) ;
#51234 = CARTESIAN_POINT ( 'NONE',  ( 25.43437500061451573, -4.541064518000419881, 2.621784821874995952 ) ) ;
#51235 = CARTESIAN_POINT ( 'NONE',  ( -2.121784821874999949, 11.17812500061459602, 26.32496088578401938 ) ) ;
#51236 = CARTESIAN_POINT ( 'NONE',  ( 19.08750000000000213, 5.773502691896255534, 3.535250795749688894E-16 ) ) ;
#51237 = ORIENTED_EDGE ( 'NONE', *, *, #55966, .F. ) ;
#51238 = CARTESIAN_POINT ( 'NONE',  ( 26.36249999999999716, 2.886751345948126879, 4.999999999999999112 ) ) ;
#51239 =( BOUNDED_CURVE ( )  B_SPLINE_CURVE ( 3, ( #33243, #48785, #15877, #72401 ),
 .UNSPECIFIED., .F., .F. ) 
 B_SPLINE_CURVE_WITH_KNOTS ( ( 4, 4 ),
 ( 2.610771512460038579, 2.658599815149916612 ),
 .UNSPECIFIED. ) 
 CURVE ( )  GEOMETRIC_REPRESENTATION_ITEM ( )  RATIONAL_B_SPLINE_CURVE ( ( 1.000000000000000000, 0.9998093802064862423, 0.9998093802064862423, 1.000000000000000000 ) ) 
 REPRESENTATION_ITEM ( '' )  );
#51240 = CARTESIAN_POINT ( 'NONE',  ( 28.24687500061451573, -3.027376345333610441, -5.243569643749999898 ) ) ;
#51241 = EDGE_LOOP ( 'NONE', ( #38145, #36925, #27527, #21925 ) ) ;
#51242 = CARTESIAN_POINT ( 'NONE',  ( 14.76562500061451821, 3.027376345333613106, -5.243569643749998122 ) ) ;
#51243 = CARTESIAN_POINT ( 'NONE',  ( 7.865625000614516971, -6.054752690667223547, -1.112240025338166033E-15 ) ) ;
#51244 = CARTESIAN_POINT ( 'NONE',  ( 18.94687500061451857, 0.000000000000000000, 4.756430356249998326 ) ) ;
#51245 = CARTESIAN_POINT ( 'NONE',  ( 4.659375000614518925, 0.000000000000000000, 5.243569643749999010 ) ) ;
#51246 = CARTESIAN_POINT ( 'NONE',  ( 17.58750000122903145, -4.330127018922194537, 2.499999999999995559 ) ) ;
#51247 = CARTESIAN_POINT ( 'NONE',  ( 21.86250000000000071, 2.886751345948126879, 4.999999999999999112 ) ) ;
#51248 = CARTESIAN_POINT ( 'NONE',  ( 29.39999999999999858, 4.330127018922192761, -2.499999999999997780 ) ) ;
#51249 = CARTESIAN_POINT ( 'NONE',  ( 4.396875000614516971, -3.027376345333610441, -5.243569643749999898 ) ) ;
#51250 = CARTESIAN_POINT ( 'NONE',  ( 11.40937500061451892, 0.000000000000000000, 5.243569643749999010 ) ) ;
#51251 = CARTESIAN_POINT ( 'NONE',  ( 22.43437500061451573, 6.421520780324663323E-16, -5.243569643749999010 ) ) ;
#51252 = EDGE_CURVE ( 'NONE', #55622, #44045, #38778, .T. ) ;
#51253 = FACE_OUTER_BOUND ( 'NONE', #14812, .T. ) ;
#51254 = ORIENTED_EDGE ( 'NONE', *, *, #62210, .T. ) ;
#51255 = CARTESIAN_POINT ( 'NONE',  ( 3.534375000614518036, 6.421520780324663323E-16, -5.243569643749999010 ) ) ;
#51256 = CARTESIAN_POINT ( 'NONE',  ( 7.209375000614519635, 4.541064518000418104, -2.621784821874998173 ) ) ;
#51257 = CARTESIAN_POINT ( 'NONE',  ( 19.23749999999999716, -2.886751345948129988, 4.999999999999997335 ) ) ;
#51258 = CARTESIAN_POINT ( 'NONE',  ( 16.34062500061451573, -3.027376345333614438, 5.243569643749998122 ) ) ;
#51259 = CARTESIAN_POINT ( 'NONE',  ( -4.000000000000000000, 19.47499999999999787, 30.00000000000000000 ) ) ;
#51260 = FACE_OUTER_BOUND ( 'NONE', #31075, .T. ) ;
#51261 = CARTESIAN_POINT ( 'NONE',  ( 18.94687500061451502, 5.492252693125287522, 3.363034840372157021E-16 ) ) ;
#51262 = CARTESIAN_POINT ( 'NONE',  ( 9.853125000614516793, 4.541064518000418104, -2.621784821874998173 ) ) ;
#51263 = CARTESIAN_POINT ( 'NONE',  ( 25.65937500061451715, 4.541064518000418104, -2.621784821874998173 ) ) ;
#51264 = DIRECTION ( 'NONE',  ( -0.000000000000000000, -1.000000000000000000, -0.000000000000000000 ) ) ;
#51265 = CARTESIAN_POINT ( 'NONE',  ( 27.30937500061451573, -4.541064518000417216, -2.621784821875001281 ) ) ;
#51266 = CARTESIAN_POINT ( 'NONE',  ( 10.38750000000000107, -2.886751345948125991, -5.000000000000000000 ) ) ;
#51267 = CARTESIAN_POINT ( 'NONE',  ( 3.999999999999998668, 13.62500000122903288, 27.69059892324149175 ) ) ;
#51268 = CARTESIAN_POINT ( 'NONE',  ( 10.05000000122903181, -2.886751345948125991, -5.000000000000000000 ) ) ;
#51269 = CARTESIAN_POINT ( 'NONE',  ( 21.00937500061451857, -4.541064518000417216, -2.621784821875001281 ) ) ;
#51270 = CARTESIAN_POINT ( 'NONE',  ( 14.55937500061451573, 0.000000000000000000, 5.243569643749999010 ) ) ;
#51271 = CARTESIAN_POINT ( 'NONE',  ( -0.5556303621801368386, 4.970948098741851062, -33.96363479047759881 ) ) ;
#51272 = ORIENTED_EDGE ( 'NONE', *, *, #29804, .F. ) ;
#51273 = CARTESIAN_POINT ( 'NONE',  ( 15.29062500061451679, 6.054752690667223547, 3.707466751127219781E-16 ) ) ;
#51274 = CARTESIAN_POINT ( 'NONE',  ( 25.87500000122903288, 2.886751345948129099, -4.999999999999998224 ) ) ;
#51275 = CARTESIAN_POINT ( 'NONE',  ( 12.53437500061451537, 6.421520780324663323E-16, -5.243569643749999010 ) ) ;
#51276 = CARTESIAN_POINT ( 'NONE',  ( 3.680627977383744920, 9.304151242747316530, -34.75401982126012967 ) ) ;
#51277 = CARTESIAN_POINT ( 'NONE',  ( 17.31562500061451715, -6.054752690667223547, -1.112240025338166033E-15 ) ) ;
#51278 = CARTESIAN_POINT ( 'NONE',  ( 3.999999999999999112, 18.87500000000000000, -30.00000000000000000 ) ) ;
#51279 = CARTESIAN_POINT ( 'NONE',  ( 26.10937500061451644, 4.541064518000418104, -2.621784821874998173 ) ) ;
#51280 = CARTESIAN_POINT ( 'NONE',  ( 9.001249775931846008E-16, 10.01562500061451644, 34.90005215228797653 ) ) ;
#51281 = AXIS2_PLACEMENT_3D ( 'NONE', #1901, #42503, #7786 ) ;
#51282 = CARTESIAN_POINT ( 'NONE',  ( 12.33750000122903145, 6.123233995736764310E-16, -4.999999999999998224 ) ) ;
#51283 = DIRECTION ( 'NONE',  ( -1.000000000000000000, -0.000000000000000000, -0.000000000000000000 ) ) ;
#51284 = CARTESIAN_POINT ( 'NONE',  ( 4.243569643749999010, 17.87187500061451928, -32.45002607614398471 ) ) ;
#51285 = CARTESIAN_POINT ( 'NONE',  ( 17.44687500061451857, -3.027376345333610441, -5.243569643749999898 ) ) ;
#51286 = CARTESIAN_POINT ( 'NONE',  ( 21.22500000122903074, -5.773502691896255534, -1.060575238724906372E-15 ) ) ;
#51287 = CIRCLE ( 'NONE', #45548, 9.000000000000000000 ) ;
#51288 = CARTESIAN_POINT ( 'NONE',  ( 14.67187500061451821, -6.054752690667223547, -1.112240025338166033E-15 ) ) ;
#51289 = CARTESIAN_POINT ( 'NONE',  ( -4.243569643749999898, 9.921875000614519990, 27.54997392385601529 ) ) ;
#51290 = CARTESIAN_POINT ( 'NONE',  ( 21.37500000122902932, 2.886751345948129099, -4.999999999999998224 ) ) ;
#51291 = CARTESIAN_POINT ( 'NONE',  ( 14.16562500061451679, -6.054752690667223547, -1.112240025338166033E-15 ) ) ;
#51292 = DIRECTION ( 'NONE',  ( -1.000000000000000000, -0.000000000000000000, -0.000000000000000000 ) ) ;
#51293 = VERTEX_POINT ( 'NONE', #51029 ) ;
#51294 = ORIENTED_EDGE ( 'NONE', *, *, #23299, .F. ) ;
#51295 = CARTESIAN_POINT ( 'NONE',  ( 19.91250000000000142, 2.886751345948129099, -4.999999999999998224 ) ) ;
#51296 = CARTESIAN_POINT ( 'NONE',  ( 2.000000000000000444, 18.36874999877096570, 26.53589838486224650 ) ) ;
#51297 = CARTESIAN_POINT ( 'NONE',  ( 3.778125000614519280, -4.541064518000419881, 2.621784821874995952 ) ) ;
#51298 = CARTESIAN_POINT ( 'NONE',  ( 16.16250000122903430, 0.000000000000000000, 4.999999999999998224 ) ) ;
#51299 = CARTESIAN_POINT ( 'NONE',  ( 20.31562500061451715, 3.027376345333611329, 5.243569643749999010 ) ) ;
#51300 = CARTESIAN_POINT ( 'NONE',  ( 22.11562500061451786, 3.027376345333611329, 5.243569643749999010 ) ) ;
#51301 = CARTESIAN_POINT ( 'NONE',  ( 3.103125000614517237, 4.541064518000418104, -2.621784821874998173 ) ) ;
#51302 = CARTESIAN_POINT ( 'NONE',  ( 29.96250000000000213, 2.886751345948126879, 4.999999999999999112 ) ) ;
#51303 = CARTESIAN_POINT ( 'NONE',  ( 1.626862140677534273E-15, 11.67500000122903181, 34.00000000000000000 ) ) ;
#51304 = CARTESIAN_POINT ( 'NONE',  ( 8.821875000614518569, -5.492252693125287522, -1.008910452111647106E-15 ) ) ;
#51305 = CARTESIAN_POINT ( 'NONE',  ( -1.626862140677534273E-15, 17.78749999999999787, 34.00000000000000000 ) ) ;
#51306 = CARTESIAN_POINT ( 'NONE',  ( 3.999999999999999112, 11.78750000122903430, -30.00000000000000000 ) ) ;
#51307 = CARTESIAN_POINT ( 'NONE',  ( 2.121784821874999061, 18.80937500061451928, -33.67503911421598417 ) ) ;
#51308 = CARTESIAN_POINT ( 'NONE',  ( 7.087500001229034119, 4.330127018922191873, 2.499999999999999556 ) ) ;
#51309 = CARTESIAN_POINT ( 'NONE',  ( 7.987500000000000711, -2.886751345948129988, 4.999999999999997335 ) ) ;
#51310 = EDGE_CURVE ( 'NONE', #15563, #58630, #33579, .T. ) ;
#51311 = CARTESIAN_POINT ( 'NONE',  ( 4.237500001229036251, 6.123233995736764310E-16, -4.999999999999998224 ) ) ;
#51312 = CARTESIAN_POINT ( 'NONE',  ( 11.07187500061451679, -6.054752690667223547, -1.112240025338166033E-15 ) ) ;
#51313 = CARTESIAN_POINT ( 'NONE',  ( 19.50000000122903288, -2.886751345948126435, -5.000000000000000000 ) ) ;
#51314 = CARTESIAN_POINT ( 'NONE',  ( 3.721875000614518036, 3.027376345333611329, 5.243569643749999010 ) ) ;
#51315 = CARTESIAN_POINT ( 'NONE',  ( 1.999999999999998668, 19.06250000122903288, 26.53589838486224650 ) ) ;
#51316 = AXIS2_PLACEMENT_3D ( 'NONE', #31732, #19900, #41713 ) ;
#51317 = CARTESIAN_POINT ( 'NONE',  ( -2.000000000000000000, 19.58750000122903501, -33.46410161513775705 ) ) ;
#51318 = CARTESIAN_POINT ( 'NONE',  ( 11.18437500061451928, 6.421520780324663323E-16, -5.243569643749999010 ) ) ;
#51319 = CARTESIAN_POINT ( 'NONE',  ( 13.62187500061451750, 3.027376345333611329, 5.243569643749999010 ) ) ;
#51320 = CARTESIAN_POINT ( 'NONE',  ( 4.898587196589411843E-16, 20.00000000000000000, 33.99999999999999289 ) ) ;
#51321 = CARTESIAN_POINT ( 'NONE',  ( 7.575000000000001954, -4.330127018922194537, 2.499999999999995559 ) ) ;
#51322 = CARTESIAN_POINT ( 'NONE',  ( 4.243569643749999010, 17.81562500061459531, 27.54997392385601174 ) ) ;
#51323 = CARTESIAN_POINT ( 'NONE',  ( 20.93437500061451573, -4.541064518000419881, 2.621784821874995952 ) ) ;
#51324 =( LENGTH_UNIT ( ) NAMED_UNIT ( * ) SI_UNIT ( .MILLI., .METRE. ) );
#51325 = CARTESIAN_POINT ( 'NONE',  ( 27.26250000122903216, 4.330127018922192761, -2.499999999999997780 ) ) ;
#51326 = VECTOR ( 'NONE', #21711, 1000.000000000000000 ) ;
#51327 = CARTESIAN_POINT ( 'NONE',  ( 18.49687500061451573, 0.000000000000000000, 4.756430356249998326 ) ) ;
#51328 = CARTESIAN_POINT ( 'NONE',  ( 22.75312500061451360, -4.541064518000417216, -2.621784821875001281 ) ) ;
#51329 = CARTESIAN_POINT ( 'NONE',  ( 16.07812500061451289, 6.421520780324663323E-16, -5.243569643749999010 ) ) ;
#51330 = CARTESIAN_POINT ( 'NONE',  ( 25.43437500061451217, -2.746126346562642428, -4.756430356249999214 ) ) ;
#51331 = CARTESIAN_POINT ( 'NONE',  ( 12.00937500061451857, -4.541064518000417216, -2.621784821875001281 ) ) ;
#51332 = CARTESIAN_POINT ( 'NONE',  ( 27.41250000000000142, -5.773502691896255534, -1.060575238724906372E-15 ) ) ;
#51333 = CARTESIAN_POINT ( 'NONE',  ( 24.03750000122903430, 6.123233995736764310E-16, -4.999999999999998224 ) ) ;
#51334 = FACE_OUTER_BOUND ( 'NONE', #60500, .T. ) ;
#51335 = CARTESIAN_POINT ( 'NONE',  ( 10.88437500061451679, 4.541064518000418104, 2.621784821874999949 ) ) ;
#51336 = CARTESIAN_POINT ( 'NONE',  ( 29.14687500061451075, -3.027376345333610441, -5.243569643749999898 ) ) ;
#51337 = CARTESIAN_POINT ( 'NONE',  ( 4.096875000614518925, 6.054752690667223547, 3.707466751127219781E-16 ) ) ;
#51338 = CARTESIAN_POINT ( 'NONE',  ( -1.071796769724488563, 12.44240381056766864, -26.00000000000000000 ) ) ;
#51339 = CARTESIAN_POINT ( 'NONE',  ( 22.62187500061451573, 3.027376345333611329, 5.243569643749999010 ) ) ;
#51340 = CARTESIAN_POINT ( 'NONE',  ( 14.89687500061451786, 6.054752690667223547, 3.707466751127219781E-16 ) ) ;
#51341 = CARTESIAN_POINT ( 'NONE',  ( -1.878215178125001827, 18.00312499938548427, 33.25316411605952283 ) ) ;
#51342 = CARTESIAN_POINT ( 'NONE',  ( 26.92499999999999716, -4.330127018922194537, 2.499999999999995559 ) ) ;
#51343 = CARTESIAN_POINT ( 'NONE',  ( 4.500000001229034652, -2.886751345948129988, 4.999999999999997335 ) ) ;
#51344 = CARTESIAN_POINT ( 'NONE',  ( 26.22187500061451715, 2.746126346562643317, 4.756430356249998326 ) ) ;
#51345 = CARTESIAN_POINT ( 'NONE',  ( 17.95312500061451644, 4.541064518000418104, -2.621784821874998173 ) ) ;
#51346 = CARTESIAN_POINT ( 'NONE',  ( 5.924999999999999822, 6.123233995736764310E-16, -4.999999999999998224 ) ) ;
#51347 = CARTESIAN_POINT ( 'NONE',  ( 16.19999999999999929, -4.330127018922190985, -2.500000000000001332 ) ) ;
#51348 = CARTESIAN_POINT ( 'NONE',  ( 4.243569643749999898, 12.34062500061451750, 32.45002607614398471 ) ) ;
#51349 = CARTESIAN_POINT ( 'NONE',  ( 24.73125000122903216, -4.330127018922194537, 2.499999999999995559 ) ) ;
#51350 = CARTESIAN_POINT ( 'NONE',  ( 21.07500000122903572, 2.886751345948126879, 4.999999999999999112 ) ) ;
#51351 = CARTESIAN_POINT ( 'NONE',  ( 26.67187500061451644, 3.027376345333611329, 5.243569643749999010 ) ) ;
#51352 = VERTEX_POINT ( 'NONE', #7405 ) ;
#51353 = CARTESIAN_POINT ( 'NONE',  ( 22.52812500061451573, 4.541064518000418104, 2.621784821874999949 ) ) ;
#51354 = CARTESIAN_POINT ( 'NONE',  ( 23.07187500061451857, 3.027376345333611329, 5.243569643749999010 ) ) ;
#51355 = CARTESIAN_POINT ( 'NONE',  ( 4.050000000000001599, -4.330127018922190985, -2.500000000000001332 ) ) ;
#51356 = CARTESIAN_POINT ( 'NONE',  ( 6.253125000614517148, 4.541064518000418104, -2.621784821874998173 ) ) ;
#51357 = CARTESIAN_POINT ( 'NONE',  ( 24.62812500061451715, 6.421520780324663323E-16, -5.243569643749999010 ) ) ;
#51358 = CARTESIAN_POINT ( 'NONE',  ( 11.67187500061451821, 3.027376345333613106, -5.243569643749998122 ) ) ;
#51359 = CARTESIAN_POINT ( 'NONE',  ( 17.52187500061451431, 3.027376345333613106, -5.243569643749998122 ) ) ;
#51360 = CARTESIAN_POINT ( 'NONE',  ( -3.000416591977282496E-16, 17.44062500061451360, 25.09994784771203058 ) ) ;
#51361 = ADVANCED_FACE ( 'NONE', ( #41393 ), #34385, .F. ) ;
#51362 = CARTESIAN_POINT ( 'NONE',  ( 21.56250000122903288, 0.000000000000000000, 4.999999999999998224 ) ) ;
#51363 = CARTESIAN_POINT ( 'NONE',  ( 15.90937500061451892, 0.000000000000000000, 4.756430356249998326 ) ) ;
#51364 = CARTESIAN_POINT ( 'NONE',  ( 10.37812500061451715, 4.541064518000418104, 2.621784821874999949 ) ) ;
#51365 = CARTESIAN_POINT ( 'NONE',  ( 6.459375000614518747, 0.000000000000000000, 5.243569643749999010 ) ) ;
#51366 = CARTESIAN_POINT ( 'NONE',  ( 4.434375000614519280, 6.421520780324663323E-16, -5.243569643749999010 ) ) ;
#51367 = ORIENTED_EDGE ( 'NONE', *, *, #42313, .T. ) ;
#51368 = CARTESIAN_POINT ( 'NONE',  ( 25.20937500061451431, 4.541064518000418104, -2.621784821874998173 ) ) ;
#51369 = CARTESIAN_POINT ( 'NONE',  ( 18.10312500061451502, 0.000000000000000000, 5.243569643749999010 ) ) ;
#51370 = CARTESIAN_POINT ( 'NONE',  ( 26.51250000122903216, 0.000000000000000000, 4.999999999999998224 ) ) ;
#51371 = CARTESIAN_POINT ( 'NONE',  ( 27.81562500061452070, 3.027376345333613106, -5.243569643749998122 ) ) ;
#51372 = CARTESIAN_POINT ( 'NONE',  ( 20.70937500061451786, 4.541064518000418104, -2.621784821874998173 ) ) ;
#51373 = CARTESIAN_POINT ( 'NONE',  ( 16.04062500061451857, -3.027376345333610441, -5.243569643749999898 ) ) ;
#51374 = CARTESIAN_POINT ( 'NONE',  ( -3.000416591977282496E-16, 18.84687500061452070, 25.09994784771203058 ) ) ;
#51375 = VECTOR ( 'NONE', #18365, 1000.000000000000000 ) ;
#51376 = CARTESIAN_POINT ( 'NONE',  ( 22.07812500061451644, 4.541064518000418104, 2.621784821874999949 ) ) ;
#51377 = CARTESIAN_POINT ( 'NONE',  ( 3.150000001229034119, -2.886751345948129988, 4.999999999999997335 ) ) ;
#51378 = ORIENTED_EDGE ( 'NONE', *, *, #44687, .F. ) ;
#51379 = CARTESIAN_POINT ( 'NONE',  ( 27.07499999999999929, 6.123233995736764310E-16, -4.999999999999998224 ) ) ;
#51380 = CARTESIAN_POINT ( 'NONE',  ( -1.999999999999997113, 12.87500000000000178, -26.53589838486224295 ) ) ;
#51381 = CARTESIAN_POINT ( 'NONE',  ( -7.967954043666661671E-16, 17.14062499938548356, 34.33755215474603517 ) ) ;
#51382 = CARTESIAN_POINT ( 'NONE',  ( 28.34062500061451928, 6.054752690667223547, 3.707466751127219781E-16 ) ) ;
#51383 = CARTESIAN_POINT ( 'NONE',  ( 11.27812500061451573, 4.541064518000418104, 2.621784821874999949 ) ) ;
#51384 = CARTESIAN_POINT ( 'NONE',  ( 22.38750000122903216, 4.330127018922191873, 2.499999999999999556 ) ) ;
#51385 = CARTESIAN_POINT ( 'NONE',  ( 27.70312500061451289, -4.541064518000417216, -2.621784821875001281 ) ) ;
#51386 = CARTESIAN_POINT ( 'NONE',  ( 28.68749999999999645, -2.886751345948129988, 4.999999999999997335 ) ) ;
#51387 = CARTESIAN_POINT ( 'NONE',  ( -3.999999999999997335, 17.90000000122903501, -27.69059892324149175 ) ) ;
#51388 = DIRECTION ( 'NONE',  ( -1.000000000000000000, -0.000000000000000000, -0.000000000000000000 ) ) ;
#51389 = CARTESIAN_POINT ( 'NONE',  ( 13.79062500061451502, -3.027376345333610441, -5.243569643749999898 ) ) ;
#51390 = ORIENTED_EDGE ( 'NONE', *, *, #24843, .T. ) ;
#51391 = VECTOR ( 'NONE', #68866, 1000.000000000000000 ) ;
#51392 = CARTESIAN_POINT ( 'NONE',  ( 8.128125000614515372, 4.541064518000418104, 2.621784821874999949 ) ) ;
#51393 = AXIS2_PLACEMENT_3D ( 'NONE', #22257, #39627, #17428 ) ;
#51394 = CARTESIAN_POINT ( 'NONE',  ( 5.615625000614517859, -6.054752690667223547, -1.112240025338166033E-15 ) ) ;
#51395 = CARTESIAN_POINT ( 'NONE',  ( 16.88437500061451502, -4.119189519843968306, 2.378215178124996054 ) ) ;
#51396 = DIRECTION ( 'NONE',  ( -1.000000000000000000, -0.000000000000000000, -0.000000000000000000 ) ) ;
#51397 = CARTESIAN_POINT ( 'NONE',  ( 16.05000000000000071, 0.000000000000000000, 4.999999999999998224 ) ) ;
#51398 =( BOUNDED_CURVE ( )  B_SPLINE_CURVE ( 2, ( #51189, #68545, #28295, #68187, #67468, #6120, #22380 ),
 .UNSPECIFIED., .F., .F. ) 
 B_SPLINE_CURVE_WITH_KNOTS ( ( 3, 2, 2, 3 ),
 ( 0.7900000000000001465, 0.7933333333333334458, 0.7966666666666666341, 0.8000000000000000444 ),
 .UNSPECIFIED. ) 
 CURVE ( )  GEOMETRIC_REPRESENTATION_ITEM ( )  RATIONAL_B_SPLINE_CURVE ( ( 0.9999999999999955591, 0.8660254037844431485, 1.000000000000000000, 0.8660254037844387076, 1.000000000000000000, 0.8660254037844387076, 1.000000000000000000 ) ) 
 REPRESENTATION_ITEM ( '' )  );
#51399 = CARTESIAN_POINT ( 'NONE',  ( 15.64687500061451608, -3.027376345333610441, -5.243569643749999898 ) ) ;
#51400 = CARTESIAN_POINT ( 'NONE',  ( 10.68750000122903288, 4.330127018922191873, 2.499999999999999556 ) ) ;
#51401 = CARTESIAN_POINT ( 'NONE',  ( 19.73437500061451644, 6.421520780324663323E-16, -5.243569643749999010 ) ) ;
#51402 = CARTESIAN_POINT ( 'NONE',  ( 16.91250000000000142, 2.886751345948126879, 4.999999999999999112 ) ) ;
#51403 = CARTESIAN_POINT ( 'NONE',  ( 21.68437500061451573, 4.541064518000418104, 2.621784821874999949 ) ) ;
#51404 = CARTESIAN_POINT ( 'NONE',  ( 9.001249775931846008E-16, 13.61562500061451786, -25.09994784771203058 ) ) ;
#51405 = DIRECTION ( 'NONE',  ( 0.000000000000000000, 0.000000000000000000, -1.000000000000000000 ) ) ;
#51406 = CARTESIAN_POINT ( 'NONE',  ( 25.24687500061451217, 0.000000000000000000, 4.756430356249998326 ) ) ;
#51407 = CARTESIAN_POINT ( 'NONE',  ( 1.626862140677534273E-15, 13.02500000122903501, -26.00000000000000355 ) ) ;
#51408 = CARTESIAN_POINT ( 'NONE',  ( 26.27812500061451573, -4.541064518000419881, 2.621784821874995952 ) ) ;
#51409 =( LENGTH_UNIT ( ) NAMED_UNIT ( * ) SI_UNIT ( .MILLI., .METRE. ) );
#51410 = CARTESIAN_POINT ( 'NONE',  ( 28.20937500061451786, -4.541064518000417216, -2.621784821875001281 ) ) ;
#51411 = EDGE_CURVE ( 'NONE', #52162, #56056, #56237, .T. ) ;
#51412 = CARTESIAN_POINT ( 'NONE',  ( 23.69999999999999929, 0.000000000000000000, 4.999999999999998224 ) ) ;
#51413 = CARTESIAN_POINT ( 'NONE',  ( 6.928125000614516082, -4.541064518000419881, 2.621784821874995952 ) ) ;
#51414 = CARTESIAN_POINT ( 'NONE',  ( 23.97187500061451715, -4.119189519843968306, 2.378215178124996054 ) ) ;
#51415 = CARTESIAN_POINT ( 'NONE',  ( 19.84687500061451360, 6.054752690667223547, 3.707466751127219781E-16 ) ) ;
#51416 = CARTESIAN_POINT ( 'NONE',  ( 10.73437500061451644, 5.492252693125287522, 3.363034840372157021E-16 ) ) ;
#51417 = VECTOR ( 'NONE', #27068, 1000.000000000000000 ) ;
#51418 = CARTESIAN_POINT ( 'NONE',  ( 4.790625000614518569, -3.027376345333610441, -5.243569643749999898 ) ) ;
#51419 = CARTESIAN_POINT ( 'NONE',  ( 10.20937500061451786, -4.541064518000417216, -2.621784821875001281 ) ) ;
#51420 = VERTEX_POINT ( 'NONE', #45849 ) ;
#51421 = CARTESIAN_POINT ( 'NONE',  ( 21.30937500061451573, 0.000000000000000000, 5.243569643749999010 ) ) ;
#51422 = CARTESIAN_POINT ( 'NONE',  ( 3.193447721043152665, 3.847322660365763536, 3.562742055761627835 ) ) ;
#51423 = CARTESIAN_POINT ( 'NONE',  ( 29.36250000000000071, 2.886751345948129099, -4.999999999999998224 ) ) ;
#51424 = CARTESIAN_POINT ( 'NONE',  ( 29.18437500061451573, 6.421520780324663323E-16, -5.243569643749999010 ) ) ;
#51425 = DIRECTION ( 'NONE',  ( -0.000000000000000000, -1.000000000000000000, -0.000000000000000000 ) ) ;
#51426 = CARTESIAN_POINT ( 'NONE',  ( 27.86249999999999716, -5.773502691896255534, -1.060575238724906372E-15 ) ) ;
#51427 = VERTEX_POINT ( 'NONE', #1516 ) ;
#51428 = CARTESIAN_POINT ( 'NONE',  ( 9.337500000000000355, -2.886751345948129988, 4.999999999999997335 ) ) ;
#51429 = CARTESIAN_POINT ( 'NONE',  ( 11.78437500061451360, -2.746126346562646425, 4.756430356249996549 ) ) ;
#51430 = CARTESIAN_POINT ( 'NONE',  ( 24.17812500061451786, 6.421520780324663323E-16, -5.243569643749999010 ) ) ;
#51431 = CARTESIAN_POINT ( 'NONE',  ( 14.06250000000000000, 2.886751345948129099, -4.999999999999998224 ) ) ;
#51432 = CARTESIAN_POINT ( 'NONE',  ( 10.95000000122903394, -2.886751345948125991, -5.000000000000000000 ) ) ;
#51433 = CARTESIAN_POINT ( 'NONE',  ( 8.503125000614515372, 4.541064518000418104, -2.621784821874998173 ) ) ;
#51434 = CARTESIAN_POINT ( 'NONE',  ( 23.88749999999999929, -2.886751345948125991, -5.000000000000000000 ) ) ;
#51435 = CARTESIAN_POINT ( 'NONE',  ( 20.95312500061451999, -4.541064518000417216, -2.621784821875001281 ) ) ;
#51436 = CARTESIAN_POINT ( 'NONE',  ( 18.75000000122903288, 5.773502691896255534, 3.535250795749688401E-16 ) ) ;
#51437 = CARTESIAN_POINT ( 'NONE',  ( 28.27500000122903145, 2.886751345948126879, 4.999999999999999112 ) ) ;
#51438 = CARTESIAN_POINT ( 'NONE',  ( -1.878215178124999163, 16.39062499938548356, 26.74683588394047007 ) ) ;
#51439 = CARTESIAN_POINT ( 'NONE',  ( 7.425000000000000711, 4.330127018922191873, 2.499999999999999556 ) ) ;
#51440 = EDGE_LOOP ( 'NONE', ( #26428, #71187, #68062, #24165 ) ) ;
#51441 = CARTESIAN_POINT ( 'NONE',  ( 21.32812500061451644, -4.541064518000419881, 2.621784821874995952 ) ) ;
#51442 = CARTESIAN_POINT ( 'NONE',  ( 3.361055028349045237, -3.701798089632991839, -3.568395224226307061 ) ) ;
#51443 = CARTESIAN_POINT ( 'NONE',  ( 28.47187500061451715, 3.027376345333611329, 5.243569643749999010 ) ) ;
#51444 = CARTESIAN_POINT ( 'NONE',  ( 19.02187500061451786, 3.027376345333611329, 5.243569643749999010 ) ) ;
#51445 = CARTESIAN_POINT ( 'NONE',  ( 16.30312500061451786, 0.000000000000000000, 5.243569643749999010 ) ) ;
#51446 = CARTESIAN_POINT ( 'NONE',  ( 4.243569643749999898, 10.09062500061459566, -27.54997392385601529 ) ) ;
#51447 = CARTESIAN_POINT ( 'NONE',  ( 5.278125000614516615, 6.421520780324663323E-16, -5.243569643749999010 ) ) ;
#51448 =( BOUNDED_CURVE ( )  B_SPLINE_CURVE ( 2, ( #13497, #52673, #18675, #41237, #35677, #63749, #57840, #70396, #2081 ),
 .UNSPECIFIED., .F., .F. ) 
 B_SPLINE_CURVE_WITH_KNOTS ( ( 3, 2, 2, 2, 3 ),
 ( 0.6847826086956522174, 0.6884057971014492239, 0.6956521739130434590, 0.7028985507246376940, 0.7065217391304348116 ),
 .UNSPECIFIED. ) 
 CURVE ( )  GEOMETRIC_REPRESENTATION_ITEM ( )  RATIONAL_B_SPLINE_CURVE ( ( 0.9330127018922192983, 0.9330127018922202975, 1.000000000000000000, 0.8660254037844387076, 1.000000000000000000, 0.8660254037844387076, 1.000000000000000000, 0.9330127018922194093, 0.9330127018922194093 ) ) 
 REPRESENTATION_ITEM ( '' )  );
#51449 = CARTESIAN_POINT ( 'NONE',  ( 27.60000000122903430, -2.886751345948125991, -5.000000000000000000 ) ) ;
#51450 = CARTESIAN_POINT ( 'NONE',  ( 21.45937500061451786, -4.119189519843965641, -2.378215178125001383 ) ) ;
#51451 = CARTESIAN_POINT ( 'NONE',  ( 18.74062500061451431, -3.027376345333610441, -5.243569643749999898 ) ) ;
#51452 = CARTESIAN_POINT ( 'NONE',  ( 27.18750000122903288, 6.123233995736764310E-16, -4.999999999999998224 ) ) ;
#51453 = CARTESIAN_POINT ( 'NONE',  ( 3.337500001229034563, 6.123233995736764310E-16, -4.999999999999998224 ) ) ;
#51454 = CARTESIAN_POINT ( 'NONE',  ( 12.94687500061451857, -3.027376345333610441, -5.243569643749999898 ) ) ;
#51455 = CARTESIAN_POINT ( 'NONE',  ( 12.98437500061451821, 6.421520780324663323E-16, -5.243569643749999010 ) ) ;
#51456 = CARTESIAN_POINT ( 'NONE',  ( 20.70937500061451786, 4.541064518000418104, -2.621784821874998173 ) ) ;
#51457 = VERTEX_POINT ( 'NONE', #62826 ) ;
#51458 = CARTESIAN_POINT ( 'NONE',  ( 24.22500000122903430, 2.886751345948093572, 5.000000000000056843 ) ) ;
#51459 = CARTESIAN_POINT ( 'NONE',  ( 24.29062500061451502, 6.054752690667223547, 3.707466751127219781E-16 ) ) ;
#51460 = CARTESIAN_POINT ( 'NONE',  ( 18.23437500061451999, -4.541064518000419881, 2.621784821874995952 ) ) ;
#51461 = CARTESIAN_POINT ( 'NONE',  ( 23.65312500061451573, -4.541064518000417216, -2.621784821875001281 ) ) ;
#51462 = CARTESIAN_POINT ( 'NONE',  ( 27.22499999999999787, 4.330127018922191873, 2.499999999999999556 ) ) ;
#51463 = CARTESIAN_POINT ( 'NONE',  ( 2.000000000000001332, 16.10000000000000142, 33.46410161513774995 ) ) ;
#51464 = CARTESIAN_POINT ( 'NONE',  ( 29.01562500061451644, -6.054752690667223547, -1.112240025338166033E-15 ) ) ;
#51465 = CARTESIAN_POINT ( 'NONE',  ( 8.587500001229035007, -4.330127018922194537, 2.499999999999995559 ) ) ;
#51466 = CARTESIAN_POINT ( 'NONE',  ( 7.537500001229033408, 4.330127018922191873, 2.499999999999999556 ) ) ;
#51467 = CARTESIAN_POINT ( 'NONE',  ( -3.999999999999999112, 19.09999999999999787, -30.00000000000000000 ) ) ;
#51468 = CARTESIAN_POINT ( 'NONE',  ( 26.55000000122902648, -2.886751345948129988, 4.999999999999997335 ) ) ;
#51469 = CARTESIAN_POINT ( 'NONE',  ( 1.999999999999997335, 19.11874999877096570, 33.46410161513775705 ) ) ;
#51470 = CARTESIAN_POINT ( 'NONE',  ( 17.08125000122903003, -4.330127018922194537, 2.499999999999995559 ) ) ;
#51471 = CARTESIAN_POINT ( 'NONE',  ( 8.821875000614518569, -6.054752690667223547, -1.112240025338166033E-15 ) ) ;
#51472 = CARTESIAN_POINT ( 'NONE',  ( 17.62500000000000000, 6.123233995736764310E-16, -4.999999999999998224 ) ) ;
#51473 = EDGE_CURVE ( 'NONE', #16300, #39486, #6321, .T. ) ;
#51474 = CARTESIAN_POINT ( 'NONE',  ( 18.06562500061451715, 3.027376345333611329, 5.243569643749999010 ) ) ;
#51475 = CARTESIAN_POINT ( 'NONE',  ( 11.10937500061451644, -4.541064518000417216, -2.621784821875001281 ) ) ;
#51476 = CARTESIAN_POINT ( 'NONE',  ( 29.21250000122903145, 0.000000000000000000, 4.999999999999998224 ) ) ;
#51477 = ADVANCED_FACE ( 'NONE', ( #30303 ), #12219, .T. ) ;
#51478 = CARTESIAN_POINT ( 'NONE',  ( 19.84687500061451360, 6.054752690667223547, 3.707466751127219781E-16 ) ) ;
#51479 = CARTESIAN_POINT ( 'NONE',  ( 6.534375000614517148, -4.541064518000419881, 2.621784821874995952 ) ) ;
#51480 = DIRECTION ( 'NONE',  ( 1.000000000000000000, 0.000000000000000000, 0.000000000000000000 ) ) ;
#51481 = CARTESIAN_POINT ( 'NONE',  ( 5.850000000000001421, -4.330127018922190985, -2.500000000000001332 ) ) ;
#51482 = CARTESIAN_POINT ( 'NONE',  ( 8.540625000614518569, 6.054752690667223547, 3.707466751127219781E-16 ) ) ;
#51483 = CARTESIAN_POINT ( 'NONE',  ( 21.06562500061451715, 3.027376345333613106, -5.243569643749998122 ) ) ;
#51484 =( BOUNDED_CURVE ( )  B_SPLINE_CURVE ( 2, ( #69518, #19974, #41792, #13341, #53611, #35878, #8543 ),
 .UNSPECIFIED., .F., .F. ) 
 B_SPLINE_CURVE_WITH_KNOTS ( ( 3, 2, 2, 3 ),
 ( 0.2333333333333333648, 0.2361111111111111327, 0.2388888888888889284, 0.2416666666666666963 ),
 .UNSPECIFIED. ) 
 CURVE ( )  GEOMETRIC_REPRESENTATION_ITEM ( )  RATIONAL_B_SPLINE_CURVE ( ( 0.9999999999999986677, 0.8660254037844400399, 1.000000000000000000, 0.8660254037844387076, 1.000000000000000000, 0.8660254037844373753, 1.000000000000001332 ) ) 
 REPRESENTATION_ITEM ( '' )  );
#51485 = ORIENTED_EDGE ( 'NONE', *, *, #25902, .T. ) ;
#51486 = CARTESIAN_POINT ( 'NONE',  ( 4.912500001229034297, 0.000000000000000000, 4.999999999999998224 ) ) ;
#51487 = CARTESIAN_POINT ( 'NONE',  ( 14.39062500061451821, 6.054752690667223547, 3.707466751127219781E-16 ) ) ;
#51488 = CARTESIAN_POINT ( 'NONE',  ( 13.22812500061451502, -4.541064518000419881, 2.621784821874995952 ) ) ;
#51489 = CARTESIAN_POINT ( 'NONE',  ( 24.64687500061451431, -2.746126346562642428, -4.756430356249999214 ) ) ;
#51490 = CARTESIAN_POINT ( 'NONE',  ( 12.26249999999999929, 2.886751345948129099, -4.999999999999998224 ) ) ;
#51491 = CARTESIAN_POINT ( 'NONE',  ( 8.062500001229034652, 0.000000000000000000, 4.999999999999998224 ) ) ;
#51492 = CARTESIAN_POINT ( 'NONE',  ( 4.865625000614517859, 3.027376345333613106, -5.243569643749998122 ) ) ;
#51493 = CARTESIAN_POINT ( 'NONE',  ( 17.47500000122903430, 2.886751345948126879, 4.999999999999999112 ) ) ;
#51494 = CARTESIAN_POINT ( 'NONE',  ( 24.00000000000000000, 4.330127018922192761, -2.499999999999997780 ) ) ;
#51495 =( BOUNDED_SURFACE ( )  B_SPLINE_SURFACE ( 1, 2, ( 
 ( #6224, #21483, #6594, #28752, #29124, #62371, #23569, #60633, #22837, #45755, #45389, #67925, #18015, #66192, #11410, #44035, #62733, #12125, #15570, #34652, #40211, #5861, #32579, #28393, #68291, #17651, #10045, #50931, #5370, #14343, #5007, #42430, #50073, #38625, #20606, #31341, #70500, #20239, #25802, #36877, #25429, #65312, #44173, #16800, #67439, #53882, #42791, #3641, #14702, #66703, #26165, #59033, #16075, #47972, #61507, #37246, #8435, #59767, #61149, #19877, #3274, #64951, #10544, #59395, #9174, #72605, #33072, #55611, #48340, #8805, #31709, #70865, #54244, #48704, #71227, #27541, #30971, #53506, #21986, #44545, #67076, #16435, #38992, #10904, #2899, #33432, #55976, #27909, #50443, #72968, #22350, #44902, #28267, #34154, #50798, #45979, #201, #560, #51882, #6091, #6815, #11994, #28622, #45625, #45258, #56691, #6452, #17522, #34881, #17165, #68514, #62598, #29349, #69241, #24152, #56343, #28987, #40084, #34517, #52242, #57047, #22706, #67791, #39724, #63318, #925, #17876, #46706, #18231, #62243, #5732, #11639, #39357, #23433, #51159, #57410, #1280, #23070, #51525, #68159, #61871, #29704, #40435, #68875, #12709, #62952, #12346, #23790, #46341, #7176, #40805, #35246, #33799, #57767, #1646, #11279, #9865, #66383, #38299, #44226, #55663, #10959, #5783, #61557, #54936, #33480, #72659, #11331, #67129, #32767, #4342, #22758, #56030, #37937, #26867, #66015, #66759, #16130, #39043, #33849, #16851, #49398, #33126, #50492, #67488, #5059, #5422, #43858, #50128, #10598, #27960, #73018, #71929, #22039, #27596, #15395, #44598, #21304, #39407, #49765, #60456, #38682, #16486, #15759, #60827, #10233, #22402, #55304, #27228, #44950, #4698, #61925, #61203, #72291, #21669, #56393, #28314, #50850, #250, #32396, #23121, #51935, #68568, #12760, #2057, #30117, #62294, #12402, #46032, #23485, #58177, #40490, #56740, #51213, #45675, #69292, #6869, #23844, #52651, #24205, #68211, #11690, #17572, #45310, #29401, #34568, #63376, #57817, #40134, #17927, #29041, #67845, #35657, #63005, #1694, #18655, #57097, #34206, #6506, #34937, #13117, #6142, #7227, #39778, #57463, #28673, #51576, #1332, #41217, #17217, #62648, #12045, #46392, #613, #63725, #68927, #7582, #18284, #975, #40859, #35296, #29756, #52293, #46757, #54482, #60006, #64457, #13470, #9050, #31581, #37485, #14578, #65188, #19008, #69646, #36390, #70731, #14212, #19749, #31946, #43029, #53014, #42663, #7948, #37111, #3146, #59269, #70004, #36019, #58902, #13848, #2408, #64088, #30843, #8677, #24569, #47114, #19374, #8314, #42298, #53377, #53749, #41570, #70371, #54120, #58536, #30485, #59638, #3516, #36749, #47843, #65558, #24929, #26037, #47472, #64824, #31209, #20109, #25672, #48209, #41931, #48576, #71103, #2773, #20476, #25296, #14947, #9416, #39322, #10869, #55579, #60737, #21951, #43403, #4972, #65928, #49310, #50408, #20851, #4253, #71844, #55218, #66664, #44508, #16764, #72565, #15308, #67042, #10512, #22314, #27506, #43768, #37846, #33763, #16402, #48946, #60367, #3883, #4613, #27143, #50039, #44867, #27875, #9776, #44137, #61474, #5335, #16041, #38956, #54844, #61115, #21583, #33402, #55939, #32310, #26778, #38589, #21215, #72932, #67403, #33039, #32679, #61835, #11240, #66292, #15672, #38209, #71475, #10147, #26403, #49677, #72206, #167, #46301, #46666, #34847, #50762, #28588, #51125, #62206, #11602, #62561, #29669, #51844, #1247, #6417, #23033, #41131, #23752, #12674, #1606, #522, #5696, #18565, #45944, #40049, #28949, #29313, #22671, #45222, #68475, #34482, #51488, #57012, #57733, #34119, #28232, #17837, #56659, #11957, #40398, #888, #13030, #62917, #67755, #7139, #23395, #56307, #12312, #57374, #17127, #45588, #39688, #6781, #6053, #17487, #68840, #68122, #18197, #40768, #63282, #35211, #52205, #24117, #69207, #63641, #31120, #13383, #42212, #58817, #3052, #65467, #20392, #52567, #2686, #36303, #13761, #48490, #30756, #47027, #41483, #35928, #59550, #70285, #14124, #42941, #14491, #58450, #1974, #7862, #35569, #19657, #24839, #53660, #48122, #30398, #8228, #19287, #58088, #25950, #53287, #65102, #8961, #47387, #24483, #69917, #25202, #3430, #69562, #70645, #30024, #47750, #18923, #41841, #64736, #31495, #7496, #52927, #2324, #36662, #64003, #54035, #59181, #71014, #8590, #64370, #25583, #20020, #42574, #37025, #60644, #44783, #50322, #54757, #3794, #72474, #21860, #27785, #4883, #55489, #9327, #59921, #26691, #61024, #4527, #10059, #22227, #33315, #43317, #32952, #71386, #27418, #66571, #49586, #60277, #26316, #49224, #4161, #65837, #54395, #21127, #72110, #14858, #37397, #9690, #71758, #32591, #20759, #32223, #55129, #66203, #10421, #15220, #21494, #38123, #49949, #31860, #72846, #48855, #27056, #15581, #44047, #37759, #15950, #43680, #38498, #44421, #38869, #66948, #16316, #61386, #10782, #55853, #5243, #39592, #24026, #28854, #56567, #12224, #6692, #45133, #17400, #51033, #67316, #57645, #45498, #23667, #18110, #5963, #33676, #28497, #56921, #35122, #28147, #29222, #61744, #11868, #5611, #429, #39957, #40673, #16674, #62115, #67668, #23304, #22584, #63193, #45853, #12587, #6325, #29581, #11146, #62471, #62830, #34389, #51394, #39232, #52119, #34030, #56218, #51758, #1158, #7052, #57287, #34752, #50675, #79, #22938, #40308, #795, #68388, #1521, #17035, #11508, #46213, #68028, #68752, #17749, #9145, #18836, #58002, #7775, #13300, #24392, #12944, #53852, #31681, #4350, #54945, #41399, #31310, #65283, #3244, #54215, #14671, #46575, #3612, #35480, #49045, #25772, #69120, #48310, #26133, #7410, #63914, #29938, #48674, #52478, #70834, #60102, #35837, #15042, #20209, #58361, #42763, #18478, #37215, #1888, #71198, #41043, #59736, #32044, #46942, #69478, #65652, #9511, #20573, #43129, #66025, #63557, #71573 ),
 ( #37579, #54576, #20947, #3980, #26504, #43500, #15403, #37945, #60464, #9873, #32407, #15768, #22410, #33489, #45316, #27969, #66766, #38310, #56746, #67495, #71938, #60837, #26877, #5068, #27603, #73026, #67851, #50858, #10242, #67137, #11339, #28321, #16495, #44957, #4706, #10966, #44607, #16858, #61934, #32775, #55312, #39050, #27237, #50499, #17224, #61564, #55671, #33855, #56037, #49774, #72298, #21678, #21314, #33134, #39413, #72667, #256, #43867, #56399, #39784, #5429, #66391, #44235, #16139, #38691, #61210, #50136, #22765, #5789, #62300, #22046, #10605, #11696, #34212, #49406, #24575, #23492, #28679, #41577, #68935, #63013, #51942, #52299, #621, #45684, #18293, #57471, #1339, #6876, #7588, #34576, #57825, #64094, #58184, #57104, #23128, #51584, #36027, #40865, #68575, #24213, #18661, #6515, #29409, #12411, #6150, #69652, #23851, #35663, #30125, #17935, #68217, #40497, #63382, #47120, #29048, #46399, #7234, #34944, #17579, #12767, #35302, #52657, #51219, #984, #46039, #29762, #1700, #2066, #46764, #19016, #69299, #13477, #40140, #41223, #63732, #13124, #62656, #12052, #20858, #25303, #47479, #43036, #65564, #71483, #48584, #26044, #53020, #30492, #70378, #31589, #48216, #53757, #65935, #3890, #13855, #3523, #41939, #71110, #37117, #20116, #30849, #70012, #19756, #47851, #36397, #24936, #64832, #42671, #15315, #58544, #53384, #42305, #3152, #14220, #65194, #25681, #7955, #14584, #19380, #60012, #36756, #2414, #59275, #59646, #64463, #2779, #58910, #9057, #8320, #8683, #20482, #31215, #14953, #70738, #54127, #37492, #9423, #31952, #54490, #26410, #48952, #43410, #44514, #61123, #5341, #67760, #22677, #54851, #4980, #38596, #16047, #50769, #33046, #49319, #43774, #15678, #61841, #72571, #172, #44873, #16408, #21590, #4260, #71850, #21958, #26784, #10154, #11245, #21222, #38216, #32686, #10518, #27512, #55945, #45227, #33407, #66301, #27880, #67049, #56312, #38963, #4620, #60743, #37854, #50414, #9783, #55225, #60375, #55585, #50046, #10874, #5702, #33770, #27149, #61480, #22320, #39327, #72938, #67408, #49683, #16770, #28237, #32316, #72212, #44144, #66671, #29320, #527, #18204, #58095, #51849, #45950, #52211, #1253, #51130, #23038, #6060, #62212, #23401, #40773, #62923, #41137, #34125, #7144, #7501, #68845, #11607, #62567, #11963, #45596, #68127, #68480, #63646, #12680, #35217, #40405, #57017, #1980, #57738, #46673, #35574, #34488, #39693, #52572, #6786, #894, #12317, #63287, #56664, #28594, #23757, #17843, #34852, #57379, #18571, #17493, #40054, #46308, #6422, #29675, #17133, #1613, #24123, #28954, #51493, #69213, #13037, #30031, #24489, #47033, #41489, #71021, #7868, #19664, #3058, #65108, #31126, #14132, #13767, #14498, #48496, #64009, #42947, #30404, #69568, #64742, #52932, #53667, #58456, #41848, #65475, #13389, #69924, #64375, #47756, #59187, #37032, #9334, #59556, #2329, #8969, #25589, #14864, #70652, #36308, #24847, #26324, #31501, #35933, #47393, #18929, #70292, #42218, #42582, #37404, #20398, #19293, #36668, #54041, #59927, #8597, #3437, #58823, #48128, #20026, #25956, #31866, #8233, #30762, #54401, #53294, #3801, #2694, #25209, #4534, #10787, #32959, #9696, #32229, #37765, #20766, #55136, #49956, #21500, #72851, #65844, #38875, #39237, #27425, #43323, #21134, #43686, #54764, #4168, #27062, #22233, #44427, #66956, #72118, #15587, #33680, #16322, #5248, #67321, #66209, #71392, #11153, #38505, #32597, #44053, #21866, #15226, #60284, #61030, #49593, #66579, #15956, #50327, #26697, #49231, #10428, #71764, #4890, #48861, #55495, #33321, #38129, #60651, #61394, #55859, #72480, #27790, #16681, #10066, #44789, #61751, #56224, #5617, #23672, #62837, #45859, #45505, #46219, #7058, #22589, #1526, #39600, #28152, #23310, #63562, #35127, #6698, #11873, #67673, #62121, #11513, #40313, #34035, #29231, #69125, #12229, #56926, #63198, #34758, #56573, #5970, #17042, #84, #34398, #51764, #803, #52124, #45140, #18116, #18483, #1163, #28501, #435, #22944, #51039, #68035, #6330, #24033, #68757, #40680, #51400, #17405, #12950, #12594, #57652, #46582, #39962, #50681, #35487, #17754, #28861, #68393, #29586, #62476, #57293, #41049, #58007, #2600, #8145, #8876, #35843, #29943, #70197, #58368, #36580, #7415, #53204, #65020, #46947, #13305, #25498, #19944, #19573, #30672, #25870, #52483, #31411, #18843, #25121, #14040, #2970, #42129, #47663, #24760, #48043, #59466, #1894, #53951, #41404, #24398, #64655, #42860, #14409, #59100, #64286, #69484, #63920, #8507, #7779, #52846, #3348, #30316, #2244, #47303, #58734, #31036, #70568, #20307, #42497, #69838, #36946, #53572, #48410, #70936, #19203, #41757, #37315, #65382, #13674, #36218, #14773, #38039, #60563, #32869, #5160, #10698, #71297, #26973, #44334, #61303, #49502, #55406, #37675, #43964, #4445, #27334, #21770, #72031, #9970, #55042, #32507, #33230, #15137, #9244, #21407, #60197, #15864, #59839, #66485, #66862, #26236, #65753, #4801, #72390, #38412, #60933, #27695, #31779, #55768, #20676, #10337, #49866, #16233, #38786, #50235, #4076, #72757, #22143, #54318, #44696, #43233, #3709, #67230, #16589, #48773, #9609, #43597, #32140, #54673, #26604, #49142, #71671, #21045, #66118, #15497, #11428, #17318, #28771, #57199, #52037, #34671, #28062, #6615, #45775, #57567, #40230, #5882, #50592, #69034, #29142, #11059, #57993, #39142, #39878, #62390, #12145, #6971, #63112, #22502, #6244, #62752, #34305, #51311, #56837, #46496, #29502, #67587, #51677, #45051, #1081, #17670, #715, #33947, #16953, #348, #28413, #39506, #5524, #45409, #23222, #61659, #33585, #56488, #22855, #68310, #67945, #23588, #46134, #56131, #68672, #62032, #40591, #11788, #50951, #18035, #12511, #35040, #1441, #23946, #25037, #52397, #52759, #30948, #58283, #59013 ) ),
 .UNSPECIFIED., .F., .F., .F. ) 
 B_SPLINE_SURFACE_WITH_KNOTS ( ( 2, 2 ),
 ( 3, 2, 2, 2, 2, 2, 2, 2, 2, 2, 2, 2, 2, 2, 2, 2, 2, 2, 2, 2, 2, 2, 2, 2, 2, 2, 2, 2, 2, 2, 2, 2, 2, 2, 2, 2, 2, 2, 2, 2, 2, 2, 2, 2, 2, 2, 2, 2, 2, 2, 2, 2, 2, 2, 2, 2, 2, 2, 2, 2, 2, 2, 2, 2, 2, 2, 2, 2, 2, 2, 2, 2, 2, 2, 2, 2, 2, 2, 2, 2, 2, 2, 2, 2, 2, 2, 2, 2, 2, 2, 2, 2, 2, 2, 2, 2, 2, 2, 2, 2, 2, 2, 2, 2, 2, 2, 2, 2, 2, 2, 2, 2, 2, 2, 2, 2, 2, 2, 2, 2, 2, 2, 2, 2, 2, 2, 2, 2, 2, 2, 2, 2, 2, 2, 2, 2, 2, 2, 2, 2, 2, 2, 2, 2, 2, 2, 2, 2, 2, 2, 2, 2, 2, 2, 2, 2, 2, 2, 2, 2, 2, 2, 2, 2, 2, 2, 2, 2, 2, 2, 2, 2, 2, 2, 2, 2, 2, 2, 2, 2, 2, 2, 2, 2, 2, 2, 2, 2, 2, 2, 2, 2, 2, 2, 2, 2, 2, 2, 2, 2, 2, 2, 2, 2, 2, 2, 2, 2, 2, 2, 2, 2, 2, 2, 2, 2, 2, 2, 2, 2, 2, 2, 2, 2, 2, 2, 2, 2, 2, 2, 2, 2, 2, 2, 2, 2, 2, 2, 2, 2, 2, 2, 2, 2, 2, 2, 2, 2, 2, 2, 2, 2, 2, 2, 2, 2, 2, 2, 2, 2, 2, 2, 2, 2, 2, 2, 2, 2, 2, 2, 2, 2, 2, 2, 2, 2, 2, 2, 2, 2, 2, 2, 2, 2, 2, 2, 2, 2, 2, 2, 2, 2, 2, 2, 2, 2, 2, 2, 2, 2, 2, 2, 2, 2, 2, 2, 2, 2, 2, 2, 2, 2, 2, 2, 2, 2, 2, 2, 2, 2, 2, 2, 2, 2, 2, 2, 2, 2, 2, 2, 2, 2, 2, 2, 2, 2, 2, 2, 2, 2, 2, 2, 2, 2, 2, 2, 2, 2, 2, 2, 2, 2, 2, 2, 2, 2, 2, 2, 2, 2, 3 ),
 ( 0.000000000000000000, 1.000000000000000000 ),
 ( 0.000000000000000000, 0.002777777777777777884, 0.005555555555555555768, 0.008333333333333333218, 0.01111111111111111154, 0.01388888888888888812, 0.01666666666666666644, 0.01944444444444444475, 0.02222222222222222307, 0.02500000000000000139, 0.02777777777777777624, 0.03055555555555555455, 0.03333333333333333287, 0.03611111111111110772, 0.03888888888888888951, 0.04166666666666666435, 0.04444444444444444614, 0.04722222222222222099, 0.05000000000000000278, 0.05277777777777777762, 0.05555555555555555247, 0.05833333333333333426, 0.06111111111111110911, 0.06388888888888888395, 0.06666666666666666574, 0.06944444444444444753, 0.07222222222222221544, 0.07499999999999999722, 0.07777777777777777901, 0.08055555555555556080, 0.08333333333333332871, 0.08611111111111111049, 0.08888888888888889228, 0.09166666666666666019, 0.09444444444444444198, 0.09722222222222222376, 0.1000000000000000056, 0.1027777777777777735, 0.1055555555555555552, 0.1083333333333333370, 0.1111111111111111049, 0.1138888888888888867, 0.1166666666666666685, 0.1194444444444444503, 0.1222222222222222182, 0.1250000000000000000, 0.1277777777777777679, 0.1305555555555555636, 0.1333333333333333315, 0.1361111111111110994, 0.1388888888888888951, 0.1416666666666666630, 0.1444444444444444309, 0.1472222222222222265, 0.1499999999999999944, 0.1527777777777777901, 0.1555555555555555580, 0.1583333333333333259, 0.1611111111111111216, 0.1638888888888888895, 0.1666666666666666574, 0.1694444444444444531, 0.1722222222222222210, 0.1749999999999999889, 0.1777777777777777846, 0.1805555555555555525, 0.1833333333333333204, 0.1861111111111111160, 0.1888888888888888840, 0.1916666666666666796, 0.1944444444444444475, 0.1972222222222222154, 0.2000000000000000111, 0.2027777777777777790, 0.2055555555555555469, 0.2083333333333333426, 0.2111111111111111105, 0.2138888888888888784, 0.2166666666666666741, 0.2194444444444444420, 0.2222222222222222099, 0.2250000000000000056, 0.2277777777777777735, 0.2305555555555555691, 0.2333333333333333370, 0.2361111111111111049, 0.2388888888888889006, 0.2416666666666666685, 0.2444444444444444364, 0.2472222222222222321, 0.2500000000000000000, 0.2527777777777777679, 0.2555555555555555358, 0.2583333333333333592, 0.2611111111111111271, 0.2638888888888888951, 0.2666666666666666630, 0.2694444444444444309, 0.2722222222222221988, 0.2750000000000000222, 0.2777777777777777901, 0.2805555555555555580, 0.2833333333333333259, 0.2861111111111110938, 0.2888888888888888618, 0.2916666666666666852, 0.2944444444444444531, 0.2972222222222222210, 0.2999999999999999889, 0.3027777777777777568, 0.3055555555555555802, 0.3083333333333333481, 0.3111111111111111160, 0.3138888888888888840, 0.3166666666666666519, 0.3194444444444444198, 0.3222222222222222432, 0.3250000000000000111, 0.3277777777777777790, 0.3305555555555555469, 0.3333333333333333148, 0.3361111111111111382, 0.3388888888888889062, 0.3416666666666666741, 0.3444444444444444420, 0.3472222222222222099, 0.3499999999999999778, 0.3527777777777778012, 0.3555555555555555691, 0.3583333333333333370, 0.3611111111111111049, 0.3638888888888888729, 0.3666666666666666408, 0.3694444444444444642, 0.3722222222222222321, 0.3750000000000000000, 0.3777777777777777679, 0.3805555555555555358, 0.3833333333333333592, 0.3861111111111111271, 0.3888888888888888951, 0.3916666666666666630, 0.3944444444444444309, 0.3972222222222221988, 0.4000000000000000222, 0.4027777777777777901, 0.4055555555555555580, 0.4083333333333333259, 0.4111111111111110938, 0.4138888888888888618, 0.4166666666666666852, 0.4194444444444444531, 0.4222222222222222210, 0.4249999999999999889, 0.4277777777777777568, 0.4305555555555555802, 0.4333333333333333481, 0.4361111111111111160, 0.4388888888888888840, 0.4416666666666666519, 0.4444444444444444198, 0.4472222222222222432, 0.4500000000000000111, 0.4527777777777777790, 0.4555555555555555469, 0.4583333333333333148, 0.4611111111111111382, 0.4638888888888889062, 0.4666666666666666741, 0.4694444444444444420, 0.4722222222222222099, 0.4749999999999999778, 0.4777777777777778012, 0.4805555555555555691, 0.4833333333333333370, 0.4861111111111111049, 0.4888888888888888729, 0.4916666666666666408, 0.4944444444444444642, 0.4972222222222222321, 0.5000000000000000000, 0.5027777777777777679, 0.5055555555555555358, 0.5083333333333333037, 0.5111111111111110716, 0.5138888888888888395, 0.5166666666666667185, 0.5194444444444444864, 0.5222222222222222543, 0.5250000000000000222, 0.5277777777777777901, 0.5305555555555555580, 0.5333333333333333259, 0.5361111111111110938, 0.5388888888888888618, 0.5416666666666666297, 0.5444444444444443976, 0.5472222222222222765, 0.5500000000000000444, 0.5527777777777778123, 0.5555555555555555802, 0.5583333333333333481, 0.5611111111111111160, 0.5638888888888888840, 0.5666666666666666519, 0.5694444444444444198, 0.5722222222222221877, 0.5749999999999999556, 0.5777777777777777235, 0.5805555555555556024, 0.5833333333333333703, 0.5861111111111111382, 0.5888888888888889062, 0.5916666666666666741, 0.5944444444444444420, 0.5972222222222222099, 0.5999999999999999778, 0.6027777777777777457, 0.6055555555555555136, 0.6083333333333332815, 0.6111111111111111605, 0.6138888888888889284, 0.6166666666666666963, 0.6194444444444444642, 0.6222222222222222321, 0.6250000000000000000, 0.6277777777777777679, 0.6305555555555555358, 0.6333333333333333037, 0.6361111111111110716, 0.6388888888888888395, 0.6416666666666667185, 0.6444444444444444864, 0.6472222222222222543, 0.6500000000000000222, 0.6527777777777777901, 0.6555555555555555580, 0.6583333333333333259, 0.6611111111111110938, 0.6638888888888888618, 0.6666666666666666297, 0.6694444444444443976, 0.6722222222222222765, 0.6750000000000000444, 0.6777777777777778123, 0.6805555555555555802, 0.6833333333333333481, 0.6861111111111111160, 0.6888888888888888840, 0.6916666666666666519, 0.6944444444444444198, 0.6972222222222221877, 0.6999999999999999556, 0.7027777777777777235, 0.7055555555555556024, 0.7083333333333333703, 0.7111111111111111382, 0.7138888888888889062, 0.7166666666666666741, 0.7194444444444444420, 0.7222222222222222099, 0.7249999999999999778, 0.7277777777777777457, 0.7305555555555555136, 0.7333333333333332815, 0.7361111111111111605, 0.7388888888888889284, 0.7416666666666666963, 0.7444444444444444642, 0.7472222222222222321, 0.7500000000000000000, 0.7527777777777777679, 0.7555555555555555358, 0.7583333333333333037, 0.7611111111111110716, 0.7638888888888888395, 0.7666666666666667185, 0.7694444444444444864, 0.7722222222222222543, 0.7750000000000000222, 0.7777777777777777901, 0.7805555555555555580, 0.7833333333333333259, 0.7861111111111110938, 0.7888888888888888618, 0.7916666666666666297, 0.7944444444444443976, 0.7972222222222222765, 0.8000000000000000444, 0.8027777777777778123, 0.8055555555555555802, 0.8083333333333333481, 0.8111111111111111160, 0.8138888888888888840, 0.8166666666666666519, 0.8194444444444444198, 0.8222222222222221877, 0.8249999999999999556, 0.8277777777777777235, 0.8305555555555556024, 0.8333333333333333703, 0.8361111111111111382, 0.8388888888888889062, 0.8416666666666666741, 0.8444444444444444420, 0.8472222222222222099, 0.8499999999999999778, 0.8527777777777777457, 0.8555555555555555136, 0.8583333333333332815, 0.8611111111111111605, 0.8638888888888889284, 0.8666666666666666963, 0.8694444444444444642, 0.8722222222222222321, 0.8750000000000000000, 0.8777777777777777679, 0.8805555555555555358, 0.8833333333333333037, 0.8861111111111110716, 0.8888888888888888395, 0.8916666666666667185, 0.8944444444444444864, 0.8972222222222222543, 0.9000000000000000222, 0.9027777777777777901, 0.9055555555555555580, 0.9083333333333333259, 0.9111111111111110938, 0.9138888888888888618, 0.9166666666666666297, 0.9194444444444443976, 0.9222222222222222765, 0.9250000000000000444, 0.9277777777777778123, 0.9305555555555555802, 0.9333333333333333481, 0.9361111111111111160, 0.9388888888888888840, 0.9416666666666666519, 0.9444444444444444198, 0.9472222222222221877, 0.9499999999999999556, 0.9527777777777777235, 0.9555555555555556024, 0.9583333333333333703, 0.9611111111111111382, 0.9638888888888889062, 0.9666666666666666741, 0.9694444444444444420, 0.9722222222222222099, 0.9749999999999999778, 0.9777777777777777457, 0.9805555555555555136, 0.9833333333333332815, 0.9861111111111111605, 0.9888888888888889284, 0.9916666666666666963, 0.9944444444444444642, 0.9972222222222222321, 1.000000000000000000 ),
 .UNSPECIFIED. ) 
 GEOMETRIC_REPRESENTATION_ITEM ( )  RATIONAL_B_SPLINE_SURFACE ( (
 ( 1.000000000000000000, 0.8660254037844387076, 1.000000000000000000, 0.8660254037844387076, 1.000000000000000000, 0.8660254037844387076, 1.000000000000000000, 0.8660254037844387076, 1.000000000000000000, 0.8660254037844387076, 1.000000000000000000, 0.8660254037844387076, 1.000000000000000000, 0.8660254037844387076, 1.000000000000000000, 0.8660254037844387076, 1.000000000000000000, 0.8660254037844387076, 1.000000000000000000, 0.8660254037844387076, 1.000000000000000000, 0.8660254037844387076, 1.000000000000000000, 0.8660254037844387076, 1.000000000000000000, 0.8660254037844387076, 1.000000000000000000, 0.8660254037844387076, 1.000000000000000000, 0.8660254037844387076, 1.000000000000000000, 0.8660254037844387076, 1.000000000000000000, 0.8660254037844387076, 1.000000000000000000, 0.8660254037844387076, 1.000000000000000000, 0.8660254037844387076, 1.000000000000000000, 0.8660254037844387076, 1.000000000000000000, 0.8660254037844387076, 1.000000000000000000, 0.8660254037844387076, 1.000000000000000000, 0.8660254037844387076, 1.000000000000000000, 0.8660254037844387076, 1.000000000000000000, 0.8660254037844387076, 1.000000000000000000, 0.8660254037844387076, 1.000000000000000000, 0.8660254037844387076, 1.000000000000000000, 0.8660254037844387076, 1.000000000000000000, 0.8660254037844387076, 1.000000000000000000, 0.8660254037844387076, 1.000000000000000000, 0.8660254037844387076, 1.000000000000000000, 0.8660254037844387076, 1.000000000000000000, 0.8660254037844387076, 1.000000000000000000, 0.8660254037844387076, 1.000000000000000000, 0.8660254037844387076, 1.000000000000000000, 0.8660254037844387076, 1.000000000000000000, 0.8660254037844387076, 1.000000000000000000, 0.8660254037844387076, 1.000000000000000000, 0.8660254037844387076, 1.000000000000000000, 0.8660254037844387076, 1.000000000000000000, 0.8660254037844387076, 1.000000000000000000, 0.8660254037844387076, 1.000000000000000000, 0.8660254037844387076, 1.000000000000000000, 0.8660254037844387076, 1.000000000000000000, 0.8660254037844387076, 1.000000000000000000, 0.8660254037844387076, 1.000000000000000000, 0.8660254037844387076, 1.000000000000000000, 0.8660254037844387076, 1.000000000000000000, 0.8660254037844387076, 1.000000000000000000, 0.8660254037844387076, 1.000000000000000000, 0.8660254037844387076, 1.000000000000000000, 0.8660254037844387076, 1.000000000000000000, 0.8660254037844387076, 1.000000000000000000, 0.8660254037844387076, 1.000000000000000000, 0.8660254037844387076, 1.000000000000000000, 0.8660254037844387076, 1.000000000000000000, 0.8660254037844387076, 1.000000000000000000, 0.8660254037844387076, 1.000000000000000000, 0.8660254037844387076, 1.000000000000000000, 0.8660254037844387076, 1.000000000000000000, 0.8660254037844387076, 1.000000000000000000, 0.8660254037844387076, 1.000000000000000000, 0.8660254037844387076, 1.000000000000000000, 0.8660254037844387076, 1.000000000000000000, 0.8660254037844387076, 1.000000000000000000, 0.8660254037844387076, 1.000000000000000000, 0.8660254037844387076, 1.000000000000000000, 0.8660254037844387076, 1.000000000000000000, 0.8660254037844387076, 1.000000000000000000, 0.8660254037844387076, 1.000000000000000000, 0.8660254037844387076, 1.000000000000000000, 0.8660254037844387076, 1.000000000000000000, 0.8660254037844387076, 1.000000000000000000, 0.8660254037844387076, 1.000000000000000000, 0.8660254037844387076, 1.000000000000000000, 0.8660254037844387076, 1.000000000000000000, 0.8660254037844387076, 1.000000000000000000, 0.8660254037844387076, 1.000000000000000000, 0.8660254037844387076, 1.000000000000000000, 0.8660254037844387076, 1.000000000000000000, 0.8660254037844387076, 1.000000000000000000, 0.8660254037844387076, 1.000000000000000000, 0.8660254037844387076, 1.000000000000000000, 0.8660254037844387076, 1.000000000000000000, 0.8660254037844387076, 1.000000000000000000, 0.8660254037844387076, 1.000000000000000000, 0.8660254037844387076, 1.000000000000000000, 0.8660254037844387076, 1.000000000000000000, 0.8660254037844387076, 1.000000000000000000, 0.8660254037844387076, 1.000000000000000000, 0.8660254037844387076, 1.000000000000000000, 0.8660254037844387076, 1.000000000000000000, 0.8660254037844387076, 1.000000000000000000, 0.8660254037844387076, 1.000000000000000000, 0.8660254037844387076, 1.000000000000000000, 0.8660254037844387076, 1.000000000000000000, 0.8660254037844387076, 1.000000000000000000, 0.8660254037844387076, 1.000000000000000000, 0.8660254037844387076, 1.000000000000000000, 0.8660254037844387076, 1.000000000000000000, 0.8660254037844387076, 1.000000000000000000, 0.8660254037844387076, 1.000000000000000000, 0.8660254037844387076, 1.000000000000000000, 0.8660254037844387076, 1.000000000000000000, 0.8660254037844387076, 1.000000000000000000, 0.8660254037844387076, 1.000000000000000000, 0.8660254037844387076, 1.000000000000000000, 0.8660254037844387076, 1.000000000000000000, 0.8660254037844387076, 1.000000000000000000, 0.8660254037844387076, 1.000000000000000000, 0.8660254037844387076, 1.000000000000000000, 0.8660254037844387076, 1.000000000000000000, 0.8660254037844387076, 1.000000000000000000, 0.8660254037844387076, 1.000000000000000000, 0.8660254037844387076, 1.000000000000000000, 0.8660254037844387076, 1.000000000000000000, 0.8660254037844387076, 1.000000000000000000, 0.8660254037844387076, 1.000000000000000000, 0.8660254037844387076, 1.000000000000000000, 0.8660254037844387076, 1.000000000000000000, 0.8660254037844387076, 1.000000000000000000, 0.8660254037844387076, 1.000000000000000000, 0.8660254037844387076, 1.000000000000000000, 0.8660254037844387076, 1.000000000000000000, 0.8660254037844387076, 1.000000000000000000, 0.8660254037844387076, 1.000000000000000000, 0.8660254037844387076, 1.000000000000000000, 0.8660254037844387076, 1.000000000000000000, 0.8660254037844387076, 1.000000000000000000, 0.8660254037844387076, 1.000000000000000000, 0.8660254037844387076, 1.000000000000000000, 0.8660254037844387076, 1.000000000000000000, 0.8660254037844387076, 1.000000000000000000, 0.8660254037844387076, 1.000000000000000000, 0.8660254037844387076, 1.000000000000000000, 0.8660254037844387076, 1.000000000000000000, 0.8660254037844387076, 1.000000000000000000, 0.8660254037844387076, 1.000000000000000000, 0.8660254037844387076, 1.000000000000000000, 0.8660254037844387076, 1.000000000000000000, 0.8660254037844387076, 1.000000000000000000, 0.8660254037844387076, 1.000000000000000000, 0.8660254037844387076, 1.000000000000000000, 0.8660254037844387076, 1.000000000000000000, 0.8660254037844387076, 1.000000000000000000, 0.8660254037844387076, 1.000000000000000000, 0.8660254037844387076, 1.000000000000000000, 0.8660254037844387076, 1.000000000000000000, 0.8660254037844387076, 1.000000000000000000, 0.8660254037844387076, 1.000000000000000000, 0.8660254037844387076, 1.000000000000000000, 0.8660254037844387076, 1.000000000000000000, 0.8660254037844387076, 1.000000000000000000, 0.8660254037844387076, 1.000000000000000000, 0.8660254037844387076, 1.000000000000000000, 0.8660254037844387076, 1.000000000000000000, 0.8660254037844387076, 1.000000000000000000, 0.8660254037844387076, 1.000000000000000000, 0.8660254037844387076, 1.000000000000000000, 0.8660254037844387076, 1.000000000000000000, 0.8660254037844387076, 1.000000000000000000, 0.8660254037844387076, 1.000000000000000000, 0.8660254037844387076, 1.000000000000000000, 0.8660254037844387076, 1.000000000000000000, 0.8660254037844387076, 1.000000000000000000, 0.8660254037844387076, 1.000000000000000000, 0.8660254037844387076, 1.000000000000000000, 0.8660254037844387076, 1.000000000000000000, 0.8660254037844387076, 1.000000000000000000, 0.8660254037844387076, 1.000000000000000000, 0.8660254037844387076, 1.000000000000000000, 0.8660254037844387076, 1.000000000000000000, 0.8660254037844387076, 1.000000000000000000, 0.8660254037844387076, 1.000000000000000000, 0.8660254037844387076, 1.000000000000000000, 0.8660254037844387076, 1.000000000000000000, 0.8660254037844387076, 1.000000000000000000, 0.8660254037844387076, 1.000000000000000000, 0.8660254037844387076, 1.000000000000000000, 0.8660254037844387076, 1.000000000000000000, 0.8660254037844387076, 1.000000000000000000, 0.8660254037844387076, 1.000000000000000000, 0.8660254037844387076, 1.000000000000000000, 0.8660254037844387076, 1.000000000000000000, 0.8660254037844387076, 1.000000000000000000, 0.8660254037844387076, 1.000000000000000000, 0.8660254037844387076, 1.000000000000000000, 0.8660254037844387076, 1.000000000000000000, 0.8660254037844387076, 1.000000000000000000, 0.8660254037844387076, 1.000000000000000000, 0.8660254037844387076, 1.000000000000000000, 0.8660254037844387076, 1.000000000000000000, 0.8660254037844387076, 1.000000000000000000, 0.8660254037844387076, 1.000000000000000000, 0.8660254037844387076, 1.000000000000000000, 0.8660254037844387076, 1.000000000000000000, 0.8660254037844387076, 1.000000000000000000, 0.8660254037844387076, 1.000000000000000000, 0.8660254037844387076, 1.000000000000000000, 0.8660254037844387076, 1.000000000000000000, 0.8660254037844387076, 1.000000000000000000, 0.8660254037844387076, 1.000000000000000000, 0.8660254037844387076, 1.000000000000000000, 0.8660254037844387076, 1.000000000000000000, 0.8660254037844387076, 1.000000000000000000, 0.8660254037844387076, 1.000000000000000000, 0.8660254037844387076, 1.000000000000000000, 0.8660254037844387076, 1.000000000000000000, 0.8660254037844387076, 1.000000000000000000, 0.8660254037844387076, 1.000000000000000000, 0.8660254037844387076, 1.000000000000000000, 0.8660254037844387076, 1.000000000000000000, 0.8660254037844387076, 1.000000000000000000, 0.8660254037844387076, 1.000000000000000000, 0.8660254037844387076, 1.000000000000000000, 0.8660254037844387076, 1.000000000000000000, 0.8660254037844387076, 1.000000000000000000, 0.8660254037844387076, 1.000000000000000000, 0.8660254037844387076, 1.000000000000000000, 0.8660254037844387076, 1.000000000000000000, 0.8660254037844387076, 1.000000000000000000, 0.8660254037844387076, 1.000000000000000000, 0.8660254037844387076, 1.000000000000000000, 0.8660254037844387076, 1.000000000000000000, 0.8660254037844387076, 1.000000000000000000, 0.8660254037844387076, 1.000000000000000000, 0.8660254037844387076, 1.000000000000000000, 0.8660254037844387076, 1.000000000000000000, 0.8660254037844387076, 1.000000000000000000, 0.8660254037844387076, 1.000000000000000000, 0.8660254037844387076, 1.000000000000000000, 0.8660254037844387076, 1.000000000000000000, 0.8660254037844387076, 1.000000000000000000, 0.8660254037844387076, 1.000000000000000000, 0.8660254037844387076, 1.000000000000000000, 0.8660254037844387076, 1.000000000000000000, 0.8660254037844387076, 1.000000000000000000, 0.8660254037844387076, 1.000000000000000000, 0.8660254037844387076, 1.000000000000000000, 0.8660254037844387076, 1.000000000000000000, 0.8660254037844387076, 1.000000000000000000, 0.8660254037844387076, 1.000000000000000000, 0.8660254037844387076, 1.000000000000000000, 0.8660254037844387076, 1.000000000000000000, 0.8660254037844387076, 1.000000000000000000, 0.8660254037844387076, 1.000000000000000000, 0.8660254037844387076, 1.000000000000000000, 0.8660254037844387076, 1.000000000000000000, 0.8660254037844387076, 1.000000000000000000, 0.8660254037844387076, 1.000000000000000000, 0.8660254037844387076, 1.000000000000000000, 0.8660254037844387076, 1.000000000000000000, 0.8660254037844387076, 1.000000000000000000, 0.8660254037844387076, 1.000000000000000000, 0.8660254037844387076, 1.000000000000000000, 0.8660254037844387076, 1.000000000000000000, 0.8660254037844387076, 1.000000000000000000, 0.8660254037844387076, 1.000000000000000000, 0.8660254037844387076, 1.000000000000000000, 0.8660254037844387076, 1.000000000000000000, 0.8660254037844387076, 1.000000000000000000, 0.8660254037844387076, 1.000000000000000000, 0.8660254037844387076, 1.000000000000000000, 0.8660254037844387076, 1.000000000000000000, 0.8660254037844387076, 1.000000000000000000, 0.8660254037844387076, 1.000000000000000000, 0.8660254037844387076, 1.000000000000000000, 0.8660254037844387076, 1.000000000000000000, 0.8660254037844387076, 1.000000000000000000, 0.8660254037844387076, 1.000000000000000000, 0.8660254037844387076, 1.000000000000000000, 0.8660254037844387076, 1.000000000000000000, 0.8660254037844387076, 1.000000000000000000, 0.8660254037844387076, 1.000000000000000000, 0.8660254037844387076, 1.000000000000000000, 0.8660254037844387076, 1.000000000000000000, 0.8660254037844387076, 1.000000000000000000, 0.8660254037844387076, 1.000000000000000000, 0.8660254037844387076, 1.000000000000000000, 0.8660254037844387076, 1.000000000000000000, 0.8660254037844387076, 1.000000000000000000, 0.8660254037844387076, 1.000000000000000000, 0.8660254037844387076, 1.000000000000000000, 0.8660254037844387076, 1.000000000000000000, 0.8660254037844387076, 1.000000000000000000, 0.8660254037844387076, 1.000000000000000000, 0.8660254037844387076, 1.000000000000000000, 0.8660254037844387076, 1.000000000000000000, 0.8660254037844387076, 1.000000000000000000, 0.8660254037844387076, 1.000000000000000000, 0.8660254037844387076, 1.000000000000000000, 0.8660254037844387076, 1.000000000000000000, 0.8660254037844387076, 1.000000000000000000, 0.8660254037844387076, 1.000000000000000000, 0.8660254037844387076, 1.000000000000000000, 0.8660254037844387076, 1.000000000000000000, 0.8660254037844387076, 1.000000000000000000, 0.8660254037844387076, 1.000000000000000000, 0.8660254037844387076, 1.000000000000000000, 0.8660254037844387076, 1.000000000000000000, 0.8660254037844387076, 1.000000000000000000, 0.8660254037844387076, 1.000000000000000000, 0.8660254037844387076, 1.000000000000000000, 0.8660254037844387076, 1.000000000000000000, 0.8660254037844387076, 1.000000000000000000, 0.8660254037844387076, 1.000000000000000000, 0.8660254037844387076, 1.000000000000000000, 0.8660254037844387076, 1.000000000000000000, 0.8660254037844387076, 1.000000000000000000, 0.8660254037844387076, 1.000000000000000000, 0.8660254037844387076, 1.000000000000000000, 0.8660254037844387076, 1.000000000000000000, 0.8660254037844387076, 1.000000000000000000, 0.8660254037844387076, 1.000000000000000000, 0.8660254037844387076, 1.000000000000000000, 0.8660254037844387076, 1.000000000000000000, 0.8660254037844387076, 1.000000000000000000, 0.8660254037844387076, 1.000000000000000000, 0.8660254037844387076, 1.000000000000000000, 0.8660254037844387076, 1.000000000000000000, 0.8660254037844387076, 1.000000000000000000, 0.8660254037844387076, 1.000000000000000000, 0.8660254037844387076, 1.000000000000000000, 0.8660254037844387076, 1.000000000000000000, 0.8660254037844387076, 1.000000000000000000, 0.8660254037844387076, 1.000000000000000000, 0.8660254037844387076, 1.000000000000000000, 0.8660254037844387076, 1.000000000000000000, 0.8660254037844387076, 1.000000000000000000, 0.8660254037844387076, 1.000000000000000000, 0.8660254037844387076, 1.000000000000000000, 0.8660254037844387076, 1.000000000000000000, 0.8660254037844387076, 1.000000000000000000, 0.8660254037844387076, 1.000000000000000000, 0.8660254037844387076, 1.000000000000000000, 0.8660254037844387076, 1.000000000000000000, 0.8660254037844387076, 1.000000000000000000, 0.8660254037844387076, 1.000000000000000000, 0.8660254037844387076, 1.000000000000000000, 0.8660254037844387076, 1.000000000000000000, 0.8660254037844387076, 1.000000000000000000, 0.8660254037844387076, 1.000000000000000000, 0.8660254037844387076, 1.000000000000000000, 0.8660254037844387076, 1.000000000000000000, 0.8660254037844387076, 1.000000000000000000, 0.8660254037844387076, 1.000000000000000000, 0.8660254037844387076, 1.000000000000000000, 0.8660254037844387076, 1.000000000000000000, 0.8660254037844387076, 1.000000000000000000, 0.8660254037844387076, 1.000000000000000000, 0.8660254037844387076, 1.000000000000000000, 0.8660254037844387076, 1.000000000000000000, 0.8660254037844387076, 1.000000000000000000, 0.8660254037844387076, 1.000000000000000000, 0.8660254037844387076, 1.000000000000000000, 0.8660254037844387076, 1.000000000000000000, 0.8660254037844387076, 1.000000000000000000, 0.8660254037844387076, 1.000000000000000000, 0.8660254037844387076, 1.000000000000000000, 0.8660254037844387076, 1.000000000000000000),
 ( 1.000000000000000000, 0.8660254037844387076, 1.000000000000000000, 0.8660254037844387076, 1.000000000000000000, 0.8660254037844387076, 1.000000000000000000, 0.8660254037844387076, 1.000000000000000000, 0.8660254037844387076, 1.000000000000000000, 0.8660254037844387076, 1.000000000000000000, 0.8660254037844387076, 1.000000000000000000, 0.8660254037844387076, 1.000000000000000000, 0.8660254037844387076, 1.000000000000000000, 0.8660254037844387076, 1.000000000000000000, 0.8660254037844387076, 1.000000000000000000, 0.8660254037844387076, 1.000000000000000000, 0.8660254037844387076, 1.000000000000000000, 0.8660254037844387076, 1.000000000000000000, 0.8660254037844387076, 1.000000000000000000, 0.8660254037844387076, 1.000000000000000000, 0.8660254037844387076, 1.000000000000000000, 0.8660254037844387076, 1.000000000000000000, 0.8660254037844387076, 1.000000000000000000, 0.8660254037844387076, 1.000000000000000000, 0.8660254037844387076, 1.000000000000000000, 0.8660254037844387076, 1.000000000000000000, 0.8660254037844387076, 1.000000000000000000, 0.8660254037844387076, 1.000000000000000000, 0.8660254037844387076, 1.000000000000000000, 0.8660254037844387076, 1.000000000000000000, 0.8660254037844387076, 1.000000000000000000, 0.8660254037844387076, 1.000000000000000000, 0.8660254037844387076, 1.000000000000000000, 0.8660254037844387076, 1.000000000000000000, 0.8660254037844387076, 1.000000000000000000, 0.8660254037844387076, 1.000000000000000000, 0.8660254037844387076, 1.000000000000000000, 0.8660254037844387076, 1.000000000000000000, 0.8660254037844387076, 1.000000000000000000, 0.8660254037844387076, 1.000000000000000000, 0.8660254037844387076, 1.000000000000000000, 0.8660254037844387076, 1.000000000000000000, 0.8660254037844387076, 1.000000000000000000, 0.8660254037844387076, 1.000000000000000000, 0.8660254037844387076, 1.000000000000000000, 0.8660254037844387076, 1.000000000000000000, 0.8660254037844387076, 1.000000000000000000, 0.8660254037844387076, 1.000000000000000000, 0.8660254037844387076, 1.000000000000000000, 0.8660254037844387076, 1.000000000000000000, 0.8660254037844387076, 1.000000000000000000, 0.8660254037844387076, 1.000000000000000000, 0.8660254037844387076, 1.000000000000000000, 0.8660254037844387076, 1.000000000000000000, 0.8660254037844387076, 1.000000000000000000, 0.8660254037844387076, 1.000000000000000000, 0.8660254037844387076, 1.000000000000000000, 0.8660254037844387076, 1.000000000000000000, 0.8660254037844387076, 1.000000000000000000, 0.8660254037844387076, 1.000000000000000000, 0.8660254037844387076, 1.000000000000000000, 0.8660254037844387076, 1.000000000000000000, 0.8660254037844387076, 1.000000000000000000, 0.8660254037844387076, 1.000000000000000000, 0.8660254037844387076, 1.000000000000000000, 0.8660254037844387076, 1.000000000000000000, 0.8660254037844387076, 1.000000000000000000, 0.8660254037844387076, 1.000000000000000000, 0.8660254037844387076, 1.000000000000000000, 0.8660254037844387076, 1.000000000000000000, 0.8660254037844387076, 1.000000000000000000, 0.8660254037844387076, 1.000000000000000000, 0.8660254037844387076, 1.000000000000000000, 0.8660254037844387076, 1.000000000000000000, 0.8660254037844387076, 1.000000000000000000, 0.8660254037844387076, 1.000000000000000000, 0.8660254037844387076, 1.000000000000000000, 0.8660254037844387076, 1.000000000000000000, 0.8660254037844387076, 1.000000000000000000, 0.8660254037844387076, 1.000000000000000000, 0.8660254037844387076, 1.000000000000000000, 0.8660254037844387076, 1.000000000000000000, 0.8660254037844387076, 1.000000000000000000, 0.8660254037844387076, 1.000000000000000000, 0.8660254037844387076, 1.000000000000000000, 0.8660254037844387076, 1.000000000000000000, 0.8660254037844387076, 1.000000000000000000, 0.8660254037844387076, 1.000000000000000000, 0.8660254037844387076, 1.000000000000000000, 0.8660254037844387076, 1.000000000000000000, 0.8660254037844387076, 1.000000000000000000, 0.8660254037844387076, 1.000000000000000000, 0.8660254037844387076, 1.000000000000000000, 0.8660254037844387076, 1.000000000000000000, 0.8660254037844387076, 1.000000000000000000, 0.8660254037844387076, 1.000000000000000000, 0.8660254037844387076, 1.000000000000000000, 0.8660254037844387076, 1.000000000000000000, 0.8660254037844387076, 1.000000000000000000, 0.8660254037844387076, 1.000000000000000000, 0.8660254037844387076, 1.000000000000000000, 0.8660254037844387076, 1.000000000000000000, 0.8660254037844387076, 1.000000000000000000, 0.8660254037844387076, 1.000000000000000000, 0.8660254037844387076, 1.000000000000000000, 0.8660254037844387076, 1.000000000000000000, 0.8660254037844387076, 1.000000000000000000, 0.8660254037844387076, 1.000000000000000000, 0.8660254037844387076, 1.000000000000000000, 0.8660254037844387076, 1.000000000000000000, 0.8660254037844387076, 1.000000000000000000, 0.8660254037844387076, 1.000000000000000000, 0.8660254037844387076, 1.000000000000000000, 0.8660254037844387076, 1.000000000000000000, 0.8660254037844387076, 1.000000000000000000, 0.8660254037844387076, 1.000000000000000000, 0.8660254037844387076, 1.000000000000000000, 0.8660254037844387076, 1.000000000000000000, 0.8660254037844387076, 1.000000000000000000, 0.8660254037844387076, 1.000000000000000000, 0.8660254037844387076, 1.000000000000000000, 0.8660254037844387076, 1.000000000000000000, 0.8660254037844387076, 1.000000000000000000, 0.8660254037844387076, 1.000000000000000000, 0.8660254037844387076, 1.000000000000000000, 0.8660254037844387076, 1.000000000000000000, 0.8660254037844387076, 1.000000000000000000, 0.8660254037844387076, 1.000000000000000000, 0.8660254037844387076, 1.000000000000000000, 0.8660254037844387076, 1.000000000000000000, 0.8660254037844387076, 1.000000000000000000, 0.8660254037844387076, 1.000000000000000000, 0.8660254037844387076, 1.000000000000000000, 0.8660254037844387076, 1.000000000000000000, 0.8660254037844387076, 1.000000000000000000, 0.8660254037844387076, 1.000000000000000000, 0.8660254037844387076, 1.000000000000000000, 0.8660254037844387076, 1.000000000000000000, 0.8660254037844387076, 1.000000000000000000, 0.8660254037844387076, 1.000000000000000000, 0.8660254037844387076, 1.000000000000000000, 0.8660254037844387076, 1.000000000000000000, 0.8660254037844387076, 1.000000000000000000, 0.8660254037844387076, 1.000000000000000000, 0.8660254037844387076, 1.000000000000000000, 0.8660254037844387076, 1.000000000000000000, 0.8660254037844387076, 1.000000000000000000, 0.8660254037844387076, 1.000000000000000000, 0.8660254037844387076, 1.000000000000000000, 0.8660254037844387076, 1.000000000000000000, 0.8660254037844387076, 1.000000000000000000, 0.8660254037844387076, 1.000000000000000000, 0.8660254037844387076, 1.000000000000000000, 0.8660254037844387076, 1.000000000000000000, 0.8660254037844387076, 1.000000000000000000, 0.8660254037844387076, 1.000000000000000000, 0.8660254037844387076, 1.000000000000000000, 0.8660254037844387076, 1.000000000000000000, 0.8660254037844387076, 1.000000000000000000, 0.8660254037844387076, 1.000000000000000000, 0.8660254037844387076, 1.000000000000000000, 0.8660254037844387076, 1.000000000000000000, 0.8660254037844387076, 1.000000000000000000, 0.8660254037844387076, 1.000000000000000000, 0.8660254037844387076, 1.000000000000000000, 0.8660254037844387076, 1.000000000000000000, 0.8660254037844387076, 1.000000000000000000, 0.8660254037844387076, 1.000000000000000000, 0.8660254037844387076, 1.000000000000000000, 0.8660254037844387076, 1.000000000000000000, 0.8660254037844387076, 1.000000000000000000, 0.8660254037844387076, 1.000000000000000000, 0.8660254037844387076, 1.000000000000000000, 0.8660254037844387076, 1.000000000000000000, 0.8660254037844387076, 1.000000000000000000, 0.8660254037844387076, 1.000000000000000000, 0.8660254037844387076, 1.000000000000000000, 0.8660254037844387076, 1.000000000000000000, 0.8660254037844387076, 1.000000000000000000, 0.8660254037844387076, 1.000000000000000000, 0.8660254037844387076, 1.000000000000000000, 0.8660254037844387076, 1.000000000000000000, 0.8660254037844387076, 1.000000000000000000, 0.8660254037844387076, 1.000000000000000000, 0.8660254037844387076, 1.000000000000000000, 0.8660254037844387076, 1.000000000000000000, 0.8660254037844387076, 1.000000000000000000, 0.8660254037844387076, 1.000000000000000000, 0.8660254037844387076, 1.000000000000000000, 0.8660254037844387076, 1.000000000000000000, 0.8660254037844387076, 1.000000000000000000, 0.8660254037844387076, 1.000000000000000000, 0.8660254037844387076, 1.000000000000000000, 0.8660254037844387076, 1.000000000000000000, 0.8660254037844387076, 1.000000000000000000, 0.8660254037844387076, 1.000000000000000000, 0.8660254037844387076, 1.000000000000000000, 0.8660254037844387076, 1.000000000000000000, 0.8660254037844387076, 1.000000000000000000, 0.8660254037844387076, 1.000000000000000000, 0.8660254037844387076, 1.000000000000000000, 0.8660254037844387076, 1.000000000000000000, 0.8660254037844387076, 1.000000000000000000, 0.8660254037844387076, 1.000000000000000000, 0.8660254037844387076, 1.000000000000000000, 0.8660254037844387076, 1.000000000000000000, 0.8660254037844387076, 1.000000000000000000, 0.8660254037844387076, 1.000000000000000000, 0.8660254037844387076, 1.000000000000000000, 0.8660254037844387076, 1.000000000000000000, 0.8660254037844387076, 1.000000000000000000, 0.8660254037844387076, 1.000000000000000000, 0.8660254037844387076, 1.000000000000000000, 0.8660254037844387076, 1.000000000000000000, 0.8660254037844387076, 1.000000000000000000, 0.8660254037844387076, 1.000000000000000000, 0.8660254037844387076, 1.000000000000000000, 0.8660254037844387076, 1.000000000000000000, 0.8660254037844387076, 1.000000000000000000, 0.8660254037844387076, 1.000000000000000000, 0.8660254037844387076, 1.000000000000000000, 0.8660254037844387076, 1.000000000000000000, 0.8660254037844387076, 1.000000000000000000, 0.8660254037844387076, 1.000000000000000000, 0.8660254037844387076, 1.000000000000000000, 0.8660254037844387076, 1.000000000000000000, 0.8660254037844387076, 1.000000000000000000, 0.8660254037844387076, 1.000000000000000000, 0.8660254037844387076, 1.000000000000000000, 0.8660254037844387076, 1.000000000000000000, 0.8660254037844387076, 1.000000000000000000, 0.8660254037844387076, 1.000000000000000000, 0.8660254037844387076, 1.000000000000000000, 0.8660254037844387076, 1.000000000000000000, 0.8660254037844387076, 1.000000000000000000, 0.8660254037844387076, 1.000000000000000000, 0.8660254037844387076, 1.000000000000000000, 0.8660254037844387076, 1.000000000000000000, 0.8660254037844387076, 1.000000000000000000, 0.8660254037844387076, 1.000000000000000000, 0.8660254037844387076, 1.000000000000000000, 0.8660254037844387076, 1.000000000000000000, 0.8660254037844387076, 1.000000000000000000, 0.8660254037844387076, 1.000000000000000000, 0.8660254037844387076, 1.000000000000000000, 0.8660254037844387076, 1.000000000000000000, 0.8660254037844387076, 1.000000000000000000, 0.8660254037844387076, 1.000000000000000000, 0.8660254037844387076, 1.000000000000000000, 0.8660254037844387076, 1.000000000000000000, 0.8660254037844387076, 1.000000000000000000, 0.8660254037844387076, 1.000000000000000000, 0.8660254037844387076, 1.000000000000000000, 0.8660254037844387076, 1.000000000000000000, 0.8660254037844387076, 1.000000000000000000, 0.8660254037844387076, 1.000000000000000000, 0.8660254037844387076, 1.000000000000000000, 0.8660254037844387076, 1.000000000000000000, 0.8660254037844387076, 1.000000000000000000, 0.8660254037844387076, 1.000000000000000000, 0.8660254037844387076, 1.000000000000000000, 0.8660254037844387076, 1.000000000000000000, 0.8660254037844387076, 1.000000000000000000, 0.8660254037844387076, 1.000000000000000000, 0.8660254037844387076, 1.000000000000000000, 0.8660254037844387076, 1.000000000000000000, 0.8660254037844387076, 1.000000000000000000, 0.8660254037844387076, 1.000000000000000000, 0.8660254037844387076, 1.000000000000000000, 0.8660254037844387076, 1.000000000000000000, 0.8660254037844387076, 1.000000000000000000, 0.8660254037844387076, 1.000000000000000000, 0.8660254037844387076, 1.000000000000000000, 0.8660254037844387076, 1.000000000000000000, 0.8660254037844387076, 1.000000000000000000, 0.8660254037844387076, 1.000000000000000000, 0.8660254037844387076, 1.000000000000000000, 0.8660254037844387076, 1.000000000000000000, 0.8660254037844387076, 1.000000000000000000, 0.8660254037844387076, 1.000000000000000000, 0.8660254037844387076, 1.000000000000000000, 0.8660254037844387076, 1.000000000000000000, 0.8660254037844387076, 1.000000000000000000, 0.8660254037844387076, 1.000000000000000000, 0.8660254037844387076, 1.000000000000000000, 0.8660254037844387076, 1.000000000000000000, 0.8660254037844387076, 1.000000000000000000, 0.8660254037844387076, 1.000000000000000000, 0.8660254037844387076, 1.000000000000000000, 0.8660254037844387076, 1.000000000000000000, 0.8660254037844387076, 1.000000000000000000, 0.8660254037844387076, 1.000000000000000000, 0.8660254037844387076, 1.000000000000000000, 0.8660254037844387076, 1.000000000000000000, 0.8660254037844387076, 1.000000000000000000, 0.8660254037844387076, 1.000000000000000000, 0.8660254037844387076, 1.000000000000000000, 0.8660254037844387076, 1.000000000000000000, 0.8660254037844387076, 1.000000000000000000, 0.8660254037844387076, 1.000000000000000000, 0.8660254037844387076, 1.000000000000000000, 0.8660254037844387076, 1.000000000000000000, 0.8660254037844387076, 1.000000000000000000, 0.8660254037844387076, 1.000000000000000000, 0.8660254037844387076, 1.000000000000000000, 0.8660254037844387076, 1.000000000000000000, 0.8660254037844387076, 1.000000000000000000, 0.8660254037844387076, 1.000000000000000000, 0.8660254037844387076, 1.000000000000000000, 0.8660254037844387076, 1.000000000000000000, 0.8660254037844387076, 1.000000000000000000, 0.8660254037844387076, 1.000000000000000000, 0.8660254037844387076, 1.000000000000000000, 0.8660254037844387076, 1.000000000000000000, 0.8660254037844387076, 1.000000000000000000, 0.8660254037844387076, 1.000000000000000000, 0.8660254037844387076, 1.000000000000000000, 0.8660254037844387076, 1.000000000000000000, 0.8660254037844387076, 1.000000000000000000, 0.8660254037844387076, 1.000000000000000000, 0.8660254037844387076, 1.000000000000000000, 0.8660254037844387076, 1.000000000000000000, 0.8660254037844387076, 1.000000000000000000, 0.8660254037844387076, 1.000000000000000000, 0.8660254037844387076, 1.000000000000000000, 0.8660254037844387076, 1.000000000000000000, 0.8660254037844387076, 1.000000000000000000, 0.8660254037844387076, 1.000000000000000000, 0.8660254037844387076, 1.000000000000000000, 0.8660254037844387076, 1.000000000000000000, 0.8660254037844387076, 1.000000000000000000, 0.8660254037844387076, 1.000000000000000000, 0.8660254037844387076, 1.000000000000000000, 0.8660254037844387076, 1.000000000000000000, 0.8660254037844387076, 1.000000000000000000, 0.8660254037844387076, 1.000000000000000000, 0.8660254037844387076, 1.000000000000000000, 0.8660254037844387076, 1.000000000000000000, 0.8660254037844387076, 1.000000000000000000, 0.8660254037844387076, 1.000000000000000000, 0.8660254037844387076, 1.000000000000000000, 0.8660254037844387076, 1.000000000000000000, 0.8660254037844387076, 1.000000000000000000, 0.8660254037844387076, 1.000000000000000000, 0.8660254037844387076, 1.000000000000000000, 0.8660254037844387076, 1.000000000000000000, 0.8660254037844387076, 1.000000000000000000, 0.8660254037844387076, 1.000000000000000000, 0.8660254037844387076, 1.000000000000000000, 0.8660254037844387076, 1.000000000000000000, 0.8660254037844387076, 1.000000000000000000, 0.8660254037844387076, 1.000000000000000000, 0.8660254037844387076, 1.000000000000000000, 0.8660254037844387076, 1.000000000000000000, 0.8660254037844387076, 1.000000000000000000, 0.8660254037844387076, 1.000000000000000000, 0.8660254037844387076, 1.000000000000000000, 0.8660254037844387076, 1.000000000000000000, 0.8660254037844387076, 1.000000000000000000, 0.8660254037844387076, 1.000000000000000000, 0.8660254037844387076, 1.000000000000000000, 0.8660254037844387076, 1.000000000000000000, 0.8660254037844387076, 1.000000000000000000, 0.8660254037844387076, 1.000000000000000000) ) ) 
 REPRESENTATION_ITEM ( '' )  SURFACE ( )  );
#51496 = CARTESIAN_POINT ( 'NONE',  ( 4.243569643749999010, 10.22187500061451892, -32.45002607614398471 ) ) ;
#51497 = CYLINDRICAL_SURFACE ( 'NONE', #1762, 4.000000000000000000 ) ;
#51498 = CARTESIAN_POINT ( 'NONE',  ( 3.075000001229035718, 2.886751345948126879, 4.999999999999999112 ) ) ;
#51499 = FACE_OUTER_BOUND ( 'NONE', #65132, .T. ) ;
#51500 = CARTESIAN_POINT ( 'NONE',  ( 19.09687500061451360, -3.027376345333614438, 5.243569643749998122 ) ) ;
#51501 = EDGE_CURVE ( 'NONE', #8342, #58790, #46310, .T. ) ;
#51502 = LINE ( 'NONE', #57746, #58659 ) ;
#51503 = CARTESIAN_POINT ( 'NONE',  ( 13.56562500061451892, 3.027376345333611329, 5.243569643749999010 ) ) ;
#51504 = CARTESIAN_POINT ( 'NONE',  ( 8.756250001229034297, 4.330127018922192761, -2.499999999999997780 ) ) ;
#51505 = CARTESIAN_POINT ( 'NONE',  ( 30.00000000000000000, 0.000000000000000000, 0.000000000000000000 ) ) ;
#51506 = CARTESIAN_POINT ( 'NONE',  ( 29.52187500061451431, -6.054752690667223547, -1.112240025338166033E-15 ) ) ;
#51507 = CARTESIAN_POINT ( 'NONE',  ( 27.15937500061451360, 0.000000000000000000, 5.243569643749999010 ) ) ;
#51508 = CARTESIAN_POINT ( 'NONE',  ( 18.38437500061451857, 5.492252693125287522, 3.363034840372157021E-16 ) ) ;
#51509 = CARTESIAN_POINT ( 'NONE',  ( 13.56562500061451892, 3.027376345333611329, 5.243569643749999010 ) ) ;
#51510 = CARTESIAN_POINT ( 'NONE',  ( 10.35937500061451644, 4.541064518000418104, -2.621784821874998173 ) ) ;
#51511 = ORIENTED_EDGE ( 'NONE', *, *, #11164, .F. ) ;
#51512 = AXIS2_PLACEMENT_3D ( 'NONE', #6598, #29128, #51661 ) ;
#51513 = DIRECTION ( 'NONE',  ( 0.000000000000000000, 0.000000000000000000, -1.000000000000000000 ) ) ;
#51514 = CARTESIAN_POINT ( 'NONE',  ( 20.01562500061451644, -6.054752690667223547, -1.112240025338166033E-15 ) ) ;
#51515 = CARTESIAN_POINT ( 'NONE',  ( 3.108217618452874476, 3.916501402570781387, -3.486551214670091881 ) ) ;
#51516 = CARTESIAN_POINT ( 'NONE',  ( 20.77500000000000213, 6.123233995736764310E-16, -4.999999999999998224 ) ) ;
#51517 = CARTESIAN_POINT ( 'NONE',  ( 10.12500000000000178, 4.330127018922191873, 2.499999999999999556 ) ) ;
#51518 = CARTESIAN_POINT ( 'NONE',  ( 20.70000000122903216, -2.886751345948129988, 4.999999999999997335 ) ) ;
#51519 = CARTESIAN_POINT ( 'NONE',  ( 15.25312500061451715, 4.541064518000418104, -2.621784821874998173 ) ) ;
#51520 = CARTESIAN_POINT ( 'NONE',  ( 10.24687500061451395, 4.119189519843966529, -2.378215178124998275 ) ) ;
#51521 = ORIENTED_EDGE ( 'NONE', *, *, #20103, .F. ) ;
#51522 = CARTESIAN_POINT ( 'NONE',  ( 18.48750000000000071, -2.886751345948125991, -5.000000000000000000 ) ) ;
#51523 = CARTESIAN_POINT ( 'NONE',  ( 20.92500000000000071, 4.330127018922191873, 2.499999999999999556 ) ) ;
#51524 = CARTESIAN_POINT ( 'NONE',  ( 18.60937500061451644, 0.000000000000000000, 5.243569643749999010 ) ) ;
#51525 = CARTESIAN_POINT ( 'NONE',  ( 24.62812500061451715, 6.421520780324663323E-16, -5.243569643749999010 ) ) ;
#51526 = ORIENTED_EDGE ( 'NONE', *, *, #16255, .F. ) ;
#51527 = CARTESIAN_POINT ( 'NONE',  ( 19.72499999999999787, -4.330127018922194537, 2.499999999999995559 ) ) ;
#51528 = CARTESIAN_POINT ( 'NONE',  ( 7.415625000614516793, -6.054752690667223547, -1.112240025338166033E-15 ) ) ;
#51529 = CARTESIAN_POINT ( 'NONE',  ( 4.898587196589411843E-16, 20.00000000000000000, 33.99999999999999289 ) ) ;
#51530 = CARTESIAN_POINT ( 'NONE',  ( 13.53749999999999964, -2.886751345948125991, -5.000000000000000000 ) ) ;
#51531 = CARTESIAN_POINT ( 'NONE',  ( -4.243569643749999898, 17.06562500061451360, 27.54997392385601529 ) ) ;
#51532 = CARTESIAN_POINT ( 'NONE',  ( 28.75312500061451715, 4.541064518000418104, -2.621784821874998173 ) ) ;
#51533 = CARTESIAN_POINT ( 'NONE',  ( -3.756430356249999214, 15.97812499938548392, 27.83122392262697531 ) ) ;
#51534 = CARTESIAN_POINT ( 'NONE',  ( 25.69687500061451502, 6.054752690667223547, 3.707466751127219781E-16 ) ) ;
#51535 = ORIENTED_EDGE ( 'NONE', *, *, #33859, .T. ) ;
#51536 = CARTESIAN_POINT ( 'NONE',  ( 22.75312500061451360, -4.541064518000417216, -2.621784821875001281 ) ) ;
#51537 = CARTESIAN_POINT ( 'NONE',  ( 24.98437500061451644, -4.541064518000419881, 2.621784821874995952 ) ) ;
#51538 = CARTESIAN_POINT ( 'NONE',  ( -4.243569643749999898, 18.00312500061459176, -30.00000000000000000 ) ) ;
#51539 = CARTESIAN_POINT ( 'NONE',  ( 11.21250000000000036, -5.773502691896255534, -1.060575238724906372E-15 ) ) ;
#51540 = CARTESIAN_POINT ( 'NONE',  ( 9.665625000614515017, -6.054752690667223547, -1.112240025338166033E-15 ) ) ;
#51541 = CARTESIAN_POINT ( 'NONE',  ( 29.44687500061451502, -2.746126346562646425, 4.756430356249996549 ) ) ;
#51542 = CARTESIAN_POINT ( 'NONE',  ( 28.49062500061451431, -3.027376345333614438, 5.243569643749998122 ) ) ;
#51543 = CARTESIAN_POINT ( 'NONE',  ( 26.01562500061451289, 3.027376345333612662, -5.243569643749998122 ) ) ;
#51544 = CARTESIAN_POINT ( 'NONE',  ( 27.68437500061451573, -2.746126346562641984, -4.756430356249999214 ) ) ;
#51545 = CARTESIAN_POINT ( 'NONE',  ( 13.09687500061451892, 5.492252693125287522, 3.363034840372157021E-16 ) ) ;
#51546 = CARTESIAN_POINT ( 'NONE',  ( 18.30937500061451928, -4.541064518000417216, -2.621784821875001281 ) ) ;
#51547 = CARTESIAN_POINT ( 'NONE',  ( 4.243569643749999898, 13.29687500061451644, 32.45002607614398471 ) ) ;
#51548 = CARTESIAN_POINT ( 'NONE',  ( 18.83437500061451431, 6.421520780324663323E-16, -5.243569643749999010 ) ) ;
#51549 = CARTESIAN_POINT ( 'NONE',  ( 26.93437500061451573, 6.421520780324663323E-16, -5.243569643749999010 ) ) ;
#51550 = CARTESIAN_POINT ( 'NONE',  ( -3.000416591977282496E-16, 17.04687500061451999, 25.09994784771203058 ) ) ;
#51551 = CARTESIAN_POINT ( 'NONE',  ( 6.590625000614518392, -3.027376345333610441, -5.243569643749999898 ) ) ;
#51552 = CARTESIAN_POINT ( 'NONE',  ( -3.999999999999999112, 19.06250000000000000, 27.69059892324149885 ) ) ;
#51553 = CARTESIAN_POINT ( 'NONE',  ( 5.671875000614519102, -6.054752690667223547, -1.112240025338166033E-15 ) ) ;
#51554 = CARTESIAN_POINT ( 'NONE',  ( 5.915625000614515905, 3.027376345333611329, 5.243569643749999010 ) ) ;
#51555 = CARTESIAN_POINT ( 'NONE',  ( 10.73437500061451644, 6.421520780324663323E-16, -5.243569643749999010 ) ) ;
#51556 =( NAMED_UNIT ( * ) PLANE_ANGLE_UNIT ( ) SI_UNIT ( $, .RADIAN. ) );
#51557 = CARTESIAN_POINT ( 'NONE',  ( 18.52500000122903145, -5.773502691896255534, -1.060575238724906372E-15 ) ) ;
#51558 = CARTESIAN_POINT ( 'NONE',  ( 6.384375000614516793, 4.541064518000418104, 2.621784821874999949 ) ) ;
#51559 = CARTESIAN_POINT ( 'NONE',  ( 6.440625000614517148, -3.027376345333614438, 5.243569643749998122 ) ) ;
#51560 = CARTESIAN_POINT ( 'NONE',  ( 5.390625000614518214, 6.054752690667223547, 3.707466751127219781E-16 ) ) ;
#51561 = CARTESIAN_POINT ( 'NONE',  ( 22.66875000122902861, 2.886751345948129099, -4.999999999999998224 ) ) ;
#51562 = CARTESIAN_POINT ( 'NONE',  ( 16.20937500061451786, 4.541064518000418104, -2.621784821874998173 ) ) ;
#51563 = DIRECTION ( 'NONE',  ( -0.000000000000000000, -0.000000000000000000, -1.000000000000000000 ) ) ;
#51564 = ORIENTED_EDGE ( 'NONE', *, *, #18886, .T. ) ;
#51565 = CARTESIAN_POINT ( 'NONE',  ( 24.74062500061451786, 6.054752690667223547, 3.707466751127219781E-16 ) ) ;
#51566 = CARTESIAN_POINT ( 'NONE',  ( 9.403125000614517504, 4.541064518000418104, -2.621784821874998173 ) ) ;
#51567 = CARTESIAN_POINT ( 'NONE',  ( 27.98437500061451289, 4.541064518000418104, 2.621784821874999949 ) ) ;
#51568 = CARTESIAN_POINT ( 'NONE',  ( 9.665625000614515017, -6.054752690667223547, -1.112240025338166033E-15 ) ) ;
#51569 = CARTESIAN_POINT ( 'NONE',  ( -3.000416591977282496E-16, 10.29687500061451644, -34.90005215228797653 ) ) ;
#51570 = CARTESIAN_POINT ( 'NONE',  ( 13.20000000122903394, -2.886751345948125991, -5.000000000000000000 ) ) ;
#51571 = ADVANCED_FACE ( 'NONE', ( #46207 ), #63764, .T. ) ;
#51572 = CARTESIAN_POINT ( 'NONE',  ( 27.06562500061451004, 3.027376345333611329, 5.243569643749999010 ) ) ;
#51573 = CARTESIAN_POINT ( 'NONE',  ( -2.121784821874999949, 12.97812500061451679, -33.67503911421598417 ) ) ;
#51574 = CARTESIAN_POINT ( 'NONE',  ( 13.05000000122903536, -2.886751345948129988, 4.999999999999997335 ) ) ;
#51575 = CARTESIAN_POINT ( 'NONE',  ( 11.55000000000000071, 0.000000000000000000, 4.999999999999998224 ) ) ;
#51576 = CARTESIAN_POINT ( 'NONE',  ( 19.82812500061451644, 4.541064518000418104, 2.621784821874999949 ) ) ;
#51577 = CARTESIAN_POINT ( 'NONE',  ( 6.046875000614519102, -3.027376345333614438, 5.243569643749998122 ) ) ;
#51578 = CARTESIAN_POINT ( 'NONE',  ( 20.51249999999999929, 2.886751345948126879, 4.999999999999999112 ) ) ;
#51579 = CARTESIAN_POINT ( 'NONE',  ( 6.675000001229034474, 2.886751345948126879, 4.999999999999999112 ) ) ;
#51580 = CARTESIAN_POINT ( 'NONE',  ( 16.98750000122903359, 4.330127018922191873, 2.499999999999999556 ) ) ;
#51581 = AXIS2_PLACEMENT_3D ( 'NONE', #20488, #25689, #64840 ) ;
#51582 = CARTESIAN_POINT ( 'NONE',  ( 12.40312500061451573, -4.541064518000417216, -2.621784821875001281 ) ) ;
#51583 = CARTESIAN_POINT ( 'NONE',  ( 15.10312500061451502, -4.541064518000417216, -2.621784821875001281 ) ) ;
#51584 = CARTESIAN_POINT ( 'NONE',  ( 26.06250000122903288, 0.000000000000000000, 4.999999999999998224 ) ) ;
#51585 = CARTESIAN_POINT ( 'NONE',  ( 19.68750000000000355, -2.886751345948129988, 4.999999999999997335 ) ) ;
#51586 = CARTESIAN_POINT ( 'NONE',  ( 24.53437500061451715, -4.541064518000419881, 2.621784821874995952 ) ) ;
#51587 = DIRECTION ( 'NONE',  ( 0.000000000000000000, 0.000000000000000000, 1.000000000000000000 ) ) ;
#51588 = CARTESIAN_POINT ( 'NONE',  ( 10.08750000122903323, 6.123233995736764310E-16, -4.999999999999998224 ) ) ;
#51589 = CARTESIAN_POINT ( 'NONE',  ( 8.596875000614518925, 6.054752690667223547, 3.707466751127219781E-16 ) ) ;
#51590 = CARTESIAN_POINT ( 'NONE',  ( 25.43437500061451573, -4.541064518000419881, 2.621784821874995952 ) ) ;
#51591 = EDGE_CURVE ( 'NONE', #37967, #71135, #7394, .T. ) ;
#51592 = CARTESIAN_POINT ( 'NONE',  ( 3.046875000614519990, -3.027376345333610441, -5.243569643749999898 ) ) ;
#51593 = CARTESIAN_POINT ( 'NONE',  ( 24.10312500061451502, -4.541064518000417216, -2.621784821875001281 ) ) ;
#51594 = CARTESIAN_POINT ( 'NONE',  ( 27.38437500061451857, 6.421520780324663323E-16, -5.243569643749999010 ) ) ;
#51595 = CARTESIAN_POINT ( 'NONE',  ( -1.878215178124999163, 17.40312499938548285, 26.74683588394047007 ) ) ;
#51596 = CARTESIAN_POINT ( 'NONE',  ( 19.21875000122902932, 2.886751345948126879, 4.999999999999998224 ) ) ;
#51597 = CARTESIAN_POINT ( 'NONE',  ( 7.434375000614519280, -4.541064518000419881, 2.621784821874995952 ) ) ;
#51598 = FACE_OUTER_BOUND ( 'NONE', #48764, .T. ) ;
#51599 = CARTESIAN_POINT ( 'NONE',  ( 28.64062500061451289, -3.027376345333610441, -5.243569643749999898 ) ) ;
#51600 = CARTESIAN_POINT ( 'NONE',  ( 5.371875000614516615, 3.027376345333613106, -5.243569643749998122 ) ) ;
#51601 = DIRECTION ( 'NONE',  ( 0.000000000000000000, 1.000000000000000000, 0.000000000000000000 ) ) ;
#51602 = CARTESIAN_POINT ( 'NONE',  ( 29.04375000122903572, 5.773502691896255534, 3.535250795749688401E-16 ) ) ;
#51603 = CARTESIAN_POINT ( 'NONE',  ( 17.47499999999999787, -4.330127018922194537, 2.499999999999995559 ) ) ;
#51604 = ORIENTED_EDGE ( 'NONE', *, *, #12260, .T. ) ;
#51605 = CARTESIAN_POINT ( 'NONE',  ( 28.01249999999999574, 2.886751345948129099, -4.999999999999998224 ) ) ;
#51606 = CARTESIAN_POINT ( 'NONE',  ( 29.59687500061451715, -3.027376345333610441, -5.243569643749999898 ) ) ;
#51607 = EDGE_LOOP ( 'NONE', ( #62445, #63188, #67086, #63218 ) ) ;
#51608 = CARTESIAN_POINT ( 'NONE',  ( 15.59062500061451573, -3.027376345333610441, -5.243569643749999898 ) ) ;
#51609 = CARTESIAN_POINT ( 'NONE',  ( 5.690625000614516260, -3.027376345333610441, -5.243569643749999898 ) ) ;
#51610 = CARTESIAN_POINT ( 'NONE',  ( 20.14687500061451786, 4.119189519843966529, -2.378215178124998275 ) ) ;
#51611 = CARTESIAN_POINT ( 'NONE',  ( 5.334375000614517859, 6.421520780324663323E-16, -5.243569643749999010 ) ) ;
#51612 = CARTESIAN_POINT ( 'NONE',  ( 15.15000000122903323, 5.773502691896255534, 3.535250795749688894E-16 ) ) ;
#51613 = CARTESIAN_POINT ( 'NONE',  ( 21.30000000000000071, 4.330127018922192761, -2.499999999999997780 ) ) ;
#51614 = CARTESIAN_POINT ( 'NONE',  ( 28.83749999999999858, -2.886751345948125991, -5.000000000000000000 ) ) ;
#51615 = CARTESIAN_POINT ( 'NONE',  ( 4.696875000614518569, -3.027376345333614438, 5.243569643749998122 ) ) ;
#51616 = CARTESIAN_POINT ( 'NONE',  ( 9.196875000614518569, -3.027376345333614438, 5.243569643749998122 ) ) ;
#51617 = CARTESIAN_POINT ( 'NONE',  ( 21.42187500061451644, -6.054752690667223547, -1.112240025338166033E-15 ) ) ;
#51618 = DIRECTION ( 'NONE',  ( -0.000000000000000000, -1.000000000000000000, -0.000000000000000000 ) ) ;
#51619 = ORIENTED_EDGE ( 'NONE', *, *, #19740, .F. ) ;
#51620 = CARTESIAN_POINT ( 'NONE',  ( 3.046875000614519990, -3.027376345333610441, -5.243569643749999898 ) ) ;
#51621 = CARTESIAN_POINT ( 'NONE',  ( 5.587500000000003020, 5.773502691896255534, 3.535250795749688894E-16 ) ) ;
#51622 = CARTESIAN_POINT ( 'NONE',  ( 6.571875000614517681, -6.054752690667223547, -1.112240025338166033E-15 ) ) ;
#51623 = VECTOR ( 'NONE', #13554, 1000.000000000000000 ) ;
#51624 = CARTESIAN_POINT ( 'NONE',  ( 17.43750000000000355, -2.886751345948129988, 4.999999999999997335 ) ) ;
#51625 = CARTESIAN_POINT ( 'NONE',  ( 16.71562500061451573, 3.027376345333611329, 5.243569643749999010 ) ) ;
#51626 = CARTESIAN_POINT ( 'NONE',  ( 1.999999999999997335, 20.07499999999999929, 33.46410161513775705 ) ) ;
#51627 = CYLINDRICAL_SURFACE ( 'NONE', #25677, 4.999999999999998224 ) ;
#51628 = CARTESIAN_POINT ( 'NONE',  ( 20.52187500061451786, -5.492252693125287522, -1.008910452111647106E-15 ) ) ;
#51629 = CARTESIAN_POINT ( 'NONE',  ( 9.703125000614514661, -4.541064518000417216, -2.621784821875001281 ) ) ;
#51630 = CARTESIAN_POINT ( 'NONE',  ( 27.49687500061451217, 6.054752690667223547, 3.707466751127219781E-16 ) ) ;
#51631 = CARTESIAN_POINT ( 'NONE',  ( 27.45937500061451786, 4.541064518000418104, -2.621784821874998173 ) ) ;
#51632 = CARTESIAN_POINT ( 'NONE',  ( 8.175000000000002487, 6.123233995736764310E-16, -4.999999999999998224 ) ) ;
#51633 = CARTESIAN_POINT ( 'NONE',  ( 3.999999999999998668, 14.07500000122903572, 27.69059892324149175 ) ) ;
#51634 = CARTESIAN_POINT ( 'NONE',  ( 6.300000001229033586, -2.886751345948129988, 4.999999999999997335 ) ) ;
#51635 = CARTESIAN_POINT ( 'NONE',  ( 17.44687500061451857, -3.027376345333610441, -5.243569643749999898 ) ) ;
#51636 = CARTESIAN_POINT ( 'NONE',  ( 12.98437500061451821, 6.421520780324663323E-16, -5.243569643749999010 ) ) ;
#51637 = CARTESIAN_POINT ( 'NONE',  ( -3.964499721297434665, 3.046849790701494420, -30.54937706598502700 ) ) ;
#51638 = VERTEX_POINT ( 'NONE', #46195 ) ;
#51639 = CARTESIAN_POINT ( 'NONE',  ( 14.35312500061451679, 4.541064518000418104, -2.621784821874998173 ) ) ;
#51640 = CARTESIAN_POINT ( 'NONE',  ( 27.15000000122902790, -2.886751345948125991, -5.000000000000000000 ) ) ;
#51641 = CARTESIAN_POINT ( 'NONE',  ( 12.45937500061451786, -4.541064518000417216, -2.621784821875001281 ) ) ;
#51642 = LINE ( 'NONE', #23913, #52417 ) ;
#51643 = CARTESIAN_POINT ( 'NONE',  ( 13.64062500061451644, -3.027376345333614438, 5.243569643749998122 ) ) ;
#51644 = CARTESIAN_POINT ( 'NONE',  ( 20.98125000122903216, 4.330127018922191873, 2.499999999999999556 ) ) ;
#51645 = CARTESIAN_POINT ( 'NONE',  ( 23.97187500061451360, 3.027376345333611329, 5.243569643749999010 ) ) ;
#51646 = CARTESIAN_POINT ( 'NONE',  ( 2.880239685073342937, -4.087086472263080417, 3.284934485538541171 ) ) ;
#51647 = CARTESIAN_POINT ( 'NONE',  ( 11.32500000122903394, -5.773502691896255534, -1.060575238724906372E-15 ) ) ;
#51648 = DIRECTION ( 'NONE',  ( -1.000000000000000000, -0.000000000000000000, -0.000000000000000000 ) ) ;
#51649 = CARTESIAN_POINT ( 'NONE',  ( 4.648177544792955741E-15, 14.18750000000000000, 33.99999999999999289 ) ) ;
#51650 = CARTESIAN_POINT ( 'NONE',  ( -4.243569643749999898, 16.22187500061452070, -32.45002607614398471 ) ) ;
#51651 = CARTESIAN_POINT ( 'NONE',  ( 19.24687500061452283, -3.027376345333610441, -5.243569643749999898 ) ) ;
#51652 = CARTESIAN_POINT ( 'NONE',  ( 19.42500000122903714, -5.773502691896255534, -1.060575238724906372E-15 ) ) ;
#51653 = CARTESIAN_POINT ( 'NONE',  ( 13.92187500061451644, 3.027376345333613106, -5.243569643749998122 ) ) ;
#51654 = CARTESIAN_POINT ( 'NONE',  ( 2.121784821875001281, 11.00937500061451857, 33.67503911421598417 ) ) ;
#51655 = CARTESIAN_POINT ( 'NONE',  ( 19.57500000122903216, 2.886751345948129099, -4.999999999999998224 ) ) ;
#51656 = CARTESIAN_POINT ( 'NONE',  ( 14.61562500061451608, -6.054752690667223547, -1.112240025338166033E-15 ) ) ;
#51657 = CARTESIAN_POINT ( 'NONE',  ( 25.31249999999999645, 2.886751345948112668, -5.000000000000024869 ) ) ;
#51658 = ORIENTED_EDGE ( 'NONE', *, *, #37910, .T. ) ;
#51659 = ORIENTED_EDGE ( 'NONE', *, *, #25362, .F. ) ;
#51660 = CARTESIAN_POINT ( 'NONE',  ( 18.75000000000000000, 0.000000000000000000, 4.999999999999998224 ) ) ;
#51661 = DIRECTION ( 'NONE',  ( 0.000000000000000000, 0.000000000000000000, -1.000000000000000000 ) ) ;
#51662 = CARTESIAN_POINT ( 'NONE',  ( 3.253125000614518036, 0.000000000000000000, 5.243569643749999010 ) ) ;
#51663 = CARTESIAN_POINT ( 'NONE',  ( 15.26250000122903216, 0.000000000000000000, 4.999999999999998224 ) ) ;
#51664 = CARTESIAN_POINT ( 'NONE',  ( 20.91562500061451502, -6.054752690667223547, -1.112240025338166033E-15 ) ) ;
#51665 = CARTESIAN_POINT ( 'NONE',  ( 22.30312500061451431, -4.541064518000417216, -2.621784821875001281 ) ) ;
#51666 = CARTESIAN_POINT ( 'NONE',  ( 3.478125000614517237, 6.421520780324663323E-16, -5.243569643749999010 ) ) ;
#51667 = CARTESIAN_POINT ( 'NONE',  ( 28.64999999999999858, 0.000000000000000000, 4.999999999999998224 ) ) ;
#51668 = DIRECTION ( 'NONE',  ( 0.000000000000000000, 0.000000000000000000, -1.000000000000000000 ) ) ;
#51669 = CARTESIAN_POINT ( 'NONE',  ( 8.184375000614515727, 4.119189519843966529, 2.378215178124999607 ) ) ;
#51670 = CARTESIAN_POINT ( 'NONE',  ( 29.37187500061451928, 3.027376345333611329, 5.243569643749999010 ) ) ;
#51671 = CARTESIAN_POINT ( 'NONE',  ( -2.828200636599751609E-16, 12.35000000122903430, -34.61880215351700230 ) ) ;
#51672 = CARTESIAN_POINT ( 'NONE',  ( 4.243569643749999898, 15.13437500061451679, -30.00000000000000000 ) ) ;
#51673 = CARTESIAN_POINT ( 'NONE',  ( 5.137500001229033941, 6.123233995736764310E-16, -4.999999999999998224 ) ) ;
#51674 = CARTESIAN_POINT ( 'NONE',  ( 9.037499999999999645, -2.886751345948125991, -5.000000000000000000 ) ) ;
#51675 =( BOUNDED_CURVE ( )  B_SPLINE_CURVE ( 2, ( #68851, #28961, #57384, #62217, #67765, #62928, #68134, #23407, #45954 ),
 .UNSPECIFIED., .F., .F. ) 
 B_SPLINE_CURVE_WITH_KNOTS ( ( 3, 2, 2, 2, 3 ),
 ( 0.8152173913043478937, 0.8188405797101449002, 0.8260869565217391353, 0.8333333333333333703, 0.8369565217391304879 ),
 .UNSPECIFIED. ) 
 CURVE ( )  GEOMETRIC_REPRESENTATION_ITEM ( )  RATIONAL_B_SPLINE_CURVE ( ( 0.9330127018922192983, 0.9330127018922202975, 1.000000000000000000, 0.8660254037844387076, 1.000000000000000000, 0.8660254037844387076, 1.000000000000000000, 0.9330127018922182991, 0.9330127018922192983 ) ) 
 REPRESENTATION_ITEM ( '' )  );
#51676 = EDGE_CURVE ( 'NONE', #40722, #46244, #30291, .T. ) ;
#51677 = CARTESIAN_POINT ( 'NONE',  ( 4.050000001229035362, -2.886751345948129988, 4.999999999999997335 ) ) ;
#51678 = CARTESIAN_POINT ( 'NONE',  ( 10.39687500061451786, 6.054752690667223547, 3.707466751127219781E-16 ) ) ;
#51679 = CARTESIAN_POINT ( 'NONE',  ( 30.00000000000000000, 6.123233995736764310E-16, -4.999999999999998224 ) ) ;
#51680 = CARTESIAN_POINT ( 'NONE',  ( 3.534375000614518036, 6.421520780324663323E-16, -5.243569643749999010 ) ) ;
#51681 = CARTESIAN_POINT ( 'NONE',  ( -4.757043123249222738, 8.797129135976163639, -33.66161464372975587 ) ) ;
#51682 = CARTESIAN_POINT ( 'NONE',  ( 16.98750000122903359, 4.330127018922191873, 2.499999999999999556 ) ) ;
#51683 = CARTESIAN_POINT ( 'NONE',  ( 6.946875000614517681, -3.027376345333614438, 5.243569643749998122 ) ) ;
#51684 = CARTESIAN_POINT ( 'NONE',  ( 12.53437500061451537, 6.421520780324663323E-16, -5.243569643749999010 ) ) ;
#51685 = CARTESIAN_POINT ( 'NONE',  ( 5.924999999999999822, 6.123233995736764310E-16, -4.999999999999998224 ) ) ;
#51686 = CARTESIAN_POINT ( 'NONE',  ( -4.243569643749999898, 17.55312500061459602, 30.00000000000000000 ) ) ;
#51687 = CARTESIAN_POINT ( 'NONE',  ( 21.94687500061451857, -3.027376345333610441, -5.243569643749999898 ) ) ;
#51688 = CARTESIAN_POINT ( 'NONE',  ( 2.803505685599422037, -4.140118174855662581, 3.024073416196122466 ) ) ;
#51689 = CARTESIAN_POINT ( 'NONE',  ( 25.95000000122903216, 5.773502691896255534, 3.535250795749688894E-16 ) ) ;
#51690 = CARTESIAN_POINT ( 'NONE',  ( 16.80937500061451573, -5.492252693125287522, -1.008910452111647106E-15 ) ) ;
#51691 = CARTESIAN_POINT ( 'NONE',  ( 21.74062500061451431, -3.027376345333614438, 5.243569643749998122 ) ) ;
#51692 = CARTESIAN_POINT ( 'NONE',  ( 12.36562500061451608, -6.054752690667223547, -1.112240025338166033E-15 ) ) ;
#51693 = CARTESIAN_POINT ( 'NONE',  ( 26.52187500061451431, 4.119189519843966529, 2.378215178124999607 ) ) ;
#51694 = CARTESIAN_POINT ( 'NONE',  ( 11.85937500061451644, 0.000000000000000000, 5.243569643749999010 ) ) ;
#51695 = CARTESIAN_POINT ( 'NONE',  ( 27.97500000000000142, 6.123233995736764310E-16, -4.999999999999998224 ) ) ;
#51696 = CARTESIAN_POINT ( 'NONE',  ( 21.63750000122903572, -4.330127018922194537, 2.499999999999995559 ) ) ;
#51697 = CARTESIAN_POINT ( 'NONE',  ( 45.00000000000000000, 0.000000000000000000, 4.999999999999998224 ) ) ;
#51698 = CARTESIAN_POINT ( 'NONE',  ( 13.02187500061451608, 3.027376345333613106, -5.243569643749998122 ) ) ;
#51699 = CARTESIAN_POINT ( 'NONE',  ( 28.09687500061451360, -3.027376345333614438, 5.243569643749998122 ) ) ;
#51700 = CARTESIAN_POINT ( 'NONE',  ( 3.984375000614517326, 6.421520780324663323E-16, -5.243569643749999010 ) ) ;
#51701 = CARTESIAN_POINT ( 'NONE',  ( -3.999999999999999112, 12.31250000000000000, -32.30940107675850470 ) ) ;
#51703 = CARTESIAN_POINT ( 'NONE',  ( 21.60937500061451644, 4.541064518000418104, -2.621784821874998173 ) ) ;
#51702 = VECTOR ( 'NONE', #60290, 1000.000000000000000 ) ;
#51704 = CARTESIAN_POINT ( 'NONE',  ( 14.55937500061451573, 0.000000000000000000, 5.243569643749999010 ) ) ;
#51705 = CARTESIAN_POINT ( 'NONE',  ( -3.756430356250000102, 17.92812499938548498, 30.00000000000000000 ) ) ;
#51706 = CARTESIAN_POINT ( 'NONE',  ( 25.27499999999999858, 6.123233995736764310E-16, -4.999999999999998224 ) ) ;
#51707 = CARTESIAN_POINT ( 'NONE',  ( -3.999999999999999556, 13.13750000000000107, 27.69059892324149175 ) ) ;
#51708 = CARTESIAN_POINT ( 'NONE',  ( 27.42187500061451644, 2.746126346562645981, -4.756430356249997438 ) ) ;
#51709 = CARTESIAN_POINT ( 'NONE',  ( 18.32812500061451644, 6.421520780324663323E-16, -5.243569643749999010 ) ) ;
#51710 = CARTESIAN_POINT ( 'NONE',  ( 7.124999999999999112, -4.330127018922194537, 2.499999999999995559 ) ) ;
#51711 = CARTESIAN_POINT ( 'NONE',  ( 2.803125000614518747, 0.000000000000000000, 5.243569643749999010 ) ) ;
#51712 = CARTESIAN_POINT ( 'NONE',  ( 15.41250000000000142, 2.886751345948129099, -4.999999999999998224 ) ) ;
#51713 = CARTESIAN_POINT ( 'NONE',  ( -4.243569643749997233, 11.29062500061451857, 32.45002607614398471 ) ) ;
#51714 = DIRECTION ( 'NONE',  ( -1.000000000000000000, -0.000000000000000000, -0.000000000000000000 ) ) ;
#51715 = CARTESIAN_POINT ( 'NONE',  ( 26.48437500061451644, 6.421520780324663323E-16, -5.243569643749999010 ) ) ;
#51716 = ORIENTED_EDGE ( 'NONE', *, *, #1232, .T. ) ;
#51717 = CARTESIAN_POINT ( 'NONE',  ( 22.19062500061451715, -3.027376345333614438, 5.243569643749998122 ) ) ;
#51718 = CARTESIAN_POINT ( 'NONE',  ( 19.32187500061451857, 3.027376345333613106, -5.243569643749998122 ) ) ;
#51719 = B_SPLINE_CURVE_WITH_KNOTS ( 'NONE', 3,
 ( #25354, #30894, #24983, #9469 ),
 .UNSPECIFIED., .F., .F.,
 ( 4, 4 ),
 ( 0.001150238639792624086, 0.002170813345905252094 ),
 .UNSPECIFIED. ) ;
#51720 = CARTESIAN_POINT ( 'NONE',  ( 3.262500000000001510, 2.886751345948129099, -4.999999999999998224 ) ) ;
#51721 = CARTESIAN_POINT ( 'NONE',  ( 6.553125000614518747, -4.541064518000417216, -2.621784821875001281 ) ) ;
#51722 = CARTESIAN_POINT ( 'NONE',  ( 22.04062500061451502, 6.054752690667223547, 3.707466751127219781E-16 ) ) ;
#51723 = CARTESIAN_POINT ( 'NONE',  ( 13.17187500061451999, 3.027376345333611329, 5.243569643749999010 ) ) ;
#51724 = CARTESIAN_POINT ( 'NONE',  ( 16.69687500061451502, 6.054752690667223547, 3.707466751127219781E-16 ) ) ;
#51725 = CARTESIAN_POINT ( 'NONE',  ( 4.243569643749999898, 18.19062500061451360, 32.45002607614398471 ) ) ;
#51726 = CARTESIAN_POINT ( 'NONE',  ( 19.38750000122903216, -4.330127018922194537, 2.499999999999995559 ) ) ;
#51727 = CARTESIAN_POINT ( 'NONE',  ( 14.33437500061451786, 5.824947211148865298E-16, -4.756430356249998326 ) ) ;
#51728 = CARTESIAN_POINT ( 'NONE',  ( 9.515625000614518214, 3.027376345333611329, 5.243569643749999010 ) ) ;
#51729 = CARTESIAN_POINT ( 'NONE',  ( 5.671875000614519102, -6.054752690667223547, -1.112240025338166033E-15 ) ) ;
#51730 = CARTESIAN_POINT ( 'NONE',  ( 5.896875000614518747, 6.054752690667223547, 3.707466751127219781E-16 ) ) ;
#51731 = CARTESIAN_POINT ( 'NONE',  ( 24.64687500061451431, -3.027376345333610441, -5.243569643749999898 ) ) ;
#51732 = CARTESIAN_POINT ( 'NONE',  ( 15.89062500061451289, -3.027376345333614438, 5.243569643749998122 ) ) ;
#51733 = CARTESIAN_POINT ( 'NONE',  ( 26.32500000122903216, 2.886751345948129099, -4.999999999999998224 ) ) ;
#51734 = EDGE_CURVE ( 'NONE', #24022, #64545, #23342, .T. ) ;
#51735 = CARTESIAN_POINT ( 'NONE',  ( 26.09062500061451573, 6.054752690667223547, 3.707466751127219781E-16 ) ) ;
#51736 = CARTESIAN_POINT ( 'NONE',  ( 22.62187500061451573, 3.027376345333611329, 5.243569643749999010 ) ) ;
#51737 = CARTESIAN_POINT ( 'NONE',  ( 18.32812500061451644, 6.421520780324663323E-16, -5.243569643749999010 ) ) ;
#51738 = CARTESIAN_POINT ( 'NONE',  ( 4.243569643749999898, 17.83437500061451786, 30.00000000000000000 ) ) ;
#51739 = EDGE_CURVE ( 'NONE', #70443, #40553, #3069, .T. ) ;
#51740 = CARTESIAN_POINT ( 'NONE',  ( 21.36562500061451431, -6.054752690667223547, -1.112240025338166033E-15 ) ) ;
#51741 = CARTESIAN_POINT ( 'NONE',  ( 2.737500001229034474, -4.330127018922194537, 2.499999999999995559 ) ) ;
#51742 = ORIENTED_EDGE ( 'NONE', *, *, #55968, .F. ) ;
#51743 = CARTESIAN_POINT ( 'NONE',  ( 25.76249999999999929, 2.886751345948129099, -4.999999999999998224 ) ) ;
#51744 = CARTESIAN_POINT ( 'NONE',  ( 3.999999999999999112, 13.47500000000000142, -30.00000000000000000 ) ) ;
#51745 = CARTESIAN_POINT ( 'NONE',  ( 1.071796769724493892, 18.17990381179669868, 26.00000000000000711 ) ) ;
#51746 = CARTESIAN_POINT ( 'NONE',  ( 28.22812500061451502, 6.421520780324663323E-16, -5.243569643749999010 ) ) ;
#51747 = CARTESIAN_POINT ( 'NONE',  ( 9.065625000614517148, 3.027376345333611329, 5.243569643749999010 ) ) ;
#51748 = CARTESIAN_POINT ( 'NONE',  ( 22.87500000122903288, 2.886751345948126879, 4.999999999999999112 ) ) ;
#51749 = CARTESIAN_POINT ( 'NONE',  ( 27.96562500061451928, 3.027376345333611329, 5.243569643749999010 ) ) ;
#51750 = CARTESIAN_POINT ( 'NONE',  ( 27.56250000000000000, 2.886751345948129099, -4.999999999999998224 ) ) ;
#51751 = CARTESIAN_POINT ( 'NONE',  ( 3.999999999999999112, 18.08750000122903501, -30.00000000000000000 ) ) ;
#51752 = EDGE_CURVE ( 'NONE', #29206, #72969, #29563, .T. ) ;
#51753 = CARTESIAN_POINT ( 'NONE',  ( -3.999999999999999112, 12.42500000122903536, 27.69059892324149885 ) ) ;
#51754 = CARTESIAN_POINT ( 'NONE',  ( 11.35312500061451679, 0.000000000000000000, 5.243569643749999010 ) ) ;
#51755 = VERTEX_POINT ( 'NONE', #47282 ) ;
#51756 = CARTESIAN_POINT ( 'NONE',  ( 26.50312500061451360, 4.541064518000418104, -2.621784821874998173 ) ) ;
#51757 = CARTESIAN_POINT ( 'NONE',  ( 8.803125000614517859, -4.541064518000417216, -2.621784821875001281 ) ) ;
#51758 = CARTESIAN_POINT ( 'NONE',  ( 5.428125000614517859, 4.541064518000418104, 2.621784821874999949 ) ) ;
#51759 = CARTESIAN_POINT ( 'NONE',  ( 16.39687500061451786, -2.746126346562646425, 4.756430356249996549 ) ) ;
#51760 = EDGE_CURVE ( 'NONE', #3193, #18895, #58344, .T. ) ;
#51761 = DIRECTION ( 'NONE',  ( -0.000000000000000000, -1.000000000000000000, -0.000000000000000000 ) ) ;
#51762 = CARTESIAN_POINT ( 'NONE',  ( 14.36249999999999893, -5.773502691896255534, -1.060575238724906372E-15 ) ) ;
#51763 = CARTESIAN_POINT ( 'NONE',  ( 15.23437500061451644, 6.421520780324663323E-16, -5.243569643749999010 ) ) ;
#51764 = CARTESIAN_POINT ( 'NONE',  ( 11.28750000122903252, -4.330127018922194537, 2.499999999999995559 ) ) ;
#51765 = CARTESIAN_POINT ( 'NONE',  ( 16.47187500061452070, -6.054752690667223547, -1.112240025338166033E-15 ) ) ;
#51766 = CARTESIAN_POINT ( 'NONE',  ( 17.06250000000000000, -5.773502691896255534, -1.060575238724906372E-15 ) ) ;
#51767 = CARTESIAN_POINT ( 'NONE',  ( 20.29687500061451644, 6.054752690667223547, 3.707466751127219781E-16 ) ) ;
#51768 = CARTESIAN_POINT ( 'NONE',  ( 9.001249775931846008E-16, 13.16562500061451857, -25.09994784771203058 ) ) ;
#51769 = CARTESIAN_POINT ( 'NONE',  ( 21.07500000122903572, 2.886751345948126879, 4.999999999999998224 ) ) ;
#51770 = CARTESIAN_POINT ( 'NONE',  ( 23.29687500061451644, 4.119189519843966529, -2.378215178124998275 ) ) ;
#51771 = CARTESIAN_POINT ( 'NONE',  ( -5.810221930991193690E-16, 14.93750000000000000, -34.00000000000000000 ) ) ;
#51772 = CARTESIAN_POINT ( 'NONE',  ( 23.80312500061451786, 4.541064518000418104, -2.621784821874998173 ) ) ;
#51773 = CARTESIAN_POINT ( 'NONE',  ( 29.52187500061451431, -6.054752690667223547, -1.112240025338166033E-15 ) ) ;
#51774 = CARTESIAN_POINT ( 'NONE',  ( 25.46249999999999858, 2.886751345948126879, 4.999999999999999112 ) ) ;
#51775 = CARTESIAN_POINT ( 'NONE',  ( 7.340625000614518392, -3.027376345333614438, 5.243569643749998122 ) ) ;
#51776 = CARTESIAN_POINT ( 'NONE',  ( 25.92187500061451644, 5.824947211148865298E-16, -4.756430356249998326 ) ) ;
#51777 = CARTESIAN_POINT ( 'NONE',  ( 19.65937500061451360, -4.541064518000417216, -2.621784821875001281 ) ) ;
#51778 = CARTESIAN_POINT ( 'NONE',  ( 10.43437500061451395, -2.746126346562646425, 4.756430356249996549 ) ) ;
#51779 = CARTESIAN_POINT ( 'NONE',  ( 6.028125000614517504, -4.541064518000419881, 2.621784821874995952 ) ) ;
#51780 = CARTESIAN_POINT ( 'NONE',  ( 8.334375000614516082, -4.541064518000419881, 2.621784821874995952 ) ) ;
#51781 = VERTEX_POINT ( 'NONE', #23651 ) ;
#51782 = CARTESIAN_POINT ( 'NONE',  ( 19.54687500061451644, -3.027376345333614438, 5.243569643749998122 ) ) ;
#51783 = FACE_OUTER_BOUND ( 'NONE', #25334, .T. ) ;
#51784 = CARTESIAN_POINT ( 'NONE',  ( 25.83749999999999858, 5.773502691896255534, 3.535250795749688894E-16 ) ) ;
#51785 = CARTESIAN_POINT ( 'NONE',  ( 29.82187500061451502, 3.027376345333611329, 5.243569643749999010 ) ) ;
#51786 = DIRECTION ( 'NONE',  ( 1.000000000000000000, -0.000000000000000000, -0.000000000000000000 ) ) ;
#51787 = ORIENTED_EDGE ( 'NONE', *, *, #34726, .F. ) ;
#51788 = CARTESIAN_POINT ( 'NONE',  ( 10.76250000000000107, -5.773502691896255534, -1.060575238724906372E-15 ) ) ;
#51789 = CARTESIAN_POINT ( 'NONE',  ( 11.89687500061451608, -4.119189519843965641, -2.378215178125001383 ) ) ;
#51790 = CARTESIAN_POINT ( 'NONE',  ( 24.96562500061451573, -6.054752690667223547, -1.112240025338166033E-15 ) ) ;
#51791 = CARTESIAN_POINT ( 'NONE',  ( 13.42499999999999893, -4.330127018922194537, 2.499999999999995559 ) ) ;
#51792 = CARTESIAN_POINT ( 'NONE',  ( 10.72500000122903252, 2.886751345948126879, 4.999999999999999112 ) ) ;
#51793 = CARTESIAN_POINT ( 'NONE',  ( 9.890625000614516438, 6.054752690667223547, 3.707466751127219781E-16 ) ) ;
#51794 = CARTESIAN_POINT ( 'NONE',  ( 24.41250000000000142, 2.886751345948129099, -4.999999999999998224 ) ) ;
#51795 = CARTESIAN_POINT ( 'NONE',  ( 20.57812500061451644, 6.421520780324663323E-16, -5.243569643749999010 ) ) ;
#51796 = CYLINDRICAL_SURFACE ( 'NONE', #20614, 9.000000000000000000 ) ;
#51797 = CARTESIAN_POINT ( 'NONE',  ( 24.86250000122903359, -4.330127018922190985, -2.500000000000001332 ) ) ;
#51798 = CARTESIAN_POINT ( 'NONE',  ( 1.878215178124997609, 17.06562499938548072, 33.25316411605952993 ) ) ;
#51799 = CARTESIAN_POINT ( 'NONE',  ( 6.375000000000001776, 6.123233995736764310E-16, -4.999999999999998224 ) ) ;
#51800 = ORIENTED_EDGE ( 'NONE', *, *, #50590, .F. ) ;
#51801 = CARTESIAN_POINT ( 'NONE',  ( 22.67812500061451431, -4.541064518000419881, 2.621784821874995952 ) ) ;
#51802 = CARTESIAN_POINT ( 'NONE',  ( 28.45312500061451289, 0.000000000000000000, 5.243569643749999010 ) ) ;
#51803 = CARTESIAN_POINT ( 'NONE',  ( 27.00937500061451857, 4.541064518000418104, -2.621784821874998173 ) ) ;
#51804 = CARTESIAN_POINT ( 'NONE',  ( 18.72187500061451360, -6.054752690667223547, -1.112240025338166033E-15 ) ) ;
#51805 = CARTESIAN_POINT ( 'NONE',  ( 14.05312500061451431, 0.000000000000000000, 5.243569643749999010 ) ) ;
#51806 = DIRECTION ( 'NONE',  ( -1.000000000000000000, -0.000000000000000000, -0.000000000000000000 ) ) ;
#51807 = CARTESIAN_POINT ( 'NONE',  ( 25.20000000122903216, -2.886751345948129988, 4.999999999999997335 ) ) ;
#51808 = CARTESIAN_POINT ( 'NONE',  ( 22.99687500061452283, 5.492252693125287522, 3.363034840372157021E-16 ) ) ;
#51809 = CARTESIAN_POINT ( 'NONE',  ( 15.77812500061451573, 4.541064518000418104, 2.621784821874999949 ) ) ;
#51810 = CARTESIAN_POINT ( 'NONE',  ( 24.91875000122902861, 2.886751345948101122, -5.000000000000046185 ) ) ;
#51811 = CARTESIAN_POINT ( 'NONE',  ( 2.775000001229033675, -5.773502691896255534, -1.060575238724906372E-15 ) ) ;
#51812 = CARTESIAN_POINT ( 'NONE',  ( 11.82187500061451679, 3.027376345333611329, 5.243569643749999010 ) ) ;
#51813 = CARTESIAN_POINT ( 'NONE',  ( 11.89687500061451608, -3.027376345333614438, 5.243569643749998122 ) ) ;
#51814 = CARTESIAN_POINT ( 'NONE',  ( 19.47187500061451360, 3.027376345333611329, 5.243569643749999010 ) ) ;
#51815 = VERTEX_POINT ( 'NONE', #18094 ) ;
#51816 = CARTESIAN_POINT ( 'NONE',  ( 9.899999999999998579, -4.330127018922190985, -2.500000000000001332 ) ) ;
#51817 = CARTESIAN_POINT ( 'NONE',  ( 25.22812500061451502, 4.541064518000418104, 2.621784821874999949 ) ) ;
#51818 = CARTESIAN_POINT ( 'NONE',  ( 19.20937500061451786, -4.541064518000417216, -2.621784821875001281 ) ) ;
#51819 = CARTESIAN_POINT ( 'NONE',  ( 24.92812500061451431, -4.541064518000419881, 2.621784821874995952 ) ) ;
#51820 = CARTESIAN_POINT ( 'NONE',  ( -1.071796769724502107, 17.07634618820330275, 26.00000000000000711 ) ) ;
#51821 = CARTESIAN_POINT ( 'NONE',  ( -2.828200636599751609E-16, 14.03750000000000142, 25.38119784648299770 ) ) ;
#51822 = CARTESIAN_POINT ( 'NONE',  ( 28.34062500061451928, 6.054752690667223547, 3.707466751127219781E-16 ) ) ;
#51823 = CARTESIAN_POINT ( 'NONE',  ( 9.750000001229032875, 5.773502691896255534, 3.535250795749688894E-16 ) ) ;
#51824 = CARTESIAN_POINT ( 'NONE',  ( 6.825000001229034829, -5.773502691896255534, -1.060575238724906372E-15 ) ) ;
#51825 = CARTESIAN_POINT ( 'NONE',  ( 28.64999999999999858, 0.000000000000000000, 4.999999999999998224 ) ) ;
#51826 = CARTESIAN_POINT ( 'NONE',  ( 27.33750000122903145, 4.330127018922191873, 2.499999999999999556 ) ) ;
#51827 = CARTESIAN_POINT ( 'NONE',  ( -7.967954043666661671E-16, 13.54062499938548214, 34.33755215474603517 ) ) ;
#51828 = CARTESIAN_POINT ( 'NONE',  ( 16.55625000122903145, 0.000000000000000000, 4.999999999999998224 ) ) ;
#51829 = CARTESIAN_POINT ( 'NONE',  ( 9.609375000614518214, 0.000000000000000000, 5.243569643749999010 ) ) ;
#51830 = DIRECTION ( 'NONE',  ( 0.000000000000000000, 0.000000000000000000, 1.000000000000000000 ) ) ;
#51831 = CARTESIAN_POINT ( 'NONE',  ( 18.17812500061451786, -4.541064518000419881, 2.621784821874995952 ) ) ;
#51832 = CARTESIAN_POINT ( 'NONE',  ( 10.47187500061451715, 3.027376345333611329, 5.243569643749999010 ) ) ;
#51833 = CARTESIAN_POINT ( 'NONE',  ( 3.553125000614516082, 4.541064518000418104, -2.621784821874998173 ) ) ;
#51834 = CARTESIAN_POINT ( 'NONE',  ( 19.28437500061451360, 6.421520780324663323E-16, -5.243569643749999010 ) ) ;
#51835 = CARTESIAN_POINT ( 'NONE',  ( 8.596875000614518925, 6.054752690667223547, 3.707466751127219781E-16 ) ) ;
#51836 = CARTESIAN_POINT ( 'NONE',  ( 14.92500000122903359, -5.773502691896255534, -1.060575238724906372E-15 ) ) ;
#51837 =( BOUNDED_CURVE ( )  B_SPLINE_CURVE ( 2, ( #38118, #26686, #10776, #32585, #33309, #14852, #59915 ),
 .UNSPECIFIED., .F., .F. ) 
 B_SPLINE_CURVE_WITH_KNOTS ( ( 3, 2, 2, 3 ),
 ( 0.8000000000000000444, 0.8027777777777778123, 0.8055555555555555802, 0.8083333333333333481 ),
 .UNSPECIFIED. ) 
 CURVE ( )  GEOMETRIC_REPRESENTATION_ITEM ( )  RATIONAL_B_SPLINE_CURVE ( ( 1.000000000000000000, 0.8660254037844387076, 1.000000000000000000, 0.8660254037844387076, 1.000000000000000000, 0.8660254037844387076, 1.000000000000000000 ) ) 
 REPRESENTATION_ITEM ( '' )  );
#51838 = ADVANCED_FACE ( 'NONE', ( #18462 ), #41382, .F. ) ;
#51839 = CARTESIAN_POINT ( 'NONE',  ( 7.153125000614518392, 4.541064518000418104, -2.621784821874998173 ) ) ;
#51840 = CARTESIAN_POINT ( 'NONE',  ( 16.94062500061451715, -3.027376345333610441, -5.243569643749999898 ) ) ;
#51841 = ORIENTED_EDGE ( 'NONE', *, *, #31751, .T. ) ;
#51842 = CARTESIAN_POINT ( 'NONE',  ( 4.875000001229034652, 2.886751345948126879, 4.999999999999999112 ) ) ;
#51843 = CARTESIAN_POINT ( 'NONE',  ( 15.62812500061451537, 6.421520780324663323E-16, -5.243569643749999010 ) ) ;
#51844 = CARTESIAN_POINT ( 'NONE',  ( 13.94062500061451892, 6.054752690667223547, 3.707466751127219781E-16 ) ) ;
#51845 = CARTESIAN_POINT ( 'NONE',  ( 22.84687500061451715, -2.746126346562642428, -4.756430356249999214 ) ) ;
#51846 = CARTESIAN_POINT ( 'NONE',  ( 12.63749999999999929, -2.886751345948125991, -5.000000000000000000 ) ) ;
#51847 = CARTESIAN_POINT ( 'NONE',  ( 8.662500001229034297, -4.330127018922190985, -2.500000000000001332 ) ) ;
#51848 = CARTESIAN_POINT ( 'NONE',  ( 4.565625000614516260, 3.027376345333611329, 5.243569643749999010 ) ) ;
#51849 = CARTESIAN_POINT ( 'NONE',  ( 19.50000000122903288, -2.886751345948125991, -5.000000000000000000 ) ) ;
#51850 = CARTESIAN_POINT ( 'NONE',  ( 23.92499999999999716, 6.123233995736764310E-16, -4.999999999999998224 ) ) ;
#51851 = CARTESIAN_POINT ( 'NONE',  ( -4.243569643749999898, 12.17187500061451999, -32.45002607614398471 ) ) ;
#51852 = CARTESIAN_POINT ( 'NONE',  ( -4.000000000000000888, 13.21250000000000036, 32.30940107675850470 ) ) ;
#51853 = CARTESIAN_POINT ( 'NONE',  ( 2.850000001229036073, -2.886751345948125991, -5.000000000000000000 ) ) ;
#51854 = EDGE_CURVE ( 'NONE', #65422, #65176, #20967, .T. ) ;
#51855 = CARTESIAN_POINT ( 'NONE',  ( 2.958964567276093582, 4.194048102626701358, -2.735695596862700807 ) ) ;
#51856 = CARTESIAN_POINT ( 'NONE',  ( 24.56249999999999645, 2.886751345948112668, 5.000000000000023981 ) ) ;
#51857 = CARTESIAN_POINT ( 'NONE',  ( 18.75937500061451857, -4.541064518000417216, -2.621784821875001281 ) ) ;
#51858 = CARTESIAN_POINT ( 'NONE',  ( -1.071796769724483234, 16.42009619066137205, 25.99999999999999645 ) ) ;
#51859 = CARTESIAN_POINT ( 'NONE',  ( 14.01562500061451644, 3.027376345333611329, 5.243569643749999010 ) ) ;
#51860 = CARTESIAN_POINT ( 'NONE',  ( 8.531250001229034652, -4.330127018922194537, 2.499999999999995559 ) ) ;
#51861 = CARTESIAN_POINT ( 'NONE',  ( 18.63750000122903216, 6.123233995736764310E-16, -4.999999999999998224 ) ) ;
#51862 = CARTESIAN_POINT ( 'NONE',  ( 25.84687500061451360, -3.027376345333614438, 5.243569643749998122 ) ) ;
#51863 = CARTESIAN_POINT ( 'NONE',  ( 18.04687500061451644, 0.000000000000000000, 4.756430356249998326 ) ) ;
#51864 = CARTESIAN_POINT ( 'NONE',  ( 13.34062500061451750, -3.027376345333610441, -5.243569643749999898 ) ) ;
#51865 = CARTESIAN_POINT ( 'NONE',  ( 15.15937500061451715, -4.541064518000417216, -2.621784821875001281 ) ) ;
#51866 = ORIENTED_EDGE ( 'NONE', *, *, #54850, .F. ) ;
#51867 = CARTESIAN_POINT ( 'NONE',  ( 28.34062500061451928, 6.054752690667223547, 3.707466751127219781E-16 ) ) ;
#51868 = CARTESIAN_POINT ( 'NONE',  ( 20.16562500061451146, 3.027376345333613106, -5.243569643749998122 ) ) ;
#51869 = CARTESIAN_POINT ( 'NONE',  ( 18.82500000000000284, -4.330127018922194537, 2.499999999999995559 ) ) ;
#51870 = CARTESIAN_POINT ( 'NONE',  ( 30.00000000000000000, 6.123233995736764310E-16, -4.999999999999998224 ) ) ;
#51871 = ADVANCED_FACE ( 'NONE', ( #9220 ), #8482, .T. ) ;
#51872 =( BOUNDED_CURVE ( )  B_SPLINE_CURVE ( 2, ( #59191, #14869, #59560, #31130, #36312, #59931, #48132, #31870, #70656 ),
 .UNSPECIFIED., .F., .F. ) 
 B_SPLINE_CURVE_WITH_KNOTS ( ( 3, 2, 2, 2, 3 ),
 ( 0.3750000000000000000, 0.3796296296296296502, 0.3888888888888888951, 0.3981481481481481399, 0.4027777777777777901 ),
 .UNSPECIFIED. ) 
 CURVE ( )  GEOMETRIC_REPRESENTATION_ITEM ( )  RATIONAL_B_SPLINE_CURVE ( ( 0.9330127018922194093, 0.9330127018922194093, 1.000000000000000000, 0.8660254037844387076, 1.000000000000000000, 0.8660254037844387076, 1.000000000000000000, 0.9330127018922189652, 0.9330127018922194093 ) ) 
 REPRESENTATION_ITEM ( '' )  );
#51873 = CARTESIAN_POINT ( 'NONE',  ( 9.674999999999998934, 4.330127018922191873, 2.499999999999999556 ) ) ;
#51874 = CARTESIAN_POINT ( 'NONE',  ( 18.41250000122903430, 0.000000000000000000, 4.999999999999998224 ) ) ;
#51875 = DIRECTION ( 'NONE',  ( 0.000000000000000000, 0.000000000000000000, 1.000000000000000000 ) ) ;
#51876 = CARTESIAN_POINT ( 'NONE',  ( 11.10937500061451821, 2.746126346562645981, -4.756430356249997438 ) ) ;
#51877 = ORIENTED_EDGE ( 'NONE', *, *, #24198, .T. ) ;
#51878 = CARTESIAN_POINT ( 'NONE',  ( 17.92500000000000071, -4.330127018922194537, 2.499999999999995559 ) ) ;
#51879 = CARTESIAN_POINT ( 'NONE',  ( 20.99999999999999645, 0.000000000000000000, 4.999999999999998224 ) ) ;
#51880 =( BOUNDED_CURVE ( )  B_SPLINE_CURVE ( 2, ( #41647, #29115, #24286, #70081, #46834, #63452, #58622 ),
 .UNSPECIFIED., .F., .F. ) 
 B_SPLINE_CURVE_WITH_KNOTS ( ( 3, 2, 2, 3 ),
 ( 0.6700000000000000400, 0.6733333333333333393, 0.6766666666666667496, 0.6800000000000001599 ),
 .UNSPECIFIED. ) 
 CURVE ( )  GEOMETRIC_REPRESENTATION_ITEM ( )  RATIONAL_B_SPLINE_CURVE ( ( 1.000000000000000000, 0.8660254037844387076, 1.000000000000000000, 0.8660254037844387076, 1.000000000000000000, 0.8660254037844342667, 1.000000000000004441 ) ) 
 REPRESENTATION_ITEM ( '' )  );
#51881 = CARTESIAN_POINT ( 'NONE',  ( 19.80937500061451573, 4.541064518000418104, -2.621784821874998173 ) ) ;
#51882 = CARTESIAN_POINT ( 'NONE',  ( 26.12812500061451360, 4.541064518000418104, 2.621784821874999949 ) ) ;
#51883 = ORIENTED_EDGE ( 'NONE', *, *, #2540, .F. ) ;
#51884 = FACE_OUTER_BOUND ( 'NONE', #10595, .T. ) ;
#51885 = CARTESIAN_POINT ( 'NONE',  ( 8.090625000614515727, 6.054752690667223547, 3.707466751127219781E-16 ) ) ;
#51886 = CARTESIAN_POINT ( 'NONE',  ( 0.3499505129295816808, 20.49406157211743462, 34.00000000000000000 ) ) ;
#51887 = CARTESIAN_POINT ( 'NONE',  ( 13.72500000000000142, 4.330127018922191873, 2.499999999999999556 ) ) ;
#51888 = CARTESIAN_POINT ( 'NONE',  ( -4.243569643749999898, 18.45312500061451644, 30.00000000000000000 ) ) ;
#51889 = CARTESIAN_POINT ( 'NONE',  ( 28.94062500061452070, -3.027376345333614438, 5.243569643749998122 ) ) ;
#51890 = CARTESIAN_POINT ( 'NONE',  ( 9.750000000000001776, 0.000000000000000000, 4.999999999999998224 ) ) ;
#51891 = CARTESIAN_POINT ( 'NONE',  ( 1.878215178124997609, 16.16562499938548569, 33.25316411605952993 ) ) ;
#51892 = CARTESIAN_POINT ( 'NONE',  ( 26.85937500061451644, -4.541064518000417216, -2.621784821875001281 ) ) ;
#51893 = ORIENTED_EDGE ( 'NONE', *, *, #66002, .T. ) ;
#51894 = CARTESIAN_POINT ( 'NONE',  ( 20.42812500061451431, -4.541064518000419881, 2.621784821874995952 ) ) ;
#51895 = CARTESIAN_POINT ( 'NONE',  ( 23.55937500061451573, 0.000000000000000000, 5.243569643749999010 ) ) ;
#51896 = CARTESIAN_POINT ( 'NONE',  ( -4.243569643749999898, 16.20312500061459460, -30.00000000000000000 ) ) ;
#51897 = CARTESIAN_POINT ( 'NONE',  ( 10.46249999999999858, 2.886751345948129099, -4.999999999999998224 ) ) ;
#51898 = CARTESIAN_POINT ( 'NONE',  ( 6.778125000614518392, 4.541064518000418104, 2.621784821874999949 ) ) ;
#51899 = CARTESIAN_POINT ( 'NONE',  ( 29.74687500061451573, 5.492252693125287522, 3.363034840372157021E-16 ) ) ;
#51900 = CARTESIAN_POINT ( 'NONE',  ( 23.20312500061451644, -4.541064518000417216, -2.621784821875001281 ) ) ;
#51901 = CARTESIAN_POINT ( 'NONE',  ( 27.38437500061451502, 5.492252693125287522, 3.363034840372157021E-16 ) ) ;
#51902 = CARTESIAN_POINT ( 'NONE',  ( 13.80937500061451750, -4.119189519843965641, -2.378215178125001383 ) ) ;
#51903 = CARTESIAN_POINT ( 'NONE',  ( 18.98437500061451644, 4.541064518000418104, 2.621784821874999949 ) ) ;
#51904 = CARTESIAN_POINT ( 'NONE',  ( -4.243569643749999898, 12.62187500061451928, 27.54997392385601529 ) ) ;
#51905 = CARTESIAN_POINT ( 'NONE',  ( 19.54687500061451644, -3.027376345333614438, 5.243569643749998122 ) ) ;
#51906 = CARTESIAN_POINT ( 'NONE',  ( 26.55937500061451573, 4.541064518000418104, -2.621784821874998173 ) ) ;
#51907 = CARTESIAN_POINT ( 'NONE',  ( 4.243569643749999898, 15.99687500061451573, 32.45002607614398471 ) ) ;
#51908 = CARTESIAN_POINT ( 'NONE',  ( 8.015625000614518214, 3.027376345333613106, -5.243569643749998122 ) ) ;
#51909 = CARTESIAN_POINT ( 'NONE',  ( -1.071796769724490783, 19.19240381056767220, 34.00000000000000000 ) ) ;
#51910 =( BOUNDED_CURVE ( )  B_SPLINE_CURVE ( 2, ( #32716, #72970, #66329, #33801, #44547, #16437, #21988 ),
 .UNSPECIFIED., .F., .F. ) 
 B_SPLINE_CURVE_WITH_KNOTS ( ( 3, 2, 2, 3 ),
 ( 0.3699999999999999956, 0.3733333333333333504, 0.3766666666666666496, 0.3800000000000000044 ),
 .UNSPECIFIED. ) 
 CURVE ( )  GEOMETRIC_REPRESENTATION_ITEM ( )  RATIONAL_B_SPLINE_CURVE ( ( 1.000000000000000000, 0.8660254037844387076, 1.000000000000000000, 0.8660254037844387076, 1.000000000000000000, 0.8660254037844387076, 1.000000000000000000 ) ) 
 REPRESENTATION_ITEM ( '' )  );
#51911 = CARTESIAN_POINT ( 'NONE',  ( 3.421875000614516882, -6.054752690667223547, -1.112240025338166033E-15 ) ) ;
#51912 = CARTESIAN_POINT ( 'NONE',  ( 25.98750000122903003, 4.330127018922191873, 2.499999999999999556 ) ) ;
#51913 = CARTESIAN_POINT ( 'NONE',  ( 6.178125000614518747, 6.421520780324663323E-16, -5.243569643749999010 ) ) ;
#51914 = CARTESIAN_POINT ( 'NONE',  ( 9.834375000614517859, 6.421520780324663323E-16, -5.243569643749999010 ) ) ;
#51915 = SURFACE_STYLE_FILL_AREA ( #19355 ) ;
#51916 = CARTESIAN_POINT ( 'NONE',  ( 15.60000000122903607, 5.773502691896255534, 3.535250795749688894E-16 ) ) ;
#51917 = CARTESIAN_POINT ( 'NONE',  ( 5.221875000614519813, -6.054752690667223547, -1.112240025338166033E-15 ) ) ;
#51918 = CARTESIAN_POINT ( 'NONE',  ( 8.353125000614518569, -4.541064518000417216, -2.621784821875001281 ) ) ;
#51919 = CARTESIAN_POINT ( 'NONE',  ( 4.073549908004127751, -3.793187680347479329, 3.430006214993830405 ) ) ;
#51920 = CARTESIAN_POINT ( 'NONE',  ( 23.15625000122903288, 4.330127018922192761, -2.499999999999997780 ) ) ;
#51921 = CARTESIAN_POINT ( 'NONE',  ( 17.33437500061451431, -4.541064518000419881, 2.621784821874995952 ) ) ;
#51922 = CARTESIAN_POINT ( 'NONE',  ( 1.626862140677534273E-15, 10.66249999999999964, 34.00000000000000000 ) ) ;
#51923 = ORIENTED_EDGE ( 'NONE', *, *, #68367, .T. ) ;
#51924 = CARTESIAN_POINT ( 'NONE',  ( 25.15312500061451217, 4.541064518000418104, -2.621784821874998173 ) ) ;
#51925 = CARTESIAN_POINT ( 'NONE',  ( 9.140625000614518214, -3.027376345333614438, 5.243569643749998122 ) ) ;
#51926 = CARTESIAN_POINT ( 'NONE',  ( 26.89687500061451431, -3.027376345333610441, -5.243569643749999898 ) ) ;
#51927 = CARTESIAN_POINT ( 'NONE',  ( 10.82812500061451644, 4.541064518000418104, 2.621784821874999949 ) ) ;
#51928 = CARTESIAN_POINT ( 'NONE',  ( -4.243569643749998122, 10.89687500061451786, -27.54997392385601174 ) ) ;
#51929 = CARTESIAN_POINT ( 'NONE',  ( 9.787500001229036073, 4.330127018922191873, 2.499999999999999556 ) ) ;
#51930 = CARTESIAN_POINT ( 'NONE',  ( 28.37812500061451715, 4.541064518000418104, 2.621784821874999949 ) ) ;
#51931 = CARTESIAN_POINT ( 'NONE',  ( 4.243569643749999898, 13.72812500061451679, -30.00000000000000000 ) ) ;
#51932 = CARTESIAN_POINT ( 'NONE',  ( 11.96250000122903501, 4.330127018922192761, -2.499999999999997780 ) ) ;
#51933 = CARTESIAN_POINT ( 'NONE',  ( 21.29062500061451502, -3.027376345333614438, 5.243569643749998122 ) ) ;
#51934 = CARTESIAN_POINT ( 'NONE',  ( 10.42500000000000071, 6.123233995736764310E-16, -4.999999999999998224 ) ) ;
#51935 = CARTESIAN_POINT ( 'NONE',  ( 21.51562500061451644, 3.027376345333613106, -5.243569643749998122 ) ) ;
#51936 = CARTESIAN_POINT ( 'NONE',  ( 6.309375000614517504, 4.541064518000418104, -2.621784821874998173 ) ) ;
#51937 = CARTESIAN_POINT ( 'NONE',  ( 20.13749999999999929, -2.886751345948129988, 4.999999999999997335 ) ) ;
#51938 = CARTESIAN_POINT ( 'NONE',  ( 7.012500001229035718, 4.330127018922192761, -2.499999999999997780 ) ) ;
#51939 = CARTESIAN_POINT ( 'NONE',  ( 15.11250000122903359, 4.330127018922192761, -2.499999999999997780 ) ) ;
#51940 = CARTESIAN_POINT ( 'NONE',  ( 13.82812500061451466, 6.421520780324663323E-16, -5.243569643749999010 ) ) ;
#51941 = CARTESIAN_POINT ( 'NONE',  ( 15.70312500061451644, 4.541064518000418104, -2.621784821874998173 ) ) ;
#51942 = CARTESIAN_POINT ( 'NONE',  ( 26.62500000122903288, -5.773502691896255534, -1.060575238724906372E-15 ) ) ;
#51943 = CARTESIAN_POINT ( 'NONE',  ( 19.50000000000000000, 4.330127018922192761, -2.499999999999997780 ) ) ;
#51944 = CARTESIAN_POINT ( 'NONE',  ( 23.29687500061451644, -3.027376345333610441, -5.243569643749999898 ) ) ;
#51945 = CARTESIAN_POINT ( 'NONE',  ( 18.58125000122903003, 6.123233995736764310E-16, -4.999999999999998224 ) ) ;
#51946 = CARTESIAN_POINT ( 'NONE',  ( 9.000000001229034652, -2.886751345948129988, 4.999999999999997335 ) ) ;
#51947 = CARTESIAN_POINT ( 'NONE',  ( 8.409375000614518925, -4.541064518000417216, -2.621784821875001281 ) ) ;
#51948 = CARTESIAN_POINT ( 'NONE',  ( 24.72187500061451360, 3.027376345333613106, -5.243569643749998122 ) ) ;
#51949 = CARTESIAN_POINT ( 'NONE',  ( 23.69999999999999929, 0.000000000000000000, 4.999999999999998224 ) ) ;
#51950 = CARTESIAN_POINT ( 'NONE',  ( 21.59062500061451928, 6.054752690667223547, 3.707466751127219781E-16 ) ) ;
#51951 = CARTESIAN_POINT ( 'NONE',  ( 26.07187500061451857, 3.027376345333613106, -5.243569643749998122 ) ) ;
#51952 = CARTESIAN_POINT ( 'NONE',  ( -1.878215178125001827, 18.00312499938548427, 33.25316411605952283 ) ) ;
#51953 = CARTESIAN_POINT ( 'NONE',  ( 18.03749999999999787, -2.886751345948126435, -5.000000000000000000 ) ) ;
#51954 = CARTESIAN_POINT ( 'NONE',  ( 8.559375000614515727, 4.541064518000418104, -2.621784821874998173 ) ) ;
#51955 = CARTESIAN_POINT ( 'NONE',  ( 18.92812500061451431, 4.541064518000418104, 2.621784821874999949 ) ) ;
#51956 = ORIENTED_EDGE ( 'NONE', *, *, #53564, .T. ) ;
#51957 = CARTESIAN_POINT ( 'NONE',  ( 34.99999999999999289, -2.499999999999999556, 3.499999999999999556 ) ) ;
#51958 = CARTESIAN_POINT ( 'NONE',  ( 27.47812500061451502, 4.541064518000418104, 2.621784821874999949 ) ) ;
#51959 = CARTESIAN_POINT ( 'NONE',  ( 4.884375000614518569, 6.421520780324663323E-16, -5.243569643749999010 ) ) ;
#51960 = CARTESIAN_POINT ( 'NONE',  ( 22.68750000122903288, 6.123233995736764310E-16, -4.999999999999998224 ) ) ;
#51961 = EDGE_CURVE ( 'NONE', #70824, #53784, #36082, .T. ) ;
#51962 = CARTESIAN_POINT ( 'NONE',  ( 11.25000000000000000, -4.330127018922190985, -2.500000000000001332 ) ) ;
#51963 = CARTESIAN_POINT ( 'NONE',  ( 16.53750000000000142, -2.886751345948129988, 4.999999999999997335 ) ) ;
#51964 = CARTESIAN_POINT ( 'NONE',  ( 21.40312500061451573, -4.541064518000417216, -2.621784821875001281 ) ) ;
#51965 = ORIENTED_EDGE ( 'NONE', *, *, #20707, .F. ) ;
#51966 = CARTESIAN_POINT ( 'NONE',  ( 24.00000000000000000, 4.330127018922192761, -2.499999999999997780 ) ) ;
#51967 = CARTESIAN_POINT ( 'NONE',  ( 26.25937500061451857, 0.000000000000000000, 5.243569643749999010 ) ) ;
#51968 = ORIENTED_EDGE ( 'NONE', *, *, #21481, .T. ) ;
#51969 = CARTESIAN_POINT ( 'NONE',  ( 14.35312500061451679, 4.541064518000418104, -2.621784821874998173 ) ) ;
#51970 = CARTESIAN_POINT ( 'NONE',  ( 5.653125000614517504, -4.541064518000417216, -2.621784821875001281 ) ) ;
#51971 = CARTESIAN_POINT ( 'NONE',  ( 18.83437500061451786, 5.492252693125287522, 3.363034840372157021E-16 ) ) ;
#51972 = CARTESIAN_POINT ( 'NONE',  ( 28.60312500061451502, -4.541064518000417216, -2.621784821875001281 ) ) ;
#51973 = CARTESIAN_POINT ( 'NONE',  ( 14.28750000122903430, 4.330127018922191873, 2.499999999999999556 ) ) ;
#51974 = CARTESIAN_POINT ( 'NONE',  ( 20.77500000000000213, 6.123233995736764310E-16, -4.999999999999998224 ) ) ;
#51975 = DIRECTION ( 'NONE',  ( -1.000000000000000000, -0.000000000000000000, -0.000000000000000000 ) ) ;
#51976 = CARTESIAN_POINT ( 'NONE',  ( 4.546875000614517326, 6.054752690667223547, 3.707466751127219781E-16 ) ) ;
#51977 = CARTESIAN_POINT ( 'NONE',  ( 8.971875000614515372, 3.027376345333613106, -5.243569643749998122 ) ) ;
#51978 = CARTESIAN_POINT ( 'NONE',  ( 19.43437500061451928, 4.541064518000418104, 2.621784821874999949 ) ) ;
#51979 = CARTESIAN_POINT ( 'NONE',  ( 10.08750000122903323, 6.123233995736764310E-16, -4.999999999999998224 ) ) ;
#51980 = ORIENTED_EDGE ( 'NONE', *, *, #45339, .T. ) ;
#51981 = CARTESIAN_POINT ( 'NONE',  ( 4.846875000614519813, -3.027376345333610441, -5.243569643749999898 ) ) ;
#51982 = CARTESIAN_POINT ( 'NONE',  ( 4.087500000000001243, -2.886751345948125991, -5.000000000000000000 ) ) ;
#51983 = CARTESIAN_POINT ( 'NONE',  ( 4.471875000614518925, 3.027376345333613106, -5.243569643749998122 ) ) ;
#51984 = CARTESIAN_POINT ( 'NONE',  ( 18.89999999999999858, -4.330127018922190985, -2.500000000000001332 ) ) ;
#51985 = CARTESIAN_POINT ( 'NONE',  ( 15.02812500061451750, -4.541064518000419881, 2.621784821874995952 ) ) ;
#51986 = CARTESIAN_POINT ( 'NONE',  ( 2.828200636599751609E-16, 20.26249999999999929, 25.38119784648299415 ) ) ;
#51987 = CARTESIAN_POINT ( 'NONE',  ( 19.62187500061451573, -5.492252693125287522, -1.008910452111647106E-15 ) ) ;
#51988 = CARTESIAN_POINT ( 'NONE',  ( 9.478125000614515017, 4.541064518000418104, 2.621784821874999949 ) ) ;
#51989 = CARTESIAN_POINT ( 'NONE',  ( 26.85937500061451644, -4.541064518000417216, -2.621784821875001281 ) ) ;
#51990 = CARTESIAN_POINT ( 'NONE',  ( 4.243569643749999898, 18.69687500061451857, 32.45002607614398471 ) ) ;
#51991 = CARTESIAN_POINT ( 'NONE',  ( 26.93437500061451573, 6.421520780324663323E-16, -5.243569643749999010 ) ) ;
#51992 = CARTESIAN_POINT ( 'NONE',  ( 8.362500000000002487, 2.886751345948126879, 4.999999999999999112 ) ) ;
#51993 = CARTESIAN_POINT ( 'NONE',  ( -1.999999999999997113, 12.08750000122903501, 33.46410161513775705 ) ) ;
#51994 = CARTESIAN_POINT ( 'NONE',  ( 15.29062500061451679, 6.054752690667223547, 3.707466751127219781E-16 ) ) ;
#51995 = CARTESIAN_POINT ( 'NONE',  ( 7.275000001229035007, -5.773502691896255534, -1.060575238724906372E-15 ) ) ;
#51996 = CARTESIAN_POINT ( 'NONE',  ( 17.29687500061451999, -3.027376345333614438, 5.243569643749998122 ) ) ;
#51997 = CARTESIAN_POINT ( 'NONE',  ( 11.55937500061451928, -4.541064518000417216, -2.621784821875001281 ) ) ;
#51998 = CARTESIAN_POINT ( 'NONE',  ( -3.027546007007308138, 3.984809627175307067, -32.62591084855416312 ) ) ;
#51999 = ORIENTED_EDGE ( 'NONE', *, *, #11236, .T. ) ;
#52000 = CARTESIAN_POINT ( 'NONE',  ( 12.17812500061451608, 4.541064518000418104, 2.621784821874999949 ) ) ;
#52001 = CARTESIAN_POINT ( 'NONE',  ( 24.71250000122903145, 0.000000000000000000, 4.999999999999998224 ) ) ;
#52002 = CARTESIAN_POINT ( 'NONE',  ( 12.72187500061451537, 3.027376345333611329, 5.243569643749999010 ) ) ;
#52003 = CARTESIAN_POINT ( 'NONE',  ( 2.695452854360172346, 9.631537354464013490, -35.36400652783709830 ) ) ;
#52004 = CARTESIAN_POINT ( 'NONE',  ( 14.27812500061451573, 6.421520780324663323E-16, -5.243569643749999010 ) ) ;
#52005 = CARTESIAN_POINT ( 'NONE',  ( 21.05625000122903145, 0.000000000000000000, 4.999999999999998224 ) ) ;
#52006 = CARTESIAN_POINT ( 'NONE',  ( 24.90937500061451715, 0.000000000000000000, 5.243569643749999010 ) ) ;
#52007 = CARTESIAN_POINT ( 'NONE',  ( 30.00000000000000000, 0.000000000000000000, 0.000000000000000000 ) ) ;
#52008 = EDGE_CURVE ( 'NONE', #7649, #6802, #52992, .T. ) ;
#52009 = CARTESIAN_POINT ( 'NONE',  ( 11.36250000122903536, -4.330127018922190985, -2.500000000000001332 ) ) ;
#52010 = CARTESIAN_POINT ( 'NONE',  ( 8.296875000614518214, -2.746126346562646425, 4.756430356249996549 ) ) ;
#52011 = CARTESIAN_POINT ( 'NONE',  ( 3.185410902401353272, 4.246968961681812260, 3.131173267699055796 ) ) ;
#52012 = CARTESIAN_POINT ( 'NONE',  ( -4.243569643749999898, 18.02187500061451786, -32.45002607614398471 ) ) ;
#52013 = CARTESIAN_POINT ( 'NONE',  ( 17.40937500061451715, -4.541064518000417216, -2.621784821875001281 ) ) ;
#52014 = CARTESIAN_POINT ( 'NONE',  ( 17.51250000122903216, 0.000000000000000000, 4.999999999999998224 ) ) ;
#52015 = ADVANCED_FACE ( 'NONE', ( #19921 ), #66299, .T. ) ;
#52016 = CARTESIAN_POINT ( 'NONE',  ( 15.27187500061451786, 3.027376345333613106, -5.243569643749998122 ) ) ;
#52017 = CARTESIAN_POINT ( 'NONE',  ( -2.121784821874999949, 10.78437500061451715, 26.32496088578401938 ) ) ;
#52018 = CARTESIAN_POINT ( 'NONE',  ( 20.36250000122903359, -4.330127018922190985, -2.500000000000001332 ) ) ;
#52019 = CARTESIAN_POINT ( 'NONE',  ( 14.31562500061451537, 3.027376345333613106, -5.243569643749998122 ) ) ;
#52020 = VERTEX_POINT ( 'NONE', #72477 ) ;
#52021 = VERTEX_POINT ( 'NONE', #61746 ) ;
#52022 = CARTESIAN_POINT ( 'NONE',  ( 17.32499999999999929, 4.330127018922191873, 2.499999999999999556 ) ) ;
#52023 = CARTESIAN_POINT ( 'NONE',  ( 3.515625000614516882, 3.027376345333613106, -5.243569643749998122 ) ) ;
#52024 = CARTESIAN_POINT ( 'NONE',  ( 14.28750000122903430, 4.330127018922191873, 2.499999999999999556 ) ) ;
#52025 = CARTESIAN_POINT ( 'NONE',  ( 26.10937500061451644, 4.541064518000418104, -2.621784821874998173 ) ) ;
#52026 = CARTESIAN_POINT ( 'NONE',  ( 20.42812500061451431, -4.541064518000419881, 2.621784821874995952 ) ) ;
#52027 = CARTESIAN_POINT ( 'NONE',  ( 23.57812500061451289, -4.541064518000419881, 2.621784821874995952 ) ) ;
#52028 = CARTESIAN_POINT ( 'NONE',  ( 4.303125000614516971, -4.541064518000417216, -2.621784821875001281 ) ) ;
#52029 = CARTESIAN_POINT ( 'NONE',  ( 26.47499999999999787, -4.330127018922194537, 2.499999999999995559 ) ) ;
#52030 = CARTESIAN_POINT ( 'NONE',  ( 45.00000000000000000, -7.332543590861129168, -5.218601775200074400 ) ) ;
#52031 = CARTESIAN_POINT ( 'NONE',  ( 8.109375000614518214, 4.119189519843966529, -2.378215178124998275 ) ) ;
#52032 = CARTESIAN_POINT ( 'NONE',  ( 2.000000000000000444, 17.97500000000000142, 26.53589838486224650 ) ) ;
#52033 = CARTESIAN_POINT ( 'NONE',  ( 3.952052806804493112, -3.062959721132712865, -4.228389990733410819 ) ) ;
#52034 = CARTESIAN_POINT ( 'NONE',  ( -4.243569643749999898, 15.80937500061451573, -30.00000000000000000 ) ) ;
#52035 = CARTESIAN_POINT ( 'NONE',  ( 5.437500001229035540, -4.330127018922194537, 2.499999999999995559 ) ) ;
#52036 = CARTESIAN_POINT ( 'NONE',  ( 6.037500000000001421, 5.773502691896255534, 3.535250795749688894E-16 ) ) ;
#52037 = CARTESIAN_POINT ( 'NONE',  ( 5.100000001229034297, -2.886751345948125991, -5.000000000000000000 ) ) ;
#52038 = CARTESIAN_POINT ( 'NONE',  ( 10.69687500061451679, -3.027376345333610441, -5.243569643749999898 ) ) ;
#52039 = CARTESIAN_POINT ( 'NONE',  ( 28.37812500061451715, 4.541064518000418104, 2.621784821874999949 ) ) ;
#52040 = DIRECTION ( 'NONE',  ( 0.000000000000000000, 0.000000000000000000, -1.000000000000000000 ) ) ;
#52041 = CARTESIAN_POINT ( 'NONE',  ( 0.000000000000000000, 10.00000000000000000, -36.00000000000000000 ) ) ;
#52042 = CARTESIAN_POINT ( 'NONE',  ( 9.674999999999998934, 4.330127018922191873, 2.499999999999999556 ) ) ;
#52043 = CARTESIAN_POINT ( 'NONE',  ( 8.896875000614517859, -3.027376345333610441, -5.243569643749999898 ) ) ;
#52044 = CARTESIAN_POINT ( 'NONE',  ( 12.23437500061451821, 4.541064518000418104, 2.621784821874999949 ) ) ;
#52045 = CARTESIAN_POINT ( 'NONE',  ( 6.375000000000001776, 6.123233995736764310E-16, -4.999999999999998224 ) ) ;
#52046 = CARTESIAN_POINT ( 'NONE',  ( 4.243569643749999898, 15.97812500061459495, 30.00000000000000000 ) ) ;
#52047 = CARTESIAN_POINT ( 'NONE',  ( 20.97187500061451715, -6.054752690667223547, -1.112240025338166033E-15 ) ) ;
#52048 = CARTESIAN_POINT ( 'NONE',  ( 3.871071818048498869, 25.03394779433038408, 28.95871227317249463 ) ) ;
#52049 = CARTESIAN_POINT ( 'NONE',  ( 7.387500000000001066, 5.773502691896255534, 3.535250795749688894E-16 ) ) ;
#52050 = CARTESIAN_POINT ( 'NONE',  ( 25.65000000122903145, -2.886751345948129988, 4.999999999999997335 ) ) ;
#52051 = CARTESIAN_POINT ( 'NONE',  ( 16.69687500061451502, 0.000000000000000000, 4.756430356249998326 ) ) ;
#52052 = CARTESIAN_POINT ( 'NONE',  ( 23.24062500061451786, -3.027376345333610441, -5.243569643749999898 ) ) ;
#52053 = CARTESIAN_POINT ( 'NONE',  ( 14.27812500061451573, 6.421520780324663323E-16, -5.243569643749999010 ) ) ;
#52054 = CARTESIAN_POINT ( 'NONE',  ( 27.19687500061451502, -4.119189519843965641, -2.378215178125001383 ) ) ;
#52055 = CARTESIAN_POINT ( 'NONE',  ( 10.88437500061451679, 4.541064518000418104, 2.621784821874999949 ) ) ;
#52056 = CARTESIAN_POINT ( 'NONE',  ( 28.80000000000000071, -4.330127018922190985, -2.500000000000001332 ) ) ;
#52057 = CARTESIAN_POINT ( 'NONE',  ( 22.01250000122903216, 0.000000000000000000, 4.999999999999998224 ) ) ;
#52058 = CARTESIAN_POINT ( 'NONE',  ( 11.43750000122903465, 6.123233995736764310E-16, -4.999999999999998224 ) ) ;
#52059 = CARTESIAN_POINT ( 'NONE',  ( 12.53437500061451537, 6.421520780324663323E-16, -5.243569643749999010 ) ) ;
#52060 = CARTESIAN_POINT ( 'NONE',  ( 28.47187500061451715, 3.027376345333611329, 5.243569643749999010 ) ) ;
#52061 = CARTESIAN_POINT ( 'NONE',  ( 1.071796769724493892, 18.17990381179669868, -34.00000000000000000 ) ) ;
#52062 = CARTESIAN_POINT ( 'NONE',  ( 24.41250000122903430, -4.330127018922190985, -2.500000000000001332 ) ) ;
#52063 = CARTESIAN_POINT ( 'NONE',  ( 21.57187500061451502, 3.027376345333613106, -5.243569643749998122 ) ) ;
#52064 = CARTESIAN_POINT ( 'NONE',  ( 14.67187500061451821, -6.054752690667223547, -1.112240025338166033E-15 ) ) ;
#52065 = CARTESIAN_POINT ( 'NONE',  ( 3.756430356250000102, 17.25312499938548072, 30.00000000000000000 ) ) ;
#52066 = CARTESIAN_POINT ( 'NONE',  ( 25.05000000000000071, 0.000000000000000000, 4.999999999999998224 ) ) ;
#52067 = CARTESIAN_POINT ( 'NONE',  ( -0.6941640578732103384, 20.61426548399373004, 33.93677634907117380 ) ) ;
#52068 = CARTESIAN_POINT ( 'NONE',  ( 27.34687500061451360, -2.746126346562642428, -4.756430356249999214 ) ) ;
#52069 = CARTESIAN_POINT ( 'NONE',  ( 18.06562500061451715, 3.027376345333611329, 5.243569643749999010 ) ) ;
#52070 = CARTESIAN_POINT ( 'NONE',  ( 6.862500000000002487, 2.886751345948129099, -4.999999999999998224 ) ) ;
#52071 = CARTESIAN_POINT ( 'NONE',  ( 18.07499999999999929, 6.123233995736764310E-16, -4.999999999999998224 ) ) ;
#52072 = CARTESIAN_POINT ( 'NONE',  ( 14.96250000000000036, 2.886751345948129099, -4.999999999999998224 ) ) ;
#52073 = CARTESIAN_POINT ( 'NONE',  ( -4.243569643749999898, 11.21562500061451750, 27.54997392385601529 ) ) ;
#52074 = CARTESIAN_POINT ( 'NONE',  ( 12.82500000122903394, 2.886751345948129099, -4.999999999999998224 ) ) ;
#52075 = CARTESIAN_POINT ( 'NONE',  ( 9.393750001229035362, -2.886751345948130876, 4.999999999999996447 ) ) ;
#52076 = CARTESIAN_POINT ( 'NONE',  ( 25.09687500061451715, -3.027376345333610441, -5.243569643749999898 ) ) ;
#52077 = ORIENTED_EDGE ( 'NONE', *, *, #47659, .F. ) ;
#52078 = CARTESIAN_POINT ( 'NONE',  ( 20.57812500061451644, 6.421520780324663323E-16, -5.243569643749999010 ) ) ;
#52079 = CARTESIAN_POINT ( 'NONE',  ( 20.89687500061452141, -3.027376345333614438, 5.243569643749998122 ) ) ;
#52080 = CARTESIAN_POINT ( 'NONE',  ( 3.112500000000000711, -5.773502691896255534, -1.060575238724906372E-15 ) ) ;
#52081 = CARTESIAN_POINT ( 'NONE',  ( 7.003125000614518036, -4.541064518000417216, -2.621784821875001281 ) ) ;
#52082 = CARTESIAN_POINT ( 'NONE',  ( 20.99062500061451431, -3.027376345333610441, -5.243569643749999898 ) ) ;
#52083 = CARTESIAN_POINT ( 'NONE',  ( 12.75937500061451857, 0.000000000000000000, 5.243569643749999010 ) ) ;
#52084 = CARTESIAN_POINT ( 'NONE',  ( 16.88437500061451502, -4.541064518000419881, 2.621784821874995952 ) ) ;
#52085 = CARTESIAN_POINT ( 'NONE',  ( 4.243569643749999010, 16.46562500061451573, 27.54997392385601174 ) ) ;
#52086 = CARTESIAN_POINT ( 'NONE',  ( 17.92500000122903359, 2.886751345948126879, 4.999999999999999112 ) ) ;
#52087 = CARTESIAN_POINT ( 'NONE',  ( 13.99687500061451928, 5.492252693125287522, 3.363034840372157021E-16 ) ) ;
#52088 = CARTESIAN_POINT ( 'NONE',  ( 9.778125000614517504, 6.421520780324663323E-16, -5.243569643749999010 ) ) ;
#52089 = CARTESIAN_POINT ( 'NONE',  ( 3.984375000614517326, 6.421520780324663323E-16, -5.243569643749999010 ) ) ;
#52090 = CARTESIAN_POINT ( 'NONE',  ( 5.709375000614517859, -4.541064518000417216, -2.621784821875001281 ) ) ;
#52091 = CARTESIAN_POINT ( 'NONE',  ( 25.69687500061451502, 6.054752690667223547, 3.707466751127219781E-16 ) ) ;
#52092 = CARTESIAN_POINT ( 'NONE',  ( 17.80312500061451786, -4.541064518000417216, -2.621784821875001281 ) ) ;
#52093 = CARTESIAN_POINT ( 'NONE',  ( 27.52500000122903145, -5.773502691896255534, -1.060575238724906372E-15 ) ) ;
#52094 = EDGE_CURVE ( 'NONE', #15128, #69237, #11149, .T. ) ;
#52095 = CARTESIAN_POINT ( 'NONE',  ( 25.71562500061451573, 3.027376345333611329, 5.243569643749999010 ) ) ;
#52096 = CARTESIAN_POINT ( 'NONE',  ( 21.19687500061451502, 6.054752690667223547, 3.707466751127219781E-16 ) ) ;
#52097 = CARTESIAN_POINT ( 'NONE',  ( 17.91562500061451502, 3.027376345333613106, -5.243569643749998122 ) ) ;
#52098 = CARTESIAN_POINT ( 'NONE',  ( -4.243569643749999898, 16.67187500061451644, 27.54997392385601529 ) ) ;
#52099 = CARTESIAN_POINT ( 'NONE',  ( 21.66562500061451502, 3.027376345333611329, 5.243569643749999010 ) ) ;
#52100 = DIRECTION ( 'NONE',  ( 1.000000000000000000, -0.000000000000000000, -0.000000000000000000 ) ) ;
#52101 = ORIENTED_EDGE ( 'NONE', *, *, #2520, .F. ) ;
#52102 = CARTESIAN_POINT ( 'NONE',  ( 25.61250000000000071, -5.773502691896255534, -1.060575238724906372E-15 ) ) ;
#52103 = CARTESIAN_POINT ( 'NONE',  ( 3.999999999999998668, 13.51250000000000107, -32.30940107675850470 ) ) ;
#52104 = CARTESIAN_POINT ( 'NONE',  ( 1.878215178125000495, 19.57812499938548356, 26.74683588394047007 ) ) ;
#52105 = CARTESIAN_POINT ( 'NONE',  ( 3.046875000614519990, -3.027376345333610441, -5.243569643749999898 ) ) ;
#52106 = CARTESIAN_POINT ( 'NONE',  ( 9.665625000614515017, -6.054752690667223547, -1.112240025338166033E-15 ) ) ;
#52107 = CARTESIAN_POINT ( 'NONE',  ( 22.16250000122903074, -4.330127018922190985, -2.500000000000001332 ) ) ;
#52108 = CARTESIAN_POINT ( 'NONE',  ( 26.57812500061451644, 4.541064518000418104, 2.621784821874999949 ) ) ;
#52110 = CARTESIAN_POINT ( 'NONE',  ( 24.78750000000000497, -2.886751345948125991, -5.000000000000000000 ) ) ;
#52109 = MECHANICAL_DESIGN_GEOMETRIC_PRESENTATION_REPRESENTATION (  '', ( #3706 ), #47508 ) ;
#52111 = CARTESIAN_POINT ( 'NONE',  ( 1.999999999999998668, 15.91250000122903430, -33.46410161513775705 ) ) ;
#52112 = CARTESIAN_POINT ( 'NONE',  ( 29.35312500061451502, 0.000000000000000000, 5.243569643749999010 ) ) ;
#52113 = CARTESIAN_POINT ( 'NONE',  ( 9.590625000614517504, -3.027376345333614438, 5.243569643749998122 ) ) ;
#52114 =( BOUNDED_CURVE ( )  B_SPLINE_CURVE ( 2, ( #34132, #23766, #11614, #902, #63654, #35225, #46319 ),
 .UNSPECIFIED., .F., .F. ) 
 B_SPLINE_CURVE_WITH_KNOTS ( ( 3, 2, 2, 3 ),
 ( 0.2900000000000000355, 0.2933333333333333903, 0.2966666666666666896, 0.2999999999999999889 ),
 .UNSPECIFIED. ) 
 CURVE ( )  GEOMETRIC_REPRESENTATION_ITEM ( )  RATIONAL_B_SPLINE_CURVE ( ( 0.9999999999999977796, 0.8660254037844409281, 1.000000000000000000, 0.8660254037844387076, 1.000000000000000000, 0.8660254037844387076, 1.000000000000000000 ) ) 
 REPRESENTATION_ITEM ( '' )  );
#52115 = ORIENTED_EDGE ( 'NONE', *, *, #4793, .F. ) ;
#52116 = CARTESIAN_POINT ( 'NONE',  ( 25.15312500061451217, 4.541064518000418104, -2.621784821874998173 ) ) ;
#52117 = CARTESIAN_POINT ( 'NONE',  ( 7.378125000614518036, -4.541064518000419881, 2.621784821874995952 ) ) ;
#52118 = UNCERTAINTY_MEASURE_WITH_UNIT (LENGTH_MEASURE( 1.000000000000000082E-05 ), #22740, 'distance_accuracy_value', 'NONE');
#52119 = CARTESIAN_POINT ( 'NONE',  ( 5.540625000614515905, -3.027376345333614438, 5.243569643749998122 ) ) ;
#52120 = CARTESIAN_POINT ( 'NONE',  ( 15.68437500061451573, 5.824947211148865298E-16, -4.756430356249998326 ) ) ;
#52121 = CARTESIAN_POINT ( 'NONE',  ( 4.629056002857023344, -1.889931353889065413, 4.891133006415133266 ) ) ;
#52122 = CARTESIAN_POINT ( 'NONE',  ( 13.19999999999999929, 4.330127018922192761, -2.499999999999997780 ) ) ;
#52123 = CARTESIAN_POINT ( 'NONE',  ( 13.62187500061451750, 3.027376345333611329, 5.243569643749999010 ) ) ;
#52124 = CARTESIAN_POINT ( 'NONE',  ( 11.21250000122903501, 0.000000000000000000, 4.999999999999998224 ) ) ;
#52125 = CARTESIAN_POINT ( 'NONE',  ( 17.25937500061451502, 0.000000000000000000, 5.243569643749999010 ) ) ;
#52126 = CARTESIAN_POINT ( 'NONE',  ( 17.92500000000000071, -4.330127018922194537, 2.499999999999995559 ) ) ;
#52127 = CARTESIAN_POINT ( 'NONE',  ( 8.559375000614515727, 4.541064518000418104, -2.621784821874998173 ) ) ;
#52128 = CARTESIAN_POINT ( 'NONE',  ( -2.121784821874999949, 10.72812500061451679, -33.67503911421598417 ) ) ;
#52129 = CARTESIAN_POINT ( 'NONE',  ( 23.59687500061451360, -4.119189519843965641, -2.378215178125001383 ) ) ;
#52130 = CARTESIAN_POINT ( 'NONE',  ( 26.39999999999999858, 0.000000000000000000, 4.999999999999998224 ) ) ;
#52131 = CARTESIAN_POINT ( 'NONE',  ( 23.76562500061451644, 3.027376345333613106, -5.243569643749998122 ) ) ;
#52132 = FILL_AREA_STYLE ('',( #46228 ) ) ;
#52133 = CARTESIAN_POINT ( 'NONE',  ( 29.07187500061451502, -6.054752690667223547, -1.112240025338166033E-15 ) ) ;
#52134 = CARTESIAN_POINT ( 'NONE',  ( 24.26249999999999929, -5.773502691896255534, -1.060575238724906372E-15 ) ) ;
#52135 = CARTESIAN_POINT ( 'NONE',  ( 6.965625000614518392, -6.054752690667223547, -1.112240025338166033E-15 ) ) ;
#52136 = CARTESIAN_POINT ( 'NONE',  ( 24.53437500061451715, -2.746126346562642428, -4.756430356249999214 ) ) ;
#52137 = CARTESIAN_POINT ( 'NONE',  ( 20.18437500061451573, 6.421520780324663323E-16, -5.243569643749999010 ) ) ;
#52138 = CARTESIAN_POINT ( 'NONE',  ( 10.65937500061451715, 2.746126346562645981, -4.756430356249997438 ) ) ;
#52139 = CARTESIAN_POINT ( 'NONE',  ( 2.990625000614519191, -3.027376345333610441, -5.243569643749999898 ) ) ;
#52140 = CARTESIAN_POINT ( 'NONE',  ( 7.659375000614518036, 4.541064518000418104, -2.621784821874998173 ) ) ;
#52141 = VERTEX_POINT ( 'NONE', #56569 ) ;
#52142 = CARTESIAN_POINT ( 'NONE',  ( 20.03437500061451715, -4.541064518000419881, 2.621784821874995952 ) ) ;
#52143 = CARTESIAN_POINT ( 'NONE',  ( 30.00000000000000000, 0.000000000000000000, 0.000000000000000000 ) ) ;
#52144 = CARTESIAN_POINT ( 'NONE',  ( 27.78749999999999787, -2.886751345948129988, 4.999999999999997335 ) ) ;
#52145 = CARTESIAN_POINT ( 'NONE',  ( 29.44687500061451857, -3.027376345333614438, 5.243569643749998122 ) ) ;
#52146 = CARTESIAN_POINT ( 'NONE',  ( 3.999999999999998668, 10.36250000000000426, -32.30940107675850470 ) ) ;
#52147 = CARTESIAN_POINT ( 'NONE',  ( 3.422429900546629877, -3.645130117820770455, -3.769356580772429410 ) ) ;
#52148 = EDGE_LOOP ( 'NONE', ( #42121, #36006, #36703, #59335 ) ) ;
#52149 = CARTESIAN_POINT ( 'NONE',  ( 9.262499999999999289, 2.886751345948126879, 4.999999999999999112 ) ) ;
#52150 = CARTESIAN_POINT ( 'NONE',  ( 10.62187500061451395, 5.824947211148865298E-16, -4.756430356249998326 ) ) ;
#52151 = CARTESIAN_POINT ( 'NONE',  ( 25.41562500061451146, -6.054752690667223547, -1.112240025338166033E-15 ) ) ;
#52152 = CARTESIAN_POINT ( 'NONE',  ( 13.68750000000000178, 5.773502691896255534, 3.535250795749688894E-16 ) ) ;
#52153 = CARTESIAN_POINT ( 'NONE',  ( 7.987500001229032698, 4.330127018922191873, 2.499999999999999556 ) ) ;
#52154 = CARTESIAN_POINT ( 'NONE',  ( 7.490625000614516082, -3.027376345333610441, -5.243569643749999898 ) ) ;
#52155 = CARTESIAN_POINT ( 'NONE',  ( 22.91249999999999432, -5.773502691896255534, -1.060575238724906372E-15 ) ) ;
#52156 = CARTESIAN_POINT ( 'NONE',  ( 22.04062500061451502, 6.054752690667223547, 3.707466751127219781E-16 ) ) ;
#52157 = DIRECTION ( 'NONE',  ( 0.000000000000000000, 0.000000000000000000, 1.000000000000000000 ) ) ;
#52158 = CIRCLE ( 'NONE', #63957, 1.500000000000000444 ) ;
#52159 = CARTESIAN_POINT ( 'NONE',  ( 26.10000000122903430, -2.886751345948129988, 4.999999999999997335 ) ) ;
#52160 = CARTESIAN_POINT ( 'NONE',  ( 1.878215178125000495, 17.66562499938548214, 26.74683588394047007 ) ) ;
#52161 = CARTESIAN_POINT ( 'NONE',  ( 4.987500000000002487, -2.886751345948125991, -5.000000000000000000 ) ) ;
#52162 = VERTEX_POINT ( 'NONE', #67670 ) ;
#52163 = CARTESIAN_POINT ( 'NONE',  ( 21.25312500061451715, 0.000000000000000000, 5.243569643749999010 ) ) ;
#52164 = CARTESIAN_POINT ( 'NONE',  ( 29.39062500061451289, -3.027376345333614438, 5.243569643749998122 ) ) ;
#52165 = CARTESIAN_POINT ( 'NONE',  ( 28.13437500061451502, -4.541064518000419881, 2.621784821874995952 ) ) ;
#52166 = CARTESIAN_POINT ( 'NONE',  ( 17.97187500061451715, 3.027376345333613106, -5.243569643749998122 ) ) ;
#52167 = EDGE_CURVE ( 'NONE', #55474, #11533, #22940, .T. ) ;
#52168 = CARTESIAN_POINT ( 'NONE',  ( 14.39062500061451821, 6.054752690667223547, 3.707466751127219781E-16 ) ) ;
#52169 = CARTESIAN_POINT ( 'NONE',  ( 29.92500000000000071, 4.330127018922191873, 2.499999999999999556 ) ) ;
#52170 = CARTESIAN_POINT ( 'NONE',  ( 25.80000000122903714, -2.886751345948125991, -5.000000000000000000 ) ) ;
#52171 = CARTESIAN_POINT ( 'NONE',  ( 22.47187500061452070, 2.746126346562645981, -4.756430356249997438 ) ) ;
#52172 = CARTESIAN_POINT ( 'NONE',  ( 16.11562500061451786, 3.027376345333612662, -5.243569643749998122 ) ) ;
#52173 = CARTESIAN_POINT ( 'NONE',  ( 1.071796769724493892, 18.51740381056766793, -34.00000000000000000 ) ) ;
#52174 = CARTESIAN_POINT ( 'NONE',  ( 2.962500001229034119, 4.330127018922192761, -2.499999999999997780 ) ) ;
#52175 = CARTESIAN_POINT ( 'NONE',  ( 12.27187500061451786, 3.027376345333611329, 5.243569643749999010 ) ) ;
#52176 = CARTESIAN_POINT ( 'NONE',  ( 11.29687500061451644, 6.054752690667223547, 3.707466751127219781E-16 ) ) ;
#52177 = CARTESIAN_POINT ( 'NONE',  ( 19.80937500061451573, 4.541064518000418104, -2.621784821874998173 ) ) ;
#52178 = EDGE_LOOP ( 'NONE', ( #23526, #16698, #43704, #45900 ) ) ;
#52179 = CARTESIAN_POINT ( 'NONE',  ( 1.111888759404800586, 4.999999999999998224, 1.111888759404800586 ) ) ;
#52180 = CARTESIAN_POINT ( 'NONE',  ( 25.00312500061451715, -4.541064518000417216, -2.621784821875001281 ) ) ;
#52181 = CARTESIAN_POINT ( 'NONE',  ( 19.65937500061451360, -4.541064518000417216, -2.621784821875001281 ) ) ;
#52182 = CARTESIAN_POINT ( 'NONE',  ( 25.37812500061451715, -4.541064518000419881, 2.621784821874995952 ) ) ;
#52183 = LINE ( 'NONE', #47006, #12041 ) ;
#52184 = CARTESIAN_POINT ( 'NONE',  ( -1.999999999999997113, 15.12500000000000000, 33.46410161513775705 ) ) ;
#52185 = CARTESIAN_POINT ( 'NONE',  ( 29.54062500061451502, -3.027376345333610441, -5.243569643749999898 ) ) ;
#52186 = CARTESIAN_POINT ( 'NONE',  ( 8.850000001229034297, 5.773502691896255534, 3.535250795749688894E-16 ) ) ;
#52187 = CARTESIAN_POINT ( 'NONE',  ( 5.287500001229035185, 4.330127018922191873, 2.499999999999999556 ) ) ;
#52188 = CARTESIAN_POINT ( 'NONE',  ( 21.44999999999999929, 0.000000000000000000, 4.999999999999998224 ) ) ;
#52189 = CARTESIAN_POINT ( 'NONE',  ( 26.88750000122903216, 4.330127018922191873, 2.499999999999999556 ) ) ;
#52190 = CARTESIAN_POINT ( 'NONE',  ( -3.756430356250001434, 13.01562499938548534, 32.16877607737301048 ) ) ;
#52191 = CARTESIAN_POINT ( 'NONE',  ( 8.746875000614515727, -3.027376345333614438, 5.243569643749998122 ) ) ;
#52192 = CYLINDRICAL_SURFACE ( 'NONE', #70294, 4.999999999999998224 ) ;
#52193 = CARTESIAN_POINT ( 'NONE',  ( 17.91562500061451502, 3.027376345333613106, -5.243569643749998122 ) ) ;
#52194 = CARTESIAN_POINT ( 'NONE',  ( 10.24687500061451750, -3.027376345333610441, -5.243569643749999898 ) ) ;
#52195 = CARTESIAN_POINT ( 'NONE',  ( 2.878125000614517592, -4.541064518000419881, 2.621784821874995952 ) ) ;
#52196 = CARTESIAN_POINT ( 'NONE',  ( 18.68437500061451928, -4.541064518000419881, 2.621784821874995952 ) ) ;
#52197 = CARTESIAN_POINT ( 'NONE',  ( 8.184375000614515727, 4.541064518000418104, 2.621784821874999949 ) ) ;
#52198 = CARTESIAN_POINT ( 'NONE',  ( 3.478125000614517237, 6.421520780324663323E-16, -5.243569643749999010 ) ) ;
#52199 = CARTESIAN_POINT ( 'NONE',  ( 7.331250001229031810, 6.123233995736764310E-16, -4.999999999999998224 ) ) ;
#52200 = CARTESIAN_POINT ( 'NONE',  ( 7.340625000614518392, -3.027376345333614438, 5.243569643749998122 ) ) ;
#52201 = CARTESIAN_POINT ( 'NONE',  ( 18.47812500061451857, 4.541064518000418104, 2.621784821874999949 ) ) ;
#52202 = ORIENTED_EDGE ( 'NONE', *, *, #58814, .T. ) ;
#52203 = CARTESIAN_POINT ( 'NONE',  ( 5.325000001229033941, 2.886751345948126879, 4.999999999999999112 ) ) ;
#52204 = CARTESIAN_POINT ( 'NONE',  ( 13.82812500061451466, 6.421520780324663323E-16, -5.243569643749999010 ) ) ;
#52205 = CARTESIAN_POINT ( 'NONE',  ( 12.10312500061451857, 4.541064518000418104, -2.621784821874998173 ) ) ;
#52206 = CARTESIAN_POINT ( 'NONE',  ( 23.74687500061451573, -2.746126346562642428, -4.756430356249999214 ) ) ;
#52207 = CARTESIAN_POINT ( 'NONE',  ( 13.98750000000000249, -2.886751345948125991, -5.000000000000000000 ) ) ;
#52208 = CARTESIAN_POINT ( 'NONE',  ( 5.887500001229034829, -4.330127018922194537, 2.499999999999995559 ) ) ;
#52209 = CARTESIAN_POINT ( 'NONE',  ( 3.103125000614517237, 4.541064518000418104, -2.621784821874998173 ) ) ;
#52210 = CARTESIAN_POINT ( 'NONE',  ( 15.90937500061451892, 0.000000000000000000, 5.243569643749999010 ) ) ;
#52211 = CARTESIAN_POINT ( 'NONE',  ( 19.42500000122903714, -5.773502691896255534, -1.060575238724906372E-15 ) ) ;
#52212 = CARTESIAN_POINT ( 'NONE',  ( 25.72499999999999787, 6.123233995736764310E-16, -4.999999999999998224 ) ) ;
#52213 = CARTESIAN_POINT ( 'NONE',  ( 4.243569643749999898, 17.77812500061451928, -30.00000000000000000 ) ) ;
#52214 = FACE_OUTER_BOUND ( 'NONE', #12613, .T. ) ;
#52215 = CARTESIAN_POINT ( 'NONE',  ( 22.98750000122903003, -4.330127018922194537, 2.499999999999995559 ) ) ;
#52216 = CARTESIAN_POINT ( 'NONE',  ( 3.041778030301053981, 4.165465603166717656, 2.785201938134701738 ) ) ;
#52217 = CARTESIAN_POINT ( 'NONE',  ( 4.465851277537014496, 2.248593419656079284, -4.736966354317482697 ) ) ;
#52218 = CARTESIAN_POINT ( 'NONE',  ( 19.28437500061451360, 6.421520780324663323E-16, -5.243569643749999010 ) ) ;
#52219 = CARTESIAN_POINT ( 'NONE',  ( 10.53750000122903252, 6.123233995736764310E-16, -4.999999999999998224 ) ) ;
#52220 = ADVANCED_FACE ( 'NONE', ( #22229 ), #62832, .T. ) ;
#52221 = CARTESIAN_POINT ( 'NONE',  ( 13.67812500061451786, -4.541064518000419881, 2.621784821874995952 ) ) ;
#52222 = CARTESIAN_POINT ( 'NONE',  ( 8.606250001229033941, -4.330127018922190985, -2.500000000000001332 ) ) ;
#52223 = CYLINDRICAL_SURFACE ( 'NONE', #63663, 4.999999999999998224 ) ;
#52224 = CARTESIAN_POINT ( 'NONE',  ( 25.39687500061451431, -3.027376345333614438, 5.243569643749998122 ) ) ;
#52225 = CARTESIAN_POINT ( 'NONE',  ( 18.23437500061451644, -2.746126346562641984, -4.756430356249999214 ) ) ;
#52226 = CARTESIAN_POINT ( 'NONE',  ( 9.628125000614517148, -4.541064518000419881, 2.621784821874995952 ) ) ;
#52227 = CARTESIAN_POINT ( 'NONE',  ( 15.04687500061451644, -3.027376345333614438, 5.243569643749998122 ) ) ;
#52228 = ORIENTED_EDGE ( 'NONE', *, *, #39715, .T. ) ;
#52229 = CARTESIAN_POINT ( 'NONE',  ( 27.74062500061451431, -3.027376345333610441, -5.243569643749999898 ) ) ;
#52230 = CARTESIAN_POINT ( 'NONE',  ( 19.52812500061451573, -4.541064518000419881, 2.621784821874995952 ) ) ;
#52231 = FACE_OUTER_BOUND ( 'NONE', #54164, .T. ) ;
#52232 = ADVANCED_FACE ( 'NONE', ( #56923 ), #34032, .T. ) ;
#52233 = CARTESIAN_POINT ( 'NONE',  ( -3.999999999999999112, 14.22500000122903430, -32.30940107675850470 ) ) ;
#52234 = CARTESIAN_POINT ( 'NONE',  ( 10.42500000000000071, 6.123233995736764310E-16, -4.999999999999998224 ) ) ;
#52235 = CARTESIAN_POINT ( 'NONE',  ( 19.05000000122903359, -2.886751345948125991, -5.000000000000000000 ) ) ;
#52236 = CARTESIAN_POINT ( 'NONE',  ( 10.17187500061451644, 5.824947211148865298E-16, -4.756430356249998326 ) ) ;
#52237 = ORIENTED_EDGE ( 'NONE', *, *, #46464, .F. ) ;
#52238 = CARTESIAN_POINT ( 'NONE',  ( 18.18750000000000000, 5.773502691896255534, 3.535250795749688894E-16 ) ) ;
#52239 = ADVANCED_FACE ( 'NONE', ( #56220 ), #17038, .F. ) ;
#52240 = CARTESIAN_POINT ( 'NONE',  ( 21.33749999999999858, 5.773502691896255534, 3.535250795749688894E-16 ) ) ;
#52241 = CARTESIAN_POINT ( 'NONE',  ( 19.09687500061451360, -3.027376345333614438, 5.243569643749998122 ) ) ;
#52242 = CARTESIAN_POINT ( 'NONE',  ( 25.34062500061451217, -3.027376345333614438, 5.243569643749998122 ) ) ;
#52243 = ORIENTED_EDGE ( 'NONE', *, *, #35065, .T. ) ;
#52244 = CARTESIAN_POINT ( 'NONE',  ( 8.887500001229033941, 4.330127018922191873, 2.499999999999999556 ) ) ;
#52245 = CARTESIAN_POINT ( 'NONE',  ( 5.540625000614515905, -3.027376345333614438, 5.243569643749998122 ) ) ;
#52246 = CARTESIAN_POINT ( 'NONE',  ( 1.071796769724491893, 15.29509619066137027, 33.99999999999999289 ) ) ;
#52247 = CARTESIAN_POINT ( 'NONE',  ( 13.68750000000000178, 5.773502691896255534, 3.535250795749688894E-16 ) ) ;
#52248 = CARTESIAN_POINT ( 'NONE',  ( 4.243569643749999898, 17.32812500061451644, 30.00000000000000000 ) ) ;
#52249 = CARTESIAN_POINT ( 'NONE',  ( 28.79062500061451502, 6.054752690667223547, 3.707466751127219781E-16 ) ) ;
#52250 = CARTESIAN_POINT ( 'NONE',  ( 10.38750000000000107, -2.886751345948125991, -5.000000000000000000 ) ) ;
#52251 = CARTESIAN_POINT ( 'NONE',  ( 2.655984681222220721E-16, 17.25312499938548072, 25.66244784525396483 ) ) ;
#52252 = CARTESIAN_POINT ( 'NONE',  ( 26.97187500061451360, 3.027376345333613106, -5.243569643749998122 ) ) ;
#52253 = ORIENTED_EDGE ( 'NONE', *, *, #23045, .T. ) ;
#52254 = CARTESIAN_POINT ( 'NONE',  ( 21.85312500061451502, -4.541064518000417216, -2.621784821875001281 ) ) ;
#52255 = CARTESIAN_POINT ( 'NONE',  ( 22.84687500061451715, -3.027376345333610441, -5.243569643749999898 ) ) ;
#52256 = CARTESIAN_POINT ( 'NONE',  ( -4.243569643749999898, 16.65312500061459389, -30.00000000000000000 ) ) ;
#52257 = CARTESIAN_POINT ( 'NONE',  ( 6.553125000614518747, -4.541064518000417216, -2.621784821875001281 ) ) ;
#52258 = DIRECTION ( 'NONE',  ( 0.000000000000000000, 0.000000000000000000, 1.000000000000000000 ) ) ;
#52259 = CARTESIAN_POINT ( 'NONE',  ( 22.75312500061451360, -4.541064518000417216, -2.621784821875001281 ) ) ;
#52260 = CARTESIAN_POINT ( 'NONE',  ( 27.90937500061452070, 2.746126346562643317, 4.756430356249998326 ) ) ;
#52261 = CARTESIAN_POINT ( 'NONE',  ( 12.12187500061451573, 2.746126346562645981, -4.756430356249997438 ) ) ;
#52262 = CARTESIAN_POINT ( 'NONE',  ( 17.33437500061451431, -4.541064518000419881, 2.621784821874995952 ) ) ;
#52263 =( BOUNDED_CURVE ( )  B_SPLINE_CURVE ( 2, ( #72718, #49457, #4758, #4033, #15821, #43552, #55365, #66445, #22101 ),
 .UNSPECIFIED., .F., .F. ) 
 B_SPLINE_CURVE_WITH_KNOTS ( ( 3, 2, 2, 2, 3 ),
 ( 0.2717391304347826497, 0.2753623188405797118, 0.2826086956521738913, 0.2898550724637681264, 0.2934782608695652439 ),
 .UNSPECIFIED. ) 
 CURVE ( )  GEOMETRIC_REPRESENTATION_ITEM ( )  RATIONAL_B_SPLINE_CURVE ( ( 0.9330127018922194093, 0.9330127018922198534, 1.000000000000000000, 0.8660254037844387076, 1.000000000000000000, 0.8660254037844387076, 1.000000000000000000, 0.9330127018922188542, 0.9330127018922194093 ) ) 
 REPRESENTATION_ITEM ( '' )  );
#52264 = CARTESIAN_POINT ( 'NONE',  ( 20.03437500061451715, -4.541064518000419881, 2.621784821874995952 ) ) ;
#52265 = CARTESIAN_POINT ( 'NONE',  ( 27.27187500061451431, -6.054752690667223547, -1.112240025338166033E-15 ) ) ;
#52266 = CARTESIAN_POINT ( 'NONE',  ( -2.121784821874999949, 15.73437500061451644, 26.32496088578401938 ) ) ;
#52267 = CARTESIAN_POINT ( 'NONE',  ( 7.378125000614518036, -4.541064518000419881, 2.621784821874995952 ) ) ;
#52268 = DIRECTION ( 'NONE',  ( 0.000000000000000000, 0.000000000000000000, 1.000000000000000000 ) ) ;
#52269 = CARTESIAN_POINT ( 'NONE',  ( 5.446875000614518569, 6.054752690667223547, 3.707466751127219781E-16 ) ) ;
#52270 = CARTESIAN_POINT ( 'NONE',  ( 26.55000000000000071, -4.330127018922190985, -2.500000000000001332 ) ) ;
#52271 = CARTESIAN_POINT ( 'NONE',  ( 4.490625000614516971, 6.054752690667223547, 3.707466751127219781E-16 ) ) ;
#52272 = CARTESIAN_POINT ( 'NONE',  ( 10.62187500061451928, -6.054752690667223547, -1.112240025338166033E-15 ) ) ;
#52273 = CARTESIAN_POINT ( 'NONE',  ( 16.31250000122903288, -4.330127018922190985, -2.500000000000001332 ) ) ;
#52274 = CARTESIAN_POINT ( 'NONE',  ( 4.621875000614516615, 3.027376345333611329, 5.243569643749999010 ) ) ;
#52275 = CARTESIAN_POINT ( 'NONE',  ( 6.553125000614518747, -4.541064518000417216, -2.621784821875001281 ) ) ;
#52276 = CARTESIAN_POINT ( 'NONE',  ( -8.484601909799255319E-16, 14.58124999877096606, 34.61880215351700940 ) ) ;
#52277 = CARTESIAN_POINT ( 'NONE',  ( 24.35625000122903216, -4.330127018922190985, -2.500000000000001332 ) ) ;
#52278 = CARTESIAN_POINT ( 'NONE',  ( 16.05937500061451573, -4.541064518000417216, -2.621784821875001281 ) ) ;
#52279 = DIRECTION ( 'NONE',  ( 0.000000000000000000, 0.000000000000000000, -1.000000000000000000 ) ) ;
#52280 = VERTEX_POINT ( 'NONE', #12226 ) ;
#52281 = CARTESIAN_POINT ( 'NONE',  ( 24.66562500061451502, 3.027376345333613106, -5.243569643749998122 ) ) ;
#52282 = CARTESIAN_POINT ( 'NONE',  ( 8.615625000614517859, 3.027376345333611329, 5.243569643749999010 ) ) ;
#52283 = EDGE_CURVE ( 'NONE', #60154, #53798, #18580, .T. ) ;
#52284 = CARTESIAN_POINT ( 'NONE',  ( 26.29687500061451644, -3.027376345333614438, 5.243569643749998122 ) ) ;
#52285 = CARTESIAN_POINT ( 'NONE',  ( 9.028125000614517504, 4.541064518000418104, 2.621784821874999949 ) ) ;
#52286 = CARTESIAN_POINT ( 'NONE',  ( 28.98750000000000071, 5.773502691896255534, 3.535250795749688401E-16 ) ) ;
#52287 = CARTESIAN_POINT ( 'NONE',  ( 10.61250000122903536, 4.330127018922192761, -2.499999999999997780 ) ) ;
#52288 = CARTESIAN_POINT ( 'NONE',  ( 26.01562500061451289, 3.027376345333613106, -5.243569643749998122 ) ) ;
#52289 = CARTESIAN_POINT ( 'NONE',  ( -4.243569643749997233, 12.64062500061451999, -27.54997392385601174 ) ) ;
#52290 = CARTESIAN_POINT ( 'NONE',  ( 11.73750000122903181, -4.330127018922194537, 2.499999999999995559 ) ) ;
#52291 = CARTESIAN_POINT ( 'NONE',  ( 22.07812500061451644, 4.541064518000418104, 2.621784821874999949 ) ) ;
#52292 = CARTESIAN_POINT ( 'NONE',  ( 11.58750000000000036, -2.886751345948129988, 4.999999999999997335 ) ) ;
#52293 = CARTESIAN_POINT ( 'NONE',  ( 19.22812500061451502, 6.421520780324663323E-16, -5.243569643749999010 ) ) ;
#52294 = FACE_OUTER_BOUND ( 'NONE', #66412, .T. ) ;
#52295 = CARTESIAN_POINT ( 'NONE',  ( 21.75000000000000000, 4.330127018922192761, -2.499999999999997780 ) ) ;
#52296 = CARTESIAN_POINT ( 'NONE',  ( 14.17500000122903536, 2.886751345948129099, -4.999999999999998224 ) ) ;
#52297 = CARTESIAN_POINT ( 'NONE',  ( 9.403125000614517504, 4.541064518000418104, -2.621784821874998173 ) ) ;
#52298 = CARTESIAN_POINT ( 'NONE',  ( 16.15312500061451573, 4.541064518000418104, -2.621784821874998173 ) ) ;
#52299 = CARTESIAN_POINT ( 'NONE',  ( 26.58750000122903145, -4.330127018922194537, 2.499999999999995559 ) ) ;
#52300 = CARTESIAN_POINT ( 'NONE',  ( 23.07187500061451857, 3.027376345333611329, 5.243569643749999010 ) ) ;
#52301 = CARTESIAN_POINT ( 'NONE',  ( 0.000000000000000000, 4.999999999999998224, 0.000000000000000000 ) ) ;
#52302 = CARTESIAN_POINT ( 'NONE',  ( 6.562500001229032875, 4.330127018922192761, -2.499999999999997780 ) ) ;
#52303 = CARTESIAN_POINT ( 'NONE',  ( 8.071875000614518569, 3.027376345333613106, -5.243569643749998122 ) ) ;
#52304 = CARTESIAN_POINT ( 'NONE',  ( 25.77187500061451075, 3.027376345333611329, 5.243569643749999010 ) ) ;
#52305 =( BOUNDED_CURVE ( )  B_SPLINE_CURVE ( 2, ( #37072, #31540, #54080, #4931, #44466, #21172, #49633 ),
 .UNSPECIFIED., .F., .F. ) 
 B_SPLINE_CURVE_WITH_KNOTS ( ( 3, 2, 2, 3 ),
 ( 0.1699999999999999567, 0.1733333333333332837, 0.1766666666666666108, 0.1799999999999999378 ),
 .UNSPECIFIED. ) 
 CURVE ( )  GEOMETRIC_REPRESENTATION_ITEM ( )  RATIONAL_B_SPLINE_CURVE ( ( 1.000000000000002220, 0.8660254037844364872, 1.000000000000000000, 0.8660254037844387076, 1.000000000000000000, 0.8660254037844409281, 0.9999999999999977796 ) ) 
 REPRESENTATION_ITEM ( '' )  );
#52306 = CARTESIAN_POINT ( 'NONE',  ( 3.121875000614518836, 3.027376345333613106, -5.243569643749998122 ) ) ;
#52307 = CARTESIAN_POINT ( 'NONE',  ( 20.24062500061451431, 6.054752690667223547, 3.707466751127219781E-16 ) ) ;
#52308 = CARTESIAN_POINT ( 'NONE',  ( 26.14687500061451431, 6.054752690667223547, 3.707466751127219781E-16 ) ) ;
#52309 = CARTESIAN_POINT ( 'NONE',  ( -3.756430356249999214, 16.09062499938548285, 27.83122392262697176 ) ) ;
#52310 = CARTESIAN_POINT ( 'NONE',  ( 18.75000000000000000, 0.000000000000000000, 4.999999999999998224 ) ) ;
#52311 = CARTESIAN_POINT ( 'NONE',  ( 7.771875000614516971, 3.027376345333611329, 5.243569643749999010 ) ) ;
#52312 = CARTESIAN_POINT ( 'NONE',  ( 19.75312500061451360, 4.541064518000418104, -2.621784821874998173 ) ) ;
#52313 = ORIENTED_EDGE ( 'NONE', *, *, #31488, .T. ) ;
#52314 = DIRECTION ( 'NONE',  ( 0.000000000000000000, 1.000000000000000000, -0.000000000000000000 ) ) ;
#52315 = CARTESIAN_POINT ( 'NONE',  ( 27.06562500061451004, 3.027376345333611329, 5.243569643749999010 ) ) ;
#52316 = CARTESIAN_POINT ( 'NONE',  ( 4.021875000614516082, 3.027376345333613106, -5.243569643749998122 ) ) ;
#52317 = DIRECTION ( 'NONE',  ( -0.000000000000000000, -1.000000000000000000, -0.000000000000000000 ) ) ;
#52318 = DIRECTION ( 'NONE',  ( 0.000000000000000000, 0.000000000000000000, -1.000000000000000000 ) ) ;
#52319 = CARTESIAN_POINT ( 'NONE',  ( 16.46249999999999503, 2.886751345948126879, 4.999999999999999112 ) ) ;
#52320 = CARTESIAN_POINT ( 'NONE',  ( 20.80312500061451431, 0.000000000000000000, 5.243569643749999010 ) ) ;
#52321 = ORIENTED_EDGE ( 'NONE', *, *, #26600, .F. ) ;
#52322 = CARTESIAN_POINT ( 'NONE',  ( 25.72499999999999787, 6.123233995736764310E-16, -4.999999999999998224 ) ) ;
#52323 = ADVANCED_FACE ( 'NONE', ( #28149 ), #28857, .F. ) ;
#52324 = CARTESIAN_POINT ( 'NONE',  ( 25.73437500061451644, 4.541064518000418104, 2.621784821874999949 ) ) ;
#52325 = EDGE_LOOP ( 'NONE', ( #3634, #6690, #15175, #36773 ) ) ;
#52326 = CARTESIAN_POINT ( 'NONE',  ( 12.51562500061451821, 3.027376345333613106, -5.243569643749998122 ) ) ;
#52327 = CARTESIAN_POINT ( 'NONE',  ( 5.503125000614516260, 0.000000000000000000, 5.243569643749999010 ) ) ;
#52328 = CARTESIAN_POINT ( 'NONE',  ( 18.90937500061451360, 2.746126346562643317, 4.756430356249998326 ) ) ;
#52329 = CARTESIAN_POINT ( 'NONE',  ( 29.46562500061451573, -6.054752690667223547, -1.112240025338166033E-15 ) ) ;
#52330 = CARTESIAN_POINT ( 'NONE',  ( 16.20000000122903216, -2.886751345948129988, 4.999999999999997335 ) ) ;
#52331 = CARTESIAN_POINT ( 'NONE',  ( 20.96250000000000213, 2.886751345948126879, 4.999999999999999112 ) ) ;
#52332 = CARTESIAN_POINT ( 'NONE',  ( 29.02499999999999858, 4.330127018922191873, 2.499999999999999556 ) ) ;
#52333 = CARTESIAN_POINT ( 'NONE',  ( 3.871875000614519280, -6.054752690667223547, -1.112240025338166033E-15 ) ) ;
#52334 = CARTESIAN_POINT ( 'NONE',  ( 9.084375000614517859, 4.541064518000418104, 2.621784821874999949 ) ) ;
#52335 = CARTESIAN_POINT ( 'NONE',  ( 18.75937500061451857, -4.541064518000417216, -2.621784821875001281 ) ) ;
#52336 = CARTESIAN_POINT ( 'NONE',  ( 9.862500001229033586, 0.000000000000000000, 4.999999999999998224 ) ) ;
#52337 = ORIENTED_EDGE ( 'NONE', *, *, #22115, .T. ) ;
#52338 = CARTESIAN_POINT ( 'NONE',  ( 29.54062500061451502, -3.027376345333610441, -5.243569643749999898 ) ) ;
#52339 = CARTESIAN_POINT ( 'NONE',  ( 3.900000000000000799, 0.000000000000000000, 4.999999999999998224 ) ) ;
#52340 = CARTESIAN_POINT ( 'NONE',  ( 4.021875000614516082, 3.027376345333613106, -5.243569643749998122 ) ) ;
#52341 = CARTESIAN_POINT ( 'NONE',  ( 17.88749999999999929, -2.886751345948129988, 4.999999999999997335 ) ) ;
#52342 = CARTESIAN_POINT ( 'NONE',  ( 14.72812500061451679, 6.421520780324663323E-16, -5.243569643749999010 ) ) ;
#52343 = CARTESIAN_POINT ( 'NONE',  ( 3.999999999999998668, 19.21250000000000213, 32.30940107675850470 ) ) ;
#52344 = CARTESIAN_POINT ( 'NONE',  ( 26.96249999999999858, -5.773502691896255534, -1.060575238724906372E-15 ) ) ;
#52345 = CARTESIAN_POINT ( 'NONE',  ( 1.626862140677534273E-15, 13.47500000122903252, 34.00000000000000000 ) ) ;
#52346 = CARTESIAN_POINT ( 'NONE',  ( 19.84687500061451360, 5.492252693125287522, 3.363034840372157021E-16 ) ) ;
#52347 = CARTESIAN_POINT ( 'NONE',  ( 7.115625000614516082, 3.027376345333613106, -5.243569643749998122 ) ) ;
#52348 = CARTESIAN_POINT ( 'NONE',  ( 25.05937500061451573, -4.541064518000417216, -2.621784821875001281 ) ) ;
#52349 = CARTESIAN_POINT ( 'NONE',  ( 19.61250000122903359, 4.330127018922192761, -2.499999999999997780 ) ) ;
#52350 = CARTESIAN_POINT ( 'NONE',  ( 26.37187500061451217, -6.054752690667223547, -1.112240025338166033E-15 ) ) ;
#52351 = CARTESIAN_POINT ( 'NONE',  ( 7.875000000000000000, 4.330127018922191873, 2.499999999999999556 ) ) ;
#52352 = CARTESIAN_POINT ( 'NONE',  ( -3.999999999999999112, 12.46250000122903323, 30.00000000000000000 ) ) ;
#52353 = CARTESIAN_POINT ( 'NONE',  ( 15.25312500061451715, 4.541064518000418104, -2.621784821874998173 ) ) ;
#52354 = CARTESIAN_POINT ( 'NONE',  ( 6.075000001229034829, 2.886751345948129099, -4.999999999999998224 ) ) ;
#52355 = CARTESIAN_POINT ( 'NONE',  ( 16.95937500061451786, -4.541064518000417216, -2.621784821875001281 ) ) ;
#52356 = CARTESIAN_POINT ( 'NONE',  ( 12.90937500061451537, -4.541064518000417216, -2.621784821875001281 ) ) ;
#52357 = CARTESIAN_POINT ( 'NONE',  ( 30.00000000000000000, 0.000000000000000000, 4.999999999999998224 ) ) ;
#52358 = VERTEX_POINT ( 'NONE', #39234 ) ;
#52359 = CARTESIAN_POINT ( 'NONE',  ( 13.30312500061451786, -4.541064518000417216, -2.621784821875001281 ) ) ;
#52360 = CARTESIAN_POINT ( 'NONE',  ( 29.10000000122903074, 5.773502691896255534, 3.535250795749688401E-16 ) ) ;
#52361 = CARTESIAN_POINT ( 'NONE',  ( 23.13750000122903216, 6.123233995736764310E-16, -4.999999999999998224 ) ) ;
#52362 = CARTESIAN_POINT ( 'NONE',  ( 13.20937500061451786, 0.000000000000000000, 5.243569643749999010 ) ) ;
#52363 = CARTESIAN_POINT ( 'NONE',  ( 14.65312500061451573, -4.541064518000417216, -2.621784821875001281 ) ) ;
#52364 = CARTESIAN_POINT ( 'NONE',  ( 30.00000000000000000, 0.000000000000000000, 0.000000000000000000 ) ) ;
#52365 = CARTESIAN_POINT ( 'NONE',  ( 24.49687500061451573, -3.027376345333614438, 5.243569643749998122 ) ) ;
#52366 = CARTESIAN_POINT ( 'NONE',  ( 8.587500000000000355, -2.886751345948181946, -4.999999999999904077 ) ) ;
#52367 = CARTESIAN_POINT ( 'NONE',  ( 11.66250000122903430, 0.000000000000000000, 4.999999999999998224 ) ) ;
#52368 = DIRECTION ( 'NONE',  ( 0.000000000000000000, 0.000000000000000000, 1.000000000000000000 ) ) ;
#52369 = CARTESIAN_POINT ( 'NONE',  ( 45.00000000000000000, -4.500000000000000000, 5.500000000000000888 ) ) ;
#52370 = CARTESIAN_POINT ( 'NONE',  ( 2.121784821874999061, 16.55937500061451573, -33.67503911421598417 ) ) ;
#52371 = CARTESIAN_POINT ( 'NONE',  ( 19.35937500061451644, 4.541064518000418104, -2.621784821874998173 ) ) ;
#52372 = CARTESIAN_POINT ( 'NONE',  ( 17.43750000122903288, 4.330127018922191873, 2.499999999999999556 ) ) ;
#52373 = CARTESIAN_POINT ( 'NONE',  ( 11.55937500061451928, -4.541064518000417216, -2.621784821875001281 ) ) ;
#52374 = CARTESIAN_POINT ( 'NONE',  ( 2.121784821875001281, 19.50312500061451360, -26.32496088578401938 ) ) ;
#52375 = CARTESIAN_POINT ( 'NONE',  ( 19.91250000122903074, -4.330127018922190985, -2.500000000000001332 ) ) ;
#52376 = CARTESIAN_POINT ( 'NONE',  ( 15.74062500061451608, 6.054752690667223547, 3.707466751127219781E-16 ) ) ;
#52377 = ORIENTED_EDGE ( 'NONE', *, *, #62265, .T. ) ;
#52378 = VERTEX_POINT ( 'NONE', #799 ) ;
#52379 = CARTESIAN_POINT ( 'NONE',  ( 17.10000000000000142, -4.330127018922190985, -2.500000000000001332 ) ) ;
#52380 = CARTESIAN_POINT ( 'NONE',  ( 27.33749999999999858, -2.886751345948096681, 5.000000000000054179 ) ) ;
#52381 = CARTESIAN_POINT ( 'NONE',  ( 13.62187500061451750, 3.027376345333611329, 5.243569643749999010 ) ) ;
#52382 = CARTESIAN_POINT ( 'NONE',  ( 7.320879633048903241E-15, 17.30000000122903003, -34.00000000000000000 ) ) ;
#52383 = EDGE_CURVE ( 'NONE', #64110, #63984, #51207, .T. ) ;
#52384 = CARTESIAN_POINT ( 'NONE',  ( 15.78750000122903430, -4.330127018922194537, 2.499999999999995559 ) ) ;
#52385 = CARTESIAN_POINT ( 'NONE',  ( 25.92187500061451999, -6.054752690667223547, -1.112240025338166033E-15 ) ) ;
#52386 = CARTESIAN_POINT ( 'NONE',  ( 19.15312500061451573, -4.541064518000417216, -2.621784821875001281 ) ) ;
#52387 = CARTESIAN_POINT ( 'NONE',  ( 21.92812500061451431, 6.421520780324663323E-16, -5.243569643749999010 ) ) ;
#52388 = CARTESIAN_POINT ( 'NONE',  ( 29.28750000122903074, -4.330127018922194537, 2.499999999999995559 ) ) ;
#52389 = CARTESIAN_POINT ( 'NONE',  ( 28.27499999999999858, -4.330127018922194537, 2.499999999999995559 ) ) ;
#52390 = LINE ( 'NONE', #40956, #46646 ) ;
#52391 = CARTESIAN_POINT ( 'NONE',  ( 10.17187500061451999, -5.492252693125287522, -1.008910452111647106E-15 ) ) ;
#52392 = DIRECTION ( 'NONE',  ( -0.000000000000000000, -1.000000000000000000, -0.000000000000000000 ) ) ;
#52393 = CARTESIAN_POINT ( 'NONE',  ( 45.00000000000000000, 0.000000000000000000, 0.000000000000000000 ) ) ;
#52394 = CARTESIAN_POINT ( 'NONE',  ( 2.121784821875001281, 15.05937500061451928, -26.32496088578401938 ) ) ;
#52395 = CARTESIAN_POINT ( 'NONE',  ( 7.200000001229035718, -2.886751345948129988, 4.999999999999997335 ) ) ;
#52396 = CARTESIAN_POINT ( 'NONE',  ( 7.050000000000000711, 0.000000000000000000, 4.999999999999998224 ) ) ;
#52397 = CARTESIAN_POINT ( 'NONE',  ( 2.812500001229033320, -4.330127018922190985, -2.500000000000001332 ) ) ;
#52398 = CARTESIAN_POINT ( 'NONE',  ( 10.95937500061451964, 0.000000000000000000, 5.243569643749999010 ) ) ;
#52399 = CARTESIAN_POINT ( 'NONE',  ( 29.16562500061451502, 3.027376345333613106, -5.243569643749998122 ) ) ;
#52400 = DIRECTION ( 'NONE',  ( 0.000000000000000000, 0.000000000000000000, -1.000000000000000000 ) ) ;
#52401 = CARTESIAN_POINT ( 'NONE',  ( -3.685099084293383509, 9.302545652542773880, -34.75097178947568466 ) ) ;
#52402 = DIRECTION ( 'NONE',  ( -1.000000000000000000, -0.000000000000000000, -0.000000000000000000 ) ) ;
#52403 = CARTESIAN_POINT ( 'NONE',  ( 7.096875000614517148, -3.027376345333610441, -5.243569643749999898 ) ) ;
#52404 = CARTESIAN_POINT ( 'NONE',  ( 11.37187500061451750, 3.027376345333611329, 5.243569643749999010 ) ) ;
#52405 = CARTESIAN_POINT ( 'NONE',  ( 7.312500000000000000, 2.886751345948129099, -4.999999999999998224 ) ) ;
#52406 = CARTESIAN_POINT ( 'NONE',  ( -4.243569643749999898, 15.75312500061459531, 30.00000000000000000 ) ) ;
#52407 = ADVANCED_FACE ( 'NONE', ( #39959 ), #27422, .T. ) ;
#52408 = CARTESIAN_POINT ( 'NONE',  ( 3.999890280212508475, 25.00002925860763625, 29.73607354501108446 ) ) ;
#52409 = CARTESIAN_POINT ( 'NONE',  ( 5.549999999999998934, 4.330127018922192761, -2.499999999999997780 ) ) ;
#52410 = CARTESIAN_POINT ( 'NONE',  ( 18.30937500061451573, 2.746126346562645981, -4.756430356249997438 ) ) ;
#52411 = CARTESIAN_POINT ( 'NONE',  ( 23.80312500061451786, 4.541064518000418104, -2.621784821874998173 ) ) ;
#52412 = CARTESIAN_POINT ( 'NONE',  ( 13.79062500061451502, -3.027376345333610441, -5.243569643749999898 ) ) ;
#52413 = CARTESIAN_POINT ( 'NONE',  ( 25.24687500061451217, 0.000000000000000000, 4.756430356249998326 ) ) ;
#52414 = CARTESIAN_POINT ( 'NONE',  ( 10.39687500061451786, 6.054752690667223547, 3.707466751127219781E-16 ) ) ;
#52415 = CARTESIAN_POINT ( 'NONE',  ( 27.26249999999999929, 2.886751345948126879, 4.999999999999999112 ) ) ;
#52416 = CARTESIAN_POINT ( 'NONE',  ( 22.95000000122903216, -2.886751345948129988, 4.999999999999997335 ) ) ;
#52417 = VECTOR ( 'NONE', #11752, 1000.000000000000000 ) ;
#52418 = CARTESIAN_POINT ( 'NONE',  ( 11.28750000122903252, -4.330127018922194537, 2.499999999999995559 ) ) ;
#52419 = CARTESIAN_POINT ( 'NONE',  ( 11.52187500061451608, -6.054752690667223547, -1.112240025338166033E-15 ) ) ;
#52420 = CARTESIAN_POINT ( 'NONE',  ( 27.72187500061451715, -6.054752690667223547, -1.112240025338166033E-15 ) ) ;
#52421 = CARTESIAN_POINT ( 'NONE',  ( 3.009375000614516793, -4.541064518000417216, -2.621784821875001281 ) ) ;
#52422 = LINE ( 'NONE', #24337, #45495 ) ;
#52423 = CARTESIAN_POINT ( 'NONE',  ( 21.64687500061451786, 6.054752690667223547, 3.707466751127219781E-16 ) ) ;
#52424 = AXIS2_PLACEMENT_3D ( 'NONE', #25877, #54325, #21777 ) ;
#52425 = CARTESIAN_POINT ( 'NONE',  ( 11.63437500061451857, 6.421520780324663323E-16, -5.243569643749999010 ) ) ;
#52426 = CARTESIAN_POINT ( 'NONE',  ( 1.878215178124997609, 18.97812499938548214, 33.25316411605952993 ) ) ;
#52427 = CARTESIAN_POINT ( 'NONE',  ( 24.71250000000000213, -5.773502691896255534, -1.060575238724906372E-15 ) ) ;
#52428 = CARTESIAN_POINT ( 'NONE',  ( -1.999999999999999112, 13.55000000000000071, 26.53589838486224650 ) ) ;
#52429 = CARTESIAN_POINT ( 'NONE',  ( 4.243569643749999010, 12.02187500061451786, -32.45002607614398471 ) ) ;
#52430 = CARTESIAN_POINT ( 'NONE',  ( 26.78437500061451360, -4.119189519843968306, 2.378215178124996054 ) ) ;
#52431 = CARTESIAN_POINT ( 'NONE',  ( 15.21562500061451750, 3.027376345333613106, -5.243569643749998122 ) ) ;
#52432 = CARTESIAN_POINT ( 'NONE',  ( 4.349999999999999645, 0.000000000000000000, 4.999999999999998224 ) ) ;
#52433 = CARTESIAN_POINT ( 'NONE',  ( 45.00000000000000000, 6.123233995736764310E-16, -4.999999999999998224 ) ) ;
#52434 = CARTESIAN_POINT ( 'NONE',  ( 30.00000000000000000, 0.000000000000000000, 0.000000000000000000 ) ) ;
#52435 = CARTESIAN_POINT ( 'NONE',  ( 13.98750000000000249, -2.886751345948125991, -5.000000000000000000 ) ) ;
#52436 = CARTESIAN_POINT ( 'NONE',  ( -3.000416591977282496E-16, 11.14062500061451644, 25.09994784771203058 ) ) ;
#52437 = CARTESIAN_POINT ( 'NONE',  ( 13.87500000122903465, 2.886751345948126879, 4.999999999999999112 ) ) ;
#52438 = AXIS2_PLACEMENT_3D ( 'NONE', #61581, #10984, #5446 ) ;
#52439 = CARTESIAN_POINT ( 'NONE',  ( 25.65937500061451715, 4.541064518000418104, -2.621784821874998173 ) ) ;
#52440 = ORIENTED_EDGE ( 'NONE', *, *, #63109, .T. ) ;
#52441 = CARTESIAN_POINT ( 'NONE',  ( 20.50312500061451715, -4.541064518000417216, -2.621784821875001281 ) ) ;
#52442 = AXIS2_PLACEMENT_3D ( 'NONE', #14779, #59844, #36223 ) ;
#52443 = CARTESIAN_POINT ( 'NONE',  ( 20.10937500061451289, -4.541064518000417216, -2.621784821875001281 ) ) ;
#52444 = CARTESIAN_POINT ( 'NONE',  ( 4.275000000000001243, 4.330127018922191873, 2.499999999999999556 ) ) ;
#52445 = CARTESIAN_POINT ( 'NONE',  ( 7.303125000614516082, 0.000000000000000000, 5.243569643749999010 ) ) ;
#52446 = CARTESIAN_POINT ( 'NONE',  ( 22.11562500061451786, 3.027376345333611329, 5.243569643749999010 ) ) ;
#52447 = CARTESIAN_POINT ( 'NONE',  ( 17.82187500061451502, -6.054752690667223547, -1.112240025338166033E-15 ) ) ;
#52448 = CARTESIAN_POINT ( 'NONE',  ( -4.243569643749997233, 14.89062500061451644, 32.45002607614398471 ) ) ;
#52449 = CARTESIAN_POINT ( 'NONE',  ( 19.65000000122902790, 5.773502691896255534, 3.535250795749688894E-16 ) ) ;
#52450 = CARTESIAN_POINT ( 'NONE',  ( 13.32187500061451502, -5.492252693125287522, -1.008910452111647106E-15 ) ) ;
#52451 = CARTESIAN_POINT ( 'NONE',  ( 8.390625000614518214, -3.027376345333610441, -5.243569643749999898 ) ) ;
#52452 = CARTESIAN_POINT ( 'NONE',  ( 13.68750000000000000, 5.773502691896255534, 3.535250795749688401E-16 ) ) ;
#52453 = CARTESIAN_POINT ( 'NONE',  ( 28.34062500061451928, 6.054752690667223547, 3.707466751127219781E-16 ) ) ;
#52454 = CARTESIAN_POINT ( 'NONE',  ( 24.60937500061451644, -4.541064518000417216, -2.621784821875001281 ) ) ;
#52455 = CARTESIAN_POINT ( 'NONE',  ( 14.76562500061451821, 3.027376345333613106, -5.243569643749998122 ) ) ;
#52456 = CARTESIAN_POINT ( 'NONE',  ( 24.60000000122903430, 5.773502691896255534, 3.535250795749688894E-16 ) ) ;
#52457 = CARTESIAN_POINT ( 'NONE',  ( 26.46562500061451573, 3.027376345333613106, -5.243569643749998122 ) ) ;
#52458 = CARTESIAN_POINT ( 'NONE',  ( 22.84687500061451715, -3.027376345333610441, -5.243569643749999898 ) ) ;
#52459 = CARTESIAN_POINT ( 'NONE',  ( 15.81562500061451537, 3.027376345333611329, 5.243569643749999010 ) ) ;
#52460 = CARTESIAN_POINT ( 'NONE',  ( 9.001249775931846008E-16, 16.37187500061451573, 34.90005215228797653 ) ) ;
#52461 = CARTESIAN_POINT ( 'NONE',  ( 22.67812500061451431, -4.541064518000419881, 2.621784821874995952 ) ) ;
#52462 = CARTESIAN_POINT ( 'NONE',  ( 29.19375000122903074, -2.886751345948150860, 4.999999999999960920 ) ) ;
#52463 = EDGE_LOOP ( 'NONE', ( #55031, #57181, #58611, #72802 ) ) ;
#52464 = CARTESIAN_POINT ( 'NONE',  ( 26.39999999999999858, 0.000000000000000000, 4.999999999999998224 ) ) ;
#52465 = CARTESIAN_POINT ( 'NONE',  ( 1.999999999999998668, 14.00000000000000178, -33.46410161513775705 ) ) ;
#52466 = CARTESIAN_POINT ( 'NONE',  ( -3.756430356250000102, 19.27812499938548640, 30.00000000000000000 ) ) ;
#52467 = CARTESIAN_POINT ( 'NONE',  ( 28.82812500061451644, 4.541064518000418104, 2.621784821874999949 ) ) ;
#52468 = CARTESIAN_POINT ( 'NONE',  ( 8.128125000614515372, 4.541064518000418104, 2.621784821874999949 ) ) ;
#52469 = CARTESIAN_POINT ( 'NONE',  ( 21.15000000122903145, -2.886751345948129988, 4.999999999999997335 ) ) ;
#52470 = CARTESIAN_POINT ( 'NONE',  ( 26.09062500061451573, 6.054752690667223547, 3.707466751127219781E-16 ) ) ;
#52471 = CARTESIAN_POINT ( 'NONE',  ( 25.83749999999999858, 5.773502691896255534, 3.535250795749688894E-16 ) ) ;
#52472 = CARTESIAN_POINT ( 'NONE',  ( 8.484601909799253346E-16, 15.72500000122903252, -25.38119784648299770 ) ) ;
#52473 = CARTESIAN_POINT ( 'NONE',  ( 25.20000000122902861, -2.886751345948114000, 5.000000000000024869 ) ) ;
#52474 = CARTESIAN_POINT ( 'NONE',  ( 11.39062500061451644, -3.027376345333614438, 5.243569643749998122 ) ) ;
#52475 = VERTEX_POINT ( 'NONE', #6327 ) ;
#52476 = CARTESIAN_POINT ( 'NONE',  ( 25.97812500061451502, 6.421520780324663323E-16, -5.243569643749999010 ) ) ;
#52477 = CARTESIAN_POINT ( 'NONE',  ( 6.890625000614516438, -3.027376345333614438, 5.243569643749998122 ) ) ;
#52478 = CARTESIAN_POINT ( 'NONE',  ( 3.665625000614517681, 3.027376345333611329, 5.243569643749999010 ) ) ;
#52479 = CARTESIAN_POINT ( 'NONE',  ( 16.32187500061451502, 2.746126346562643317, 4.756430356249998326 ) ) ;
#52480 = CARTESIAN_POINT ( 'NONE',  ( 13.08750000000000213, -2.886751345948126435, -5.000000000000000000 ) ) ;
#52481 = CARTESIAN_POINT ( 'NONE',  ( 12.56250000000000178, -5.773502691896255534, -1.060575238724906372E-15 ) ) ;
#52482 = CARTESIAN_POINT ( 'NONE',  ( 12.79687500061451821, -3.027376345333614438, 5.243569643749998122 ) ) ;
#52483 = CARTESIAN_POINT ( 'NONE',  ( 9.375000001229036428, 2.886751345948126879, 4.999999999999999112 ) ) ;
#52484 = CARTESIAN_POINT ( 'NONE',  ( 17.63437500061451502, 4.541064518000418104, 2.621784821874999949 ) ) ;
#52485 = CARTESIAN_POINT ( 'NONE',  ( 17.43750000000000355, -2.886751345948129988, 4.999999999999997335 ) ) ;
#52486 = CARTESIAN_POINT ( 'NONE',  ( 8.109375000614518214, 4.541064518000418104, -2.621784821874998173 ) ) ;
#52487 = CARTESIAN_POINT ( 'NONE',  ( -2.121784821874996840, 10.87812500061451715, -26.32496088578401583 ) ) ;
#52488 = CARTESIAN_POINT ( 'NONE',  ( 2.000000000000001332, 16.55000000000000071, 33.46410161513774995 ) ) ;
#52489 = CARTESIAN_POINT ( 'NONE',  ( 23.22187500061451360, 5.824947211148865298E-16, -4.756430356249998326 ) ) ;
#52490 = CARTESIAN_POINT ( 'NONE',  ( 26.28750000000000142, 5.773502691896255534, 3.535250795749688401E-16 ) ) ;
#52491 = CARTESIAN_POINT ( 'NONE',  ( 24.92812500061451431, -4.541064518000419881, 2.621784821874995952 ) ) ;
#52492 = CARTESIAN_POINT ( 'NONE',  ( 21.33750000122903145, 6.123233995736764310E-16, -4.999999999999998224 ) ) ;
#52493 = CARTESIAN_POINT ( 'NONE',  ( 27.57187500061451857, 3.027376345333611329, 5.243569643749999010 ) ) ;
#52494 = CARTESIAN_POINT ( 'NONE',  ( 22.68750000000000000, 5.773502691896255534, 3.535250795749688894E-16 ) ) ;
#52495 = EDGE_CURVE ( 'NONE', #8533, #72227, #28120, .T. ) ;
#52496 = CARTESIAN_POINT ( 'NONE',  ( 6.515625000614516438, -6.054752690667223547, -1.112240025338166033E-15 ) ) ;
#52497 = CARTESIAN_POINT ( 'NONE',  ( 24.38437500061451502, -2.746126346562646425, 4.756430356249996549 ) ) ;
#52498 = CARTESIAN_POINT ( 'NONE',  ( 15.79687500061451821, 6.054752690667223547, 3.707466751127219781E-16 ) ) ;
#52499 = CARTESIAN_POINT ( 'NONE',  ( 8.446875000614515017, 4.119189519843966529, -2.378215178124998275 ) ) ;
#52500 = CARTESIAN_POINT ( 'NONE',  ( 29.13750000122903216, 4.330127018922191873, 2.499999999999999556 ) ) ;
#52501 = CARTESIAN_POINT ( 'NONE',  ( 8.071875000614518569, 3.027376345333613106, -5.243569643749998122 ) ) ;
#52502 = ORIENTED_EDGE ( 'NONE', *, *, #28533, .F. ) ;
#52503 = CARTESIAN_POINT ( 'NONE',  ( 18.34687500061451715, -3.027376345333610441, -5.243569643749999898 ) ) ;
#52504 = CARTESIAN_POINT ( 'NONE',  ( -3.973417775690189835, 25.00714840155672292, 30.52930962823944938 ) ) ;
#52505 = CARTESIAN_POINT ( 'NONE',  ( 27.07499999999999929, 6.123233995736764310E-16, -4.999999999999998224 ) ) ;
#52506 = CARTESIAN_POINT ( 'NONE',  ( 28.47187500061451715, 3.027376345333611329, 5.243569643749999010 ) ) ;
#52507 = DIRECTION ( 'NONE',  ( -1.000000000000000000, -0.000000000000000000, -0.000000000000000000 ) ) ;
#52508 = CARTESIAN_POINT ( 'NONE',  ( 12.35625000122903394, 4.330127018922192761, -2.499999999999997780 ) ) ;
#52509 = ORIENTED_EDGE ( 'NONE', *, *, #34544, .F. ) ;
#52510 = CARTESIAN_POINT ( 'NONE',  ( 10.16249999999999964, 2.886751345948126879, 4.999999999999999112 ) ) ;
#52511 = CARTESIAN_POINT ( 'NONE',  ( 10.58437500061451608, -2.746126346562642428, -4.756430356249999214 ) ) ;
#52512 = CARTESIAN_POINT ( 'NONE',  ( 25.30312500061451431, 0.000000000000000000, 5.243569643749999010 ) ) ;
#52513 = CARTESIAN_POINT ( 'NONE',  ( 13.72500000000000142, 4.330127018922191873, 2.499999999999999556 ) ) ;
#52514 = ADVANCED_FACE ( 'NONE', ( #40675, #13670 ), #36213, .T. ) ;
#52515 = CARTESIAN_POINT ( 'NONE',  ( 7.387500001229032165, 6.123233995736764310E-16, -4.999999999999998224 ) ) ;
#52516 = CARTESIAN_POINT ( 'NONE',  ( 6.515625000614516438, -6.054752690667223547, -1.112240025338166033E-15 ) ) ;
#52517 = CARTESIAN_POINT ( 'NONE',  ( 21.60000000000000142, -4.330127018922190985, -2.500000000000001332 ) ) ;
#52518 = CARTESIAN_POINT ( 'NONE',  ( 20.76562500061451644, 3.027376345333611329, 5.243569643749999010 ) ) ;
#52519 = CARTESIAN_POINT ( 'NONE',  ( 23.58749999999999858, 5.773502691896255534, 3.535250795749688401E-16 ) ) ;
#52520 = CARTESIAN_POINT ( 'NONE',  ( 24.71250000122903145, 0.000000000000000000, 4.999999999999998224 ) ) ;
#52521 = CARTESIAN_POINT ( 'NONE',  ( -3.756430356250000102, 18.26562499938548356, 30.00000000000000000 ) ) ;
#52522 = CARTESIAN_POINT ( 'NONE',  ( 5.775000000000002132, -4.330127018922194537, 2.499999999999995559 ) ) ;
#52523 = AXIS2_PLACEMENT_3D ( 'NONE', #54186, #41282, #63793 ) ;
#52524 = ORIENTED_EDGE ( 'NONE', *, *, #57647, .T. ) ;
#52525 = CARTESIAN_POINT ( 'NONE',  ( 20.91562500061451502, -6.054752690667223547, -1.112240025338166033E-15 ) ) ;
#52526 = CARTESIAN_POINT ( 'NONE',  ( 27.36562500061451786, 3.027376345333613106, -5.243569643749998122 ) ) ;
#52527 = CARTESIAN_POINT ( 'NONE',  ( 27.12187500061451573, 3.027376345333611329, 5.243569643749999010 ) ) ;
#52528 = CARTESIAN_POINT ( 'NONE',  ( 14.20312500061451644, -4.541064518000417216, -2.621784821875001281 ) ) ;
#52529 = CARTESIAN_POINT ( 'NONE',  ( 45.00000000000000000, 0.000000000000000000, 0.000000000000000000 ) ) ;
#52530 = CARTESIAN_POINT ( 'NONE',  ( 27.03750000122903430, -4.330127018922194537, 2.499999999999995559 ) ) ;
#52531 = CARTESIAN_POINT ( 'NONE',  ( 20.37187500061451573, 2.746126346562643317, 4.756430356249998326 ) ) ;
#52532 = CARTESIAN_POINT ( 'NONE',  ( 17.12812500061451715, 4.541064518000418104, 2.621784821874999949 ) ) ;
#52533 = FACE_OUTER_BOUND ( 'NONE', #6027, .T. ) ;
#52534 = CARTESIAN_POINT ( 'NONE',  ( 11.40937500061451892, 0.000000000000000000, 5.243569643749999010 ) ) ;
#52535 = CARTESIAN_POINT ( 'NONE',  ( 9.046875000614518214, 6.054752690667223547, 3.707466751127219781E-16 ) ) ;
#52536 = CARTESIAN_POINT ( 'NONE',  ( 20.37187500061451573, 3.027376345333611329, 5.243569643749999010 ) ) ;
#52537 = ORIENTED_EDGE ( 'NONE', *, *, #25258, .F. ) ;
#52538 = CARTESIAN_POINT ( 'NONE',  ( -3.685099084293382177, 9.302545652542775656, 25.24902821052430824 ) ) ;
#52539 = CARTESIAN_POINT ( 'NONE',  ( 22.97812500061451857, 4.541064518000418104, 2.621784821874999949 ) ) ;
#52540 =( BOUNDED_CURVE ( )  B_SPLINE_CURVE ( 2, ( #47354, #52173, #71634, #43559, #9570, #13730, #21007, #29635, #69887 ),
 .UNSPECIFIED., .F., .F. ) 
 B_SPLINE_CURVE_WITH_KNOTS ( ( 3, 2, 2, 2, 3 ),
 ( 0.1413043478260869734, 0.1449275362318840632, 0.1521739130434782705, 0.1594202898550724501, 0.1630434782608695676 ),
 .UNSPECIFIED. ) 
 CURVE ( )  GEOMETRIC_REPRESENTATION_ITEM ( )  RATIONAL_B_SPLINE_CURVE ( ( 0.9330127018922194093, 0.9330127018922196314, 1.000000000000000000, 0.8660254037844387076, 1.000000000000000000, 0.8660254037844387076, 1.000000000000000000, 0.9330127018922190762, 0.9330127018922194093 ) ) 
 REPRESENTATION_ITEM ( '' )  );
#52541 = CIRCLE ( 'NONE', #70260, 10.00000000000000000 ) ;
#52542 = CARTESIAN_POINT ( 'NONE',  ( 18.87187500061451573, 3.027376345333613106, -5.243569643749998122 ) ) ;
#52543 = CARTESIAN_POINT ( 'NONE',  ( 23.31562500061451715, 3.027376345333613106, -5.243569643749998122 ) ) ;
#52544 = CARTESIAN_POINT ( 'NONE',  ( 4.000000000000000000, 18.78124999877096357, 27.69059892324149885 ) ) ;
#52545 = CARTESIAN_POINT ( 'NONE',  ( -2.828200636599751609E-16, 14.93750000000000000, 25.38119784648299770 ) ) ;
#52546 = CARTESIAN_POINT ( 'NONE',  ( 28.94062500061452070, -3.027376345333614438, 5.243569643749998122 ) ) ;
#52547 = CARTESIAN_POINT ( 'NONE',  ( 8.700000001229032165, -2.886751345948125991, -5.000000000000000000 ) ) ;
#52548 = AXIS2_PLACEMENT_3D ( 'NONE', #20809, #23354, #68434 ) ;
#52549 = ORIENTED_EDGE ( 'NONE', *, *, #37707, .F. ) ;
#52550 = CARTESIAN_POINT ( 'NONE',  ( 5.362500001229033586, 0.000000000000000000, 4.999999999999998224 ) ) ;
#52551 = CARTESIAN_POINT ( 'NONE',  ( -3.999999999999999556, 19.51250000000000284, -32.30940107675850470 ) ) ;
#52552 = CARTESIAN_POINT ( 'NONE',  ( 25.98750000122903003, 4.330127018922191873, 2.499999999999999556 ) ) ;
#52553 = CARTESIAN_POINT ( 'NONE',  ( 2.828200636599751609E-16, 20.20624999877096784, 25.38119784648299415 ) ) ;
#52554 = CARTESIAN_POINT ( 'NONE',  ( 9.721875000614517148, -6.054752690667223547, -1.112240025338166033E-15 ) ) ;
#52555 = CYLINDRICAL_SURFACE ( 'NONE', #34914, 4.999999999999998224 ) ;
#52556 = CARTESIAN_POINT ( 'NONE',  ( 16.56562500061451715, 3.027376345333613106, -5.243569643749998122 ) ) ;
#52557 = CARTESIAN_POINT ( 'NONE',  ( 11.67187500061451821, 3.027376345333613106, -5.243569643749998122 ) ) ;
#52558 = CARTESIAN_POINT ( 'NONE',  ( 28.87500000122902932, -5.773502691896255534, -1.060575238724906372E-15 ) ) ;
#52559 = CARTESIAN_POINT ( 'NONE',  ( 19.05937500061451928, 0.000000000000000000, 5.243569643749999010 ) ) ;
#52560 = CARTESIAN_POINT ( 'NONE',  ( 8.259375000614518569, 0.000000000000000000, 5.243569643749999010 ) ) ;
#52561 = CARTESIAN_POINT ( 'NONE',  ( 45.00000000000000000, 0.000000000000000000, 0.000000000000000000 ) ) ;
#52562 = CARTESIAN_POINT ( 'NONE',  ( 7.715625000614515727, 3.027376345333611329, 5.243569643749999010 ) ) ;
#52563 = CARTESIAN_POINT ( 'NONE',  ( 16.67812500061451786, 4.541064518000418104, 2.621784821874999949 ) ) ;
#52564 = ORIENTED_EDGE ( 'NONE', *, *, #8903, .T. ) ;
#52565 = CARTESIAN_POINT ( 'NONE',  ( 6.337500001229033231, -4.330127018922194537, 2.499999999999995559 ) ) ;
#52566 = CARTESIAN_POINT ( 'NONE',  ( 15.25312500061451715, 4.541064518000418104, -2.621784821874998173 ) ) ;
#52567 = CARTESIAN_POINT ( 'NONE',  ( 11.69062500061451360, 6.054752690667223547, 3.707466751127219781E-16 ) ) ;
#52568 = CARTESIAN_POINT ( 'NONE',  ( 23.55937500061451573, 0.000000000000000000, 4.756430356249998326 ) ) ;
#52569 = CARTESIAN_POINT ( 'NONE',  ( 10.72500000000000142, -4.330127018922194537, 2.499999999999995559 ) ) ;
#52570 = CARTESIAN_POINT ( 'NONE',  ( 5.437500001229035540, -4.330127018922194537, 2.499999999999995559 ) ) ;
#52571 = CARTESIAN_POINT ( 'NONE',  ( 15.79687500061451821, 6.054752690667223547, 3.707466751127219781E-16 ) ) ;
#52572 = CARTESIAN_POINT ( 'NONE',  ( 18.26250000122903216, 4.330127018922192761, -2.499999999999997780 ) ) ;
#52573 = CARTESIAN_POINT ( 'NONE',  ( 25.16249999999999432, -5.773502691896255534, -1.060575238724906372E-15 ) ) ;
#52574 = CARTESIAN_POINT ( 'NONE',  ( 4.243569643749999898, 19.09062500061451573, -27.54997392385601529 ) ) ;
#52575 = CARTESIAN_POINT ( 'NONE',  ( -1.071796769724490783, 13.26740381056766616, 34.00000000000000711 ) ) ;
#52576 = CARTESIAN_POINT ( 'NONE',  ( 23.06250000122903288, -4.330127018922190985, -2.500000000000001332 ) ) ;
#52577 = CARTESIAN_POINT ( 'NONE',  ( 3.999999999999999112, 10.88750000122903394, -30.00000000000000000 ) ) ;
#52578 = CARTESIAN_POINT ( 'NONE',  ( 17.29687500061451999, -3.027376345333614438, 5.243569643749998122 ) ) ;
#52579 = CARTESIAN_POINT ( 'NONE',  ( 18.31875000122903430, 2.886751345948182834, 4.999999999999902300 ) ) ;
#52581 = ADVANCED_FACE ( 'NONE', ( #18480 ), #64652, .F. ) ;
#52580 = CIRCLE ( 'NONE', #20734, 4.000000000000003553 ) ;
#52582 = CARTESIAN_POINT ( 'NONE',  ( 15.02812500061451750, -4.541064518000419881, 2.621784821874995952 ) ) ;
#52583 = CARTESIAN_POINT ( 'NONE',  ( 9.543750001229033941, -2.886751345948125991, -5.000000000000000000 ) ) ;
#52584 = CARTESIAN_POINT ( 'NONE',  ( 8.849999999999999645, 0.000000000000000000, 4.999999999999998224 ) ) ;
#52585 = CARTESIAN_POINT ( 'NONE',  ( 24.42187500061451999, 3.027376345333611329, 5.243569643749999010 ) ) ;
#52586 = CARTESIAN_POINT ( 'NONE',  ( 18.90937500061451360, 2.746126346562643317, 4.756430356249998326 ) ) ;
#52587 = CARTESIAN_POINT ( 'NONE',  ( 9.665625000614515017, -6.054752690667223547, -1.112240025338166033E-15 ) ) ;
#52588 = CARTESIAN_POINT ( 'NONE',  ( 16.35937500061451644, 0.000000000000000000, 5.243569643749999010 ) ) ;
#52589 = ORIENTED_EDGE ( 'NONE', *, *, #41229, .T. ) ;
#52590 = CARTESIAN_POINT ( 'NONE',  ( 26.97187500061451360, 3.027376345333613106, -5.243569643749998122 ) ) ;
#52591 = CARTESIAN_POINT ( 'NONE',  ( 27.17812500061451786, -4.541064518000419881, 2.621784821874995952 ) ) ;
#52592 = CARTESIAN_POINT ( 'NONE',  ( 21.44062500061452070, -3.027376345333610441, -5.243569643749999898 ) ) ;
#52593 = CARTESIAN_POINT ( 'NONE',  ( 29.50312500061451360, -4.541064518000417216, -2.621784821875001281 ) ) ;
#52594 = DIRECTION ( 'NONE',  ( 0.000000000000000000, 0.000000000000000000, 1.000000000000000000 ) ) ;
#52595 = CARTESIAN_POINT ( 'NONE',  ( 9.899999999999998579, -4.330127018922190985, -2.500000000000001332 ) ) ;
#52596 = CARTESIAN_POINT ( 'NONE',  ( 20.25000000122903288, -2.886751345948129988, 4.999999999999997335 ) ) ;
#52597 = CARTESIAN_POINT ( 'NONE',  ( -1.071796769724491005, 18.67009619066136494, -34.00000000000000000 ) ) ;
#52598 = CARTESIAN_POINT ( 'NONE',  ( 11.33437500061451431, -2.746126346562646425, 4.756430356249996549 ) ) ;
#52599 = VERTEX_POINT ( 'NONE', #63917 ) ;
#52600 = CARTESIAN_POINT ( 'NONE',  ( 17.58749999999999858, -2.886751345948125991, -5.000000000000000000 ) ) ;
#52601 = CARTESIAN_POINT ( 'NONE',  ( 21.44999999999999929, 0.000000000000000000, 4.999999999999998224 ) ) ;
#52602 = CARTESIAN_POINT ( 'NONE',  ( 19.17187500061451999, -6.054752690667223547, -1.112240025338166033E-15 ) ) ;
#52603 = CARTESIAN_POINT ( 'NONE',  ( 12.89062500061451821, -3.027376345333610441, -5.243569643749999898 ) ) ;
#52604 = EDGE_LOOP ( 'NONE', ( #22124, #27092, #36341, #2710 ) ) ;
#52605 = CARTESIAN_POINT ( 'NONE',  ( 28.57499999999999929, 4.330127018922191873, 2.499999999999999556 ) ) ;
#52606 = CARTESIAN_POINT ( 'NONE',  ( 6.440625000614517148, -3.027376345333614438, 5.243569643749998122 ) ) ;
#52607 = CARTESIAN_POINT ( 'NONE',  ( 8.006250001229034297, 0.000000000000000000, 4.999999999999998224 ) ) ;
#52608 = CARTESIAN_POINT ( 'NONE',  ( 11.43750000000000000, 5.773502691896255534, 3.535250795749688894E-16 ) ) ;
#52609 = CARTESIAN_POINT ( 'NONE',  ( 28.65937500061451715, 2.746126346562645981, -4.756430356249997438 ) ) ;
#52610 = CARTESIAN_POINT ( 'NONE',  ( 2.121784821875001281, 14.10312500061451679, 33.67503911421598417 ) ) ;
#52611 = CARTESIAN_POINT ( 'NONE',  ( 2.896875000614518747, -3.027376345333614438, 5.243569643749998122 ) ) ;
#52612 = CARTESIAN_POINT ( 'NONE',  ( 8.662499999999999645, 2.886751345948129099, -4.999999999999998224 ) ) ;
#52613 = CARTESIAN_POINT ( 'NONE',  ( 3.756430356250000546, 16.27812499938548285, 27.83122392262697886 ) ) ;
#52614 = CARTESIAN_POINT ( 'NONE',  ( 24.04687500061451644, -3.027376345333614438, 5.243569643749998122 ) ) ;
#52615 = EDGE_LOOP ( 'NONE', ( #4866, #36055, #61369, #38531 ) ) ;
#52616 = CARTESIAN_POINT ( 'NONE',  ( 21.29062500061451502, -3.027376345333614438, 5.243569643749998122 ) ) ;
#52617 = CARTESIAN_POINT ( 'NONE',  ( 23.70937500061451786, -4.541064518000417216, -2.621784821875001281 ) ) ;
#52618 = CARTESIAN_POINT ( 'NONE',  ( -4.243569643749999898, 15.30312500061459247, -30.00000000000000000 ) ) ;
#52619 = CARTESIAN_POINT ( 'NONE',  ( 5.653125000614517504, -4.541064518000417216, -2.621784821875001281 ) ) ;
#52620 = CARTESIAN_POINT ( 'NONE',  ( 28.05937500061451573, 0.000000000000000000, 4.756430356249998326 ) ) ;
#52621 = CARTESIAN_POINT ( 'NONE',  ( 24.10312500061451502, -4.541064518000417216, -2.621784821875001281 ) ) ;
#52622 = CARTESIAN_POINT ( 'NONE',  ( 28.54687500061451644, -4.119189519843965641, -2.378215178125001383 ) ) ;
#52623 = CARTESIAN_POINT ( 'NONE',  ( 10.92187500061451644, 2.746126346562643317, 4.756430356249998326 ) ) ;
#52624 = CARTESIAN_POINT ( 'NONE',  ( 15.98437500061451821, -4.541064518000419881, 2.621784821874995952 ) ) ;
#52625 = CARTESIAN_POINT ( 'NONE',  ( 17.85937500061451999, -4.541064518000417216, -2.621784821875001281 ) ) ;
#52626 = CARTESIAN_POINT ( 'NONE',  ( 26.10937500061451644, 4.541064518000418104, -2.621784821874998173 ) ) ;
#52627 = CARTESIAN_POINT ( 'NONE',  ( -4.243569643749998122, 16.74687500061451573, 32.45002607614398471 ) ) ;
#52628 = CARTESIAN_POINT ( 'NONE',  ( 7.228125000614517681, 4.541064518000418104, 2.621784821874999949 ) ) ;
#52629 = CYLINDRICAL_SURFACE ( 'NONE', #27784, 4.999999999999998224 ) ;
#52630 = CARTESIAN_POINT ( 'NONE',  ( 4.434375000614519280, 6.421520780324663323E-16, -5.243569643749999010 ) ) ;
#52631 = CARTESIAN_POINT ( 'NONE',  ( 5.053125000614517859, 0.000000000000000000, 5.243569643749999010 ) ) ;
#52632 = CARTESIAN_POINT ( 'NONE',  ( 8.934375000614517504, 6.421520780324663323E-16, -5.243569643749999010 ) ) ;
#52633 = CARTESIAN_POINT ( 'NONE',  ( 17.40000000122903145, 5.773502691896255534, 3.535250795749688894E-16 ) ) ;
#52634 = CARTESIAN_POINT ( 'NONE',  ( 5.859375000614519102, 4.541064518000418104, -2.621784821874998173 ) ) ;
#52635 = CARTESIAN_POINT ( 'NONE',  ( 7.603125000614517681, 4.541064518000418104, -2.621784821874998173 ) ) ;
#52636 = CARTESIAN_POINT ( 'NONE',  ( 4.000000000000000000, 14.24374999877096748, 30.00000000000000000 ) ) ;
#52637 = CARTESIAN_POINT ( 'NONE',  ( 21.01875000122903003, 2.886751345948126879, 4.999999999999999112 ) ) ;
#52638 = CARTESIAN_POINT ( 'NONE',  ( 15.75937500061451857, 4.541064518000418104, -2.621784821874998173 ) ) ;
#52639 = ORIENTED_EDGE ( 'NONE', *, *, #62566, .F. ) ;
#52640 = CARTESIAN_POINT ( 'NONE',  ( 23.76562500061451644, 3.027376345333613106, -5.243569643749998122 ) ) ;
#52641 = CARTESIAN_POINT ( 'NONE',  ( 9.740625000614516082, -3.027376345333610441, -5.243569643749999898 ) ) ;
#52642 = CARTESIAN_POINT ( 'NONE',  ( 27.30937500061451573, -4.541064518000417216, -2.621784821875001281 ) ) ;
#52643 = CARTESIAN_POINT ( 'NONE',  ( 8.840625000614515727, -3.027376345333610441, -5.243569643749999898 ) ) ;
#52644 = CARTESIAN_POINT ( 'NONE',  ( 7.893750001229031810, 5.773502691896255534, 3.535250795749688401E-16 ) ) ;
#52645 = CARTESIAN_POINT ( 'NONE',  ( 10.23750000122903359, 4.330127018922191873, 2.499999999999999556 ) ) ;
#52646 = EDGE_CURVE ( 'NONE', #47727, #17166, #66368, .T. ) ;
#52647 = CARTESIAN_POINT ( 'NONE',  ( 24.25312500061451715, 4.541064518000418104, -2.621784821874998173 ) ) ;
#52648 = CARTESIAN_POINT ( 'NONE',  ( -2.121784821874999949, 12.07812500061451821, -33.67503911421598417 ) ) ;
#52649 = CARTESIAN_POINT ( 'NONE',  ( 13.20000000122903394, -2.886751345948125991, -5.000000000000000000 ) ) ;
#52650 = CARTESIAN_POINT ( 'NONE',  ( 22.56562500061451715, 3.027376345333611329, 5.243569643749999010 ) ) ;
#52651 = CARTESIAN_POINT ( 'NONE',  ( 20.87812500061451715, -4.541064518000419881, 2.621784821874995952 ) ) ;
#52652 = CARTESIAN_POINT ( 'NONE',  ( 29.82187500061451502, 2.746126346562643317, 4.756430356249998326 ) ) ;
#52653 = CARTESIAN_POINT ( 'NONE',  ( 19.98749999999999716, 5.773502691896255534, 3.535250795749688894E-16 ) ) ;
#52654 = CARTESIAN_POINT ( 'NONE',  ( 13.42500000122903536, 2.886751345948126879, 4.999999999999999112 ) ) ;
#52655 = CARTESIAN_POINT ( 'NONE',  ( 10.30312500061451431, 4.541064518000418104, -2.621784821874998173 ) ) ;
#52656 = CARTESIAN_POINT ( 'NONE',  ( 14.09062500061451750, -3.027376345333614438, 5.243569643749998122 ) ) ;
#52657 = CARTESIAN_POINT ( 'NONE',  ( 25.08750000122903145, 4.330127018922191873, 2.499999999999999556 ) ) ;
#52658 = CARTESIAN_POINT ( 'NONE',  ( 20.78437500061451715, 4.541064518000418104, 2.621784821874999949 ) ) ;
#52659 = CARTESIAN_POINT ( 'NONE',  ( 25.34999999999999787, 4.330127018922192761, -2.499999999999997780 ) ) ;
#52660 = CIRCLE ( 'NONE', #66866, 9.000000000000000000 ) ;
#52661 = ADVANCED_FACE ( 'NONE', ( #41046 ), #29225, .F. ) ;
#52662 = CARTESIAN_POINT ( 'NONE',  ( 8.850000001229034297, 5.773502691896255534, 3.535250795749688894E-16 ) ) ;
#52663 = CARTESIAN_POINT ( 'NONE',  ( 5.746875000614517504, -3.027376345333610441, -5.243569643749999898 ) ) ;
#52664 = CARTESIAN_POINT ( 'NONE',  ( 26.07187500061451857, 3.027376345333613106, -5.243569643749998122 ) ) ;
#52665 = LINE ( 'NONE', #35310, #64536 ) ;
#52666 = CARTESIAN_POINT ( 'NONE',  ( 22.26562500061451644, -6.054752690667223547, -1.112240025338166033E-15 ) ) ;
#52667 = CARTESIAN_POINT ( 'NONE',  ( 26.03437500061451715, 6.421520780324663323E-16, -5.243569643749999010 ) ) ;
#52668 = CARTESIAN_POINT ( 'NONE',  ( 1.878215178124997609, 17.17812499938548498, 33.25316411605952993 ) ) ;
#52669 = VECTOR ( 'NONE', #18819, 1000.000000000000000 ) ;
#52670 = CARTESIAN_POINT ( 'NONE',  ( 7.546875000614517326, -3.027376345333610441, -5.243569643749999898 ) ) ;
#52671 = CARTESIAN_POINT ( 'NONE',  ( 17.91562500061451502, 3.027376345333613106, -5.243569643749998122 ) ) ;
#52672 = EDGE_LOOP ( 'NONE', ( #44481, #42089, #37022, #53059 ) ) ;
#52673 = CARTESIAN_POINT ( 'NONE',  ( -1.071796769724504328, 12.89240381056766616, -26.00000000000001066 ) ) ;
#52674 = CARTESIAN_POINT ( 'NONE',  ( 27.02812500061451573, 4.541064518000418104, 2.621784821874999949 ) ) ;
#52675 = CARTESIAN_POINT ( 'NONE',  ( 4.959375000614516971, 4.541064518000418104, -2.621784821874998173 ) ) ;
#52676 = CARTESIAN_POINT ( 'NONE',  ( -5.810221930991193690E-16, 15.83749999999999680, -34.00000000000000000 ) ) ;
#52677 = CARTESIAN_POINT ( 'NONE',  ( 4.111889464957033447, 2.844708250062874200, 4.404844785106587501 ) ) ;
#52678 = CARTESIAN_POINT ( 'NONE',  ( 18.18750000000000000, 5.773502691896255534, 3.535250795749688894E-16 ) ) ;
#52679 = CARTESIAN_POINT ( 'NONE',  ( 20.61562500061451431, 3.027376345333613106, -5.243569643749998122 ) ) ;
#52680 = ORIENTED_EDGE ( 'NONE', *, *, #29219, .F. ) ;
#52681 = CARTESIAN_POINT ( 'NONE',  ( 24.44999999999999929, 4.330127018922192761, -2.499999999999997780 ) ) ;
#52682 =( BOUNDED_CURVE ( )  B_SPLINE_CURVE ( 2, ( #49321, #54854, #4263, #26786, #30852, #53387, #2782 ),
 .UNSPECIFIED., .F., .F. ) 
 B_SPLINE_CURVE_WITH_KNOTS ( ( 3, 2, 2, 3 ),
 ( 0.2200000000000000011, 0.2233333333333333282, 0.2266666666666666552, 0.2300000000000000100 ),
 .UNSPECIFIED. ) 
 CURVE ( )  GEOMETRIC_REPRESENTATION_ITEM ( )  RATIONAL_B_SPLINE_CURVE ( ( 1.000000000000000000, 0.8660254037844387076, 1.000000000000000000, 0.8660254037844387076, 1.000000000000000000, 0.8660254037844387076, 1.000000000000000000 ) ) 
 REPRESENTATION_ITEM ( '' )  );
#52683 = ADVANCED_FACE ( 'NONE', ( #24395 ), #7412, .F. ) ;
#52684 = CARTESIAN_POINT ( 'NONE',  ( 25.50937500061451502, -4.541064518000417216, -2.621784821875001281 ) ) ;
#52685 = ORIENTED_EDGE ( 'NONE', *, *, #28856, .T. ) ;
#52686 = CARTESIAN_POINT ( 'NONE',  ( 13.71562500061451750, -6.054752690667223547, -1.112240025338166033E-15 ) ) ;
#52687 = CARTESIAN_POINT ( 'NONE',  ( 4.903125000614516615, 4.541064518000418104, -2.621784821874998173 ) ) ;
#52688 = CARTESIAN_POINT ( 'NONE',  ( 15.45937500061451608, -5.492252693125287522, -1.008910452111647106E-15 ) ) ;
#52689 = CARTESIAN_POINT ( 'NONE',  ( 3.196875000614516793, 6.054752690667223547, 3.707466751127219781E-16 ) ) ;
#52690 = CARTESIAN_POINT ( 'NONE',  ( 14.88750000122903394, -4.330127018922194537, 2.499999999999995559 ) ) ;
#52691 = CARTESIAN_POINT ( 'NONE',  ( 19.61249999999999716, 2.886751345948126879, 4.999999999999999112 ) ) ;
#52692 = CARTESIAN_POINT ( 'NONE',  ( 28.01249999999999574, 2.886751345948129099, -4.999999999999998224 ) ) ;
#52693 = CARTESIAN_POINT ( 'NONE',  ( 5.521875000614517859, 3.027376345333611329, 5.243569643749999010 ) ) ;
#52694 = CARTESIAN_POINT ( 'NONE',  ( 9.046875000614518214, 6.054752690667223547, 3.707466751127219781E-16 ) ) ;
#52695 = CARTESIAN_POINT ( 'NONE',  ( 18.27187500061451431, -6.054752690667223547, -1.112240025338166033E-15 ) ) ;
#52696 = CARTESIAN_POINT ( 'NONE',  ( 11.38125000122903252, 6.123233995736764310E-16, -4.999999999999998224 ) ) ;
#52697 = ORIENTED_EDGE ( 'NONE', *, *, #7510, .F. ) ;
#52698 = CARTESIAN_POINT ( 'NONE',  ( 28.22812500061451502, 6.421520780324663323E-16, -5.243569643749999010 ) ) ;
#52699 = CARTESIAN_POINT ( 'NONE',  ( 29.40937500061451715, 0.000000000000000000, 5.243569643749999010 ) ) ;
#52700 = CARTESIAN_POINT ( 'NONE',  ( 3.796875000614517326, -3.027376345333614438, 5.243569643749998122 ) ) ;
#52701 = CARTESIAN_POINT ( 'NONE',  ( 16.64999999999999858, -4.330127018922190985, -2.500000000000001332 ) ) ;
#52702 = CARTESIAN_POINT ( 'NONE',  ( 12.85312500061451502, -4.541064518000417216, -2.621784821875001281 ) ) ;
#52703 = CARTESIAN_POINT ( 'NONE',  ( 3.999999999999999112, 14.03750000122903430, 30.00000000000000000 ) ) ;
#52704 = CARTESIAN_POINT ( 'NONE',  ( 27.03750000000000142, -2.886751345948142422, -4.999999999999970690 ) ) ;
#52705 = CARTESIAN_POINT ( 'NONE',  ( 19.35000000122903430, -2.886751345948129988, 4.999999999999997335 ) ) ;
#52706 = CARTESIAN_POINT ( 'NONE',  ( 1.970565482296614990, 9.811066920826819526, 24.31906361249631843 ) ) ;
#52707 = CARTESIAN_POINT ( 'NONE',  ( 17.22187500061451715, 2.746126346562643317, 4.756430356249998326 ) ) ;
#52708 = CARTESIAN_POINT ( 'NONE',  ( 8.278125000614515727, -4.541064518000419881, 2.621784821874995952 ) ) ;
#52709 = CARTESIAN_POINT ( 'NONE',  ( 23.89687500061451786, 6.054752690667223547, 3.707466751127219781E-16 ) ) ;
#52710 = FACE_OUTER_BOUND ( 'NONE', #17780, .T. ) ;
#52711 = CARTESIAN_POINT ( 'NONE',  ( 27.08437500061451786, 4.541064518000418104, 2.621784821874999949 ) ) ;
#52712 = CARTESIAN_POINT ( 'NONE',  ( 8.587500000000002132, -2.886751345948125991, -5.000000000000000000 ) ) ;
#52713 = CARTESIAN_POINT ( 'NONE',  ( 3.999999999999999112, 13.58750000122903323, 30.00000000000000000 ) ) ;
#52714 = CARTESIAN_POINT ( 'NONE',  ( 13.90312500061451750, 4.541064518000418104, -2.621784821874998173 ) ) ;
#52715 = CARTESIAN_POINT ( 'NONE',  ( 6.037500001229035185, 6.123233995736764310E-16, -4.999999999999998224 ) ) ;
#52716 = CARTESIAN_POINT ( 'NONE',  ( 12.64687500061451608, 6.054752690667223547, 3.707466751127219781E-16 ) ) ;
#52717 = CARTESIAN_POINT ( 'NONE',  ( -2.482458701038962712, 4.346511033910189781, -26.85332358594694924 ) ) ;
#52718 = EDGE_LOOP ( 'NONE', ( #42915, #53402, #30372, #27781 ) ) ;
#52719 = CARTESIAN_POINT ( 'NONE',  ( 11.31562500061451892, 3.027376345333611329, 5.243569643749999010 ) ) ;
#52720 = CARTESIAN_POINT ( 'NONE',  ( 1.071796769724488785, 19.55134618820330417, 34.00000000000000000 ) ) ;
#52721 = CARTESIAN_POINT ( 'NONE',  ( 23.70000000122903216, 5.773502691896255534, 3.535250795749688894E-16 ) ) ;
#52722 = CARTESIAN_POINT ( 'NONE',  ( 11.82187500061451679, 3.027376345333611329, 5.243569643749999010 ) ) ;
#52723 = AXIS2_PLACEMENT_3D ( 'NONE', #64916, #30577, #35747 ) ;
#52724 = CARTESIAN_POINT ( 'NONE',  ( 13.49062500061451608, 6.054752690667223547, 3.707466751127219781E-16 ) ) ;
#52725 = CARTESIAN_POINT ( 'NONE',  ( 45.00000000000000000, -6.363961030678871644, 6.363961030678982667 ) ) ;
#52726 = CARTESIAN_POINT ( 'NONE',  ( 24.83437500061451431, 4.541064518000418104, 2.621784821874999949 ) ) ;
#52727 = CARTESIAN_POINT ( 'NONE',  ( 7.246875000614514839, 0.000000000000000000, 4.756430356249998326 ) ) ;
#52728 = VECTOR ( 'NONE', #11366, 1000.000000000000000 ) ;
#52729 = CARTESIAN_POINT ( 'NONE',  ( 5.325000000000000178, -4.330127018922194537, 2.499999999999995559 ) ) ;
#52730 = CARTESIAN_POINT ( 'NONE',  ( 8.062500001229034652, 0.000000000000000000, 4.999999999999998224 ) ) ;
#52731 = CARTESIAN_POINT ( 'NONE',  ( -2.121784821874996840, 16.33437500061451786, -26.32496088578401583 ) ) ;
#52732 = CARTESIAN_POINT ( 'NONE',  ( 15.57187500061451679, -6.054752690667223547, -1.112240025338166033E-15 ) ) ;
#52733 = CARTESIAN_POINT ( 'NONE',  ( 18.60000000122903430, -2.886751345948125991, -5.000000000000000000 ) ) ;
#52734 = CARTESIAN_POINT ( 'NONE',  ( 12.64687500061451608, 6.054752690667223547, 3.707466751127219781E-16 ) ) ;
#52735 = CARTESIAN_POINT ( 'NONE',  ( -4.243569643749999898, 19.80312500061451786, -30.00000000000000000 ) ) ;
#52736 = CARTESIAN_POINT ( 'NONE',  ( 19.53750000122903430, 6.123233995736764310E-16, -4.999999999999998224 ) ) ;
#52737 = CARTESIAN_POINT ( 'NONE',  ( 12.21562500061451573, 3.027376345333611329, 5.243569643749999010 ) ) ;
#52738 = ORIENTED_EDGE ( 'NONE', *, *, #4935, .F. ) ;
#52739 = ORIENTED_EDGE ( 'NONE', *, *, #72113, .T. ) ;
#52740 = CARTESIAN_POINT ( 'NONE',  ( 17.62500000000000000, 6.123233995736764310E-16, -4.999999999999998224 ) ) ;
#52741 = PLANE ( 'NONE',  #53887 ) ;
#52742 = CARTESIAN_POINT ( 'NONE',  ( 11.89687500061451608, -3.027376345333614438, 5.243569643749998122 ) ) ;
#52743 = CARTESIAN_POINT ( 'NONE',  ( 22.46250000000000213, -5.773502691896255534, -1.060575238724906372E-15 ) ) ;
#52744 = CARTESIAN_POINT ( 'NONE',  ( 11.92500000122903181, 2.886751345948129099, -4.999999999999998224 ) ) ;
#52745 = CARTESIAN_POINT ( 'NONE',  ( 21.15000000122903145, -2.886751345948129988, 4.999999999999997335 ) ) ;
#52746 = CARTESIAN_POINT ( 'NONE',  ( 18.06562500061451715, 3.027376345333611329, 5.243569643749999010 ) ) ;
#52747 = EDGE_CURVE ( 'NONE', #32704, #22971, #12946, .T. ) ;
#52748 = CARTESIAN_POINT ( 'NONE',  ( 19.60312500061451502, -4.541064518000417216, -2.621784821875001281 ) ) ;
#52749 = CARTESIAN_POINT ( 'NONE',  ( 29.10000000122903074, 5.773502691896255534, 3.535250795749688894E-16 ) ) ;
#52750 =( BOUNDED_CURVE ( )  B_SPLINE_CURVE ( 2, ( #4015, #71607, #14348, #8441, #43534, #70133, #15433 ),
 .UNSPECIFIED., .F., .F. ) 
 B_SPLINE_CURVE_WITH_KNOTS ( ( 3, 2, 2, 3 ),
 ( 0.9429739840102342452, 0.9444444444444444198, 0.9472222222222221877, 0.9485519436316427466 ),
 .UNSPECIFIED. ) 
 CURVE ( )  GEOMETRIC_REPRESENTATION_ITEM ( )  RATIONAL_B_SPLINE_CURVE ( ( 0.9332437672470215162, 0.9290784365472635198, 1.000000000000000000, 0.8660254037844387076, 1.000000000000000000, 0.9358663999937293365, 0.9331342711013768110 ) ) 
 REPRESENTATION_ITEM ( '' )  );
#52751 = CARTESIAN_POINT ( 'NONE',  ( 27.52500000000000213, 6.123233995736764310E-16, -4.999999999999998224 ) ) ;
#52752 = CARTESIAN_POINT ( 'NONE',  ( 1.878215178125000495, 12.71562499938548463, 26.74683588394047007 ) ) ;
#52753 = CARTESIAN_POINT ( 'NONE',  ( 29.69999999999999574, -4.330127018922190985, -2.500000000000001332 ) ) ;
#52754 = CARTESIAN_POINT ( 'NONE',  ( 27.34687500061451360, -3.027376345333610441, -5.243569643749999898 ) ) ;
#52755 = CARTESIAN_POINT ( 'NONE',  ( 1.999999999999998668, 10.06250000122903465, -33.46410161513775705 ) ) ;
#52756 = CARTESIAN_POINT ( 'NONE',  ( -4.243569643749999898, 14.87187500061451928, -32.45002607614398471 ) ) ;
#52757 = CARTESIAN_POINT ( 'NONE',  ( 3.450000001229036162, 5.773502691896255534, 3.535250795749688894E-16 ) ) ;
#52758 = CARTESIAN_POINT ( 'NONE',  ( 6.000000000000001776, 4.330127018922192761, -2.499999999999997780 ) ) ;
#52759 = CARTESIAN_POINT ( 'NONE',  ( 2.775000001229033675, -5.773502691896255534, -1.060575238724906372E-15 ) ) ;
#52760 = CARTESIAN_POINT ( 'NONE',  ( 9.984375000614518214, 4.541064518000418104, 2.621784821874999949 ) ) ;
#52761 = CARTESIAN_POINT ( 'NONE',  ( 29.20312500061451644, 4.541064518000418104, -2.621784821874998173 ) ) ;
#52762 = CARTESIAN_POINT ( 'NONE',  ( 45.00000000000000000, 0.000000000000000000, 0.000000000000000000 ) ) ;
#52763 = CARTESIAN_POINT ( 'NONE',  ( -4.518949595698578570, 8.925733855591198918, -26.03435065765658152 ) ) ;
#52764 = DIRECTION ( 'NONE',  ( -0.000000000000000000, -1.000000000000000000, -0.000000000000000000 ) ) ;
#52765 = CARTESIAN_POINT ( 'NONE',  ( 7.209375000614519635, 4.541064518000418104, -2.621784821874998173 ) ) ;
#52766 = CARTESIAN_POINT ( 'NONE',  ( 10.95937500061451964, 0.000000000000000000, 5.243569643749999010 ) ) ;
#52767 = CARTESIAN_POINT ( 'NONE',  ( 7.650000000000000355, -4.330127018922190985, -2.500000000000001332 ) ) ;
#52768 = ADVANCED_FACE ( 'NONE', ( #58363 ), #63195, .F. ) ;
#52769 = CARTESIAN_POINT ( 'NONE',  ( -4.243569643749999898, 15.71562500061459744, 27.54997392385601529 ) ) ;
#52770 = CARTESIAN_POINT ( 'NONE',  ( 2.645498907222010754, 25.30421092789820392, 26.98856407078577391 ) ) ;
#52771 = CARTESIAN_POINT ( 'NONE',  ( 6.937499999999999112, 5.773502691896255534, 3.535250795749688894E-16 ) ) ;
#52772 = CARTESIAN_POINT ( 'NONE',  ( 14.25937500061451679, 2.746126346562645981, -4.756430356249997438 ) ) ;
#52773 = CARTESIAN_POINT ( 'NONE',  ( 20.65312500061451573, 4.541064518000418104, -2.621784821874998173 ) ) ;
#52774 = CARTESIAN_POINT ( 'NONE',  ( 12.81562500061451537, -6.054752690667223547, -1.112240025338166033E-15 ) ) ;
#52775 = CARTESIAN_POINT ( 'NONE',  ( 23.55937500061451573, -5.492252693125287522, -1.008910452111647106E-15 ) ) ;
#52776 = CARTESIAN_POINT ( 'NONE',  ( 10.05937500061451750, 0.000000000000000000, 5.243569643749999010 ) ) ;
#52777 = CARTESIAN_POINT ( 'NONE',  ( 25.80000000000000071, 4.330127018922192761, -2.499999999999997780 ) ) ;
#52778 = CARTESIAN_POINT ( 'NONE',  ( 22.65000000122903856, -2.886751345948125991, -5.000000000000000000 ) ) ;
#52779 = CARTESIAN_POINT ( 'NONE',  ( 17.10000000000000142, -4.330127018922190985, -2.500000000000001332 ) ) ;
#52780 = CARTESIAN_POINT ( 'NONE',  ( 12.42187500061451821, -6.054752690667223547, -1.112240025338166033E-15 ) ) ;
#52781 = CARTESIAN_POINT ( 'NONE',  ( 26.59687500061451360, 6.054752690667223547, 3.707466751127219781E-16 ) ) ;
#52782 = CARTESIAN_POINT ( 'NONE',  ( 28.03125000122903288, 6.123233995736764310E-16, -4.999999999999998224 ) ) ;
#52783 = EDGE_CURVE ( 'NONE', #55608, #15201, #8242, .T. ) ;
#52784 = DIRECTION ( 'NONE',  ( -0.000000000000000000, -1.000000000000000000, -0.000000000000000000 ) ) ;
#52785 = CARTESIAN_POINT ( 'NONE',  ( 20.93437500061451573, -4.541064518000419881, 2.621784821874995952 ) ) ;
#52786 = CARTESIAN_POINT ( 'NONE',  ( 12.45937500061451786, -4.541064518000417216, -2.621784821875001281 ) ) ;
#52787 = CARTESIAN_POINT ( 'NONE',  ( 1.878215178125000495, 19.57812499938548356, 26.74683588394047007 ) ) ;
#52788 = CARTESIAN_POINT ( 'NONE',  ( 24.44999999999999929, 4.330127018922192761, -2.499999999999997780 ) ) ;
#52789 = CARTESIAN_POINT ( 'NONE',  ( 3.756430356250000102, 19.84062499938548640, 30.00000000000000000 ) ) ;
#52790 = CARTESIAN_POINT ( 'NONE',  ( -4.243569643749999898, 12.65937500061451715, -30.00000000000000000 ) ) ;
#52791 = CARTESIAN_POINT ( 'NONE',  ( 27.57187500061451857, 2.746126346562643317, 4.756430356249998326 ) ) ;
#52792 = CARTESIAN_POINT ( 'NONE',  ( 13.94062500061451892, 6.054752690667223547, 3.707466751127219781E-16 ) ) ;
#52793 = CARTESIAN_POINT ( 'NONE',  ( 5.287500000000000533, -2.886751345948129988, 4.999999999999997335 ) ) ;
#52794 = DIRECTION ( 'NONE',  ( 0.000000000000000000, 0.000000000000000000, 1.000000000000000000 ) ) ;
#52795 = LINE ( 'NONE', #67709, #43238 ) ;
#52796 = CARTESIAN_POINT ( 'NONE',  ( 15.59999999999999964, 0.000000000000000000, 4.999999999999998224 ) ) ;
#52797 = CARTESIAN_POINT ( 'NONE',  ( 2.000000000000001332, 19.36250000122903359, 33.46410161513774995 ) ) ;
#52798 = CARTESIAN_POINT ( 'NONE',  ( 13.68750000122903288, 6.123233995736764310E-16, -4.999999999999998224 ) ) ;
#52799 = CARTESIAN_POINT ( 'NONE',  ( 23.97187500061451360, 3.027376345333611329, 5.243569643749999010 ) ) ;
#52800 = CARTESIAN_POINT ( 'NONE',  ( 3.422429900546629877, -3.645130117820770455, -3.769356580772429410 ) ) ;
#52801 = EDGE_LOOP ( 'NONE', ( #13312, #8483, #7518, #47830 ) ) ;
#52802 = CARTESIAN_POINT ( 'NONE',  ( 18.66562500061451146, -6.054752690667223547, -1.112240025338166033E-15 ) ) ;
#52803 = CARTESIAN_POINT ( 'NONE',  ( 3.740625000614516527, -3.027376345333614438, 5.243569643749998122 ) ) ;
#52804 = CARTESIAN_POINT ( 'NONE',  ( 21.12187500061451573, 3.027376345333613106, -5.243569643749998122 ) ) ;
#52805 = CARTESIAN_POINT ( 'NONE',  ( 3.862500000000001155, 2.886751345948126879, 4.999999999999999112 ) ) ;
#52806 = CARTESIAN_POINT ( 'NONE',  ( 6.365625000614518747, 3.027376345333611329, 5.243569643749999010 ) ) ;
#52807 = CARTESIAN_POINT ( 'NONE',  ( 22.52812500061451573, 4.541064518000418104, 2.621784821874999949 ) ) ;
#52808 = CARTESIAN_POINT ( 'NONE',  ( 4.243569643749999898, 15.94062500061451537, 32.45002607614398471 ) ) ;
#52809 = CARTESIAN_POINT ( 'NONE',  ( 18.26250000122903216, 4.330127018922192761, -2.499999999999997780 ) ) ;
#52810 = CARTESIAN_POINT ( 'NONE',  ( 12.08437500061451608, 5.824947211148865298E-16, -4.756430356249998326 ) ) ;
#52811 = CARTESIAN_POINT ( 'NONE',  ( 8.990625000614517859, 6.054752690667223547, 3.707466751127219781E-16 ) ) ;
#52812 = ADVANCED_FACE ( 'NONE', ( #2241 ), #64282, .F. ) ;
#52813 = CARTESIAN_POINT ( 'NONE',  ( 3.684375000614518836, 4.541064518000418104, 2.621784821874999949 ) ) ;
#52814 = CARTESIAN_POINT ( 'NONE',  ( 28.67812500061451431, 6.421520780324663323E-16, -5.243569643749999010 ) ) ;
#52815 = CARTESIAN_POINT ( 'NONE',  ( 22.28437500061451715, -4.541064518000419881, 2.621784821874995952 ) ) ;
#52816 = CARTESIAN_POINT ( 'NONE',  ( 13.86562500061451431, 3.027376345333613106, -5.243569643749998122 ) ) ;
#52817 = CARTESIAN_POINT ( 'NONE',  ( 23.96250000122903145, -4.330127018922190985, -2.500000000000001332 ) ) ;
#52818 = CARTESIAN_POINT ( 'NONE',  ( 24.59062500061451573, -3.027376345333610441, -5.243569643749999898 ) ) ;
#52819 = CARTESIAN_POINT ( 'NONE',  ( 18.94687500061451502, 6.054752690667223547, 3.707466751127219781E-16 ) ) ;
#52820 = CARTESIAN_POINT ( 'NONE',  ( 14.54062500061451679, -3.027376345333614438, 5.243569643749998122 ) ) ;
#52821 = CARTESIAN_POINT ( 'NONE',  ( 9.001249775931846008E-16, 17.27187500061451786, 34.90005215228797653 ) ) ;
#52822 = CARTESIAN_POINT ( 'NONE',  ( 20.27812500061451573, 4.541064518000418104, 2.621784821874999949 ) ) ;
#52823 = CARTESIAN_POINT ( 'NONE',  ( 29.15625000122903288, 0.000000000000000000, 4.999999999999998224 ) ) ;
#52824 = ORIENTED_EDGE ( 'NONE', *, *, #20472, .T. ) ;
#52825 = CARTESIAN_POINT ( 'NONE',  ( 24.44999999999999929, 4.330127018922192761, -2.499999999999997780 ) ) ;
#52826 = CARTESIAN_POINT ( 'NONE',  ( -0.6945855716117766976, 10.00052347946771825, -33.93923227085034000 ) ) ;
#52827 = CARTESIAN_POINT ( 'NONE',  ( -3.756430356250001434, 20.21562499938548285, 32.16877607737301048 ) ) ;
#52828 = CARTESIAN_POINT ( 'NONE',  ( 27.81562500061452070, 3.027376345333613106, -5.243569643749998122 ) ) ;
#52829 = CARTESIAN_POINT ( 'NONE',  ( 8.615625000614517859, 3.027376345333611329, 5.243569643749999010 ) ) ;
#52830 = CARTESIAN_POINT ( 'NONE',  ( 18.67500000122903714, 2.886751345948129099, -4.999999999999998224 ) ) ;
#52831 = ADVANCED_FACE ( 'NONE', ( #47660 ), #19570, .F. ) ;
#52832 = VECTOR ( 'NONE', #30539, 1000.000000000000000 ) ;
#52833 = CARTESIAN_POINT ( 'NONE',  ( 24.21562500061451573, 3.027376345333613106, -5.243569643749998122 ) ) ;
#52834 = CARTESIAN_POINT ( 'NONE',  ( 26.21249999999999858, 2.886751345948129099, -4.999999999999998224 ) ) ;
#52835 = CARTESIAN_POINT ( 'NONE',  ( 3.999999999999999112, 15.83750000122903501, -30.00000000000000000 ) ) ;
#52836 = CARTESIAN_POINT ( 'NONE',  ( 30.00000000000000000, 6.123233995736764310E-16, -4.999999999999998224 ) ) ;
#52837 = CARTESIAN_POINT ( 'NONE',  ( 9.628125000614517148, -4.541064518000419881, 2.621784821874995952 ) ) ;
#52838 = ORIENTED_EDGE ( 'NONE', *, *, #3226, .F. ) ;
#52839 = CARTESIAN_POINT ( 'NONE',  ( 25.64062500061451644, 6.054752690667223547, 3.707466751127219781E-16 ) ) ;
#52840 = CARTESIAN_POINT ( 'NONE',  ( 8.428125000614517859, 6.421520780324663323E-16, -5.243569643749999010 ) ) ;
#52841 = CARTESIAN_POINT ( 'NONE',  ( 14.18437500061451750, -4.119189519843968306, 2.378215178124996054 ) ) ;
#52842 = VECTOR ( 'NONE', #41413, 1000.000000000000000 ) ;
#52843 = CARTESIAN_POINT ( 'NONE',  ( 17.96250000122903501, 0.000000000000000000, 4.999999999999998224 ) ) ;
#52844 = CARTESIAN_POINT ( 'NONE',  ( 12.41249999999999964, 2.886751345948126879, 4.999999999999999112 ) ) ;
#52845 = CARTESIAN_POINT ( 'NONE',  ( 13.73437500061451821, -4.541064518000419881, 2.621784821874995952 ) ) ;
#52846 = CARTESIAN_POINT ( 'NONE',  ( 8.475000001229034297, 2.886751345948126879, 4.999999999999999112 ) ) ;
#52847 = CARTESIAN_POINT ( 'NONE',  ( 17.89687500061451431, -3.027376345333610441, -5.243569643749999898 ) ) ;
#52848 = CARTESIAN_POINT ( 'NONE',  ( 18.03749999999999787, -2.886751345948125991, -5.000000000000000000 ) ) ;
#52849 = CARTESIAN_POINT ( 'NONE',  ( 9.234375000614518214, -4.541064518000419881, 2.621784821874995952 ) ) ;
#52850 = CARTESIAN_POINT ( 'NONE',  ( -4.243569643749999898, 12.60312500061451679, -30.00000000000000000 ) ) ;
#52851 = CARTESIAN_POINT ( 'NONE',  ( -3.999999999999999112, 11.86249999999999893, -32.30940107675850470 ) ) ;
#52852 = CARTESIAN_POINT ( 'NONE',  ( 22.39687500061451431, 4.119189519843966529, -2.378215178124998275 ) ) ;
#52853 = CARTESIAN_POINT ( 'NONE',  ( 15.82499999999999929, 6.123233995736764310E-16, -4.999999999999998224 ) ) ;
#52854 = CARTESIAN_POINT ( 'NONE',  ( 25.37812500061451715, -4.541064518000419881, 2.621784821874995952 ) ) ;
#52855 = CYLINDRICAL_SURFACE ( 'NONE', #40366, 4.000000000000000000 ) ;
#52856 = CARTESIAN_POINT ( 'NONE',  ( 25.54687500061451644, -3.027376345333610441, -5.243569643749999898 ) ) ;
#52857 = CARTESIAN_POINT ( 'NONE',  ( 29.63437500061451502, 6.421520780324663323E-16, -5.243569643749999010 ) ) ;
#52858 = CARTESIAN_POINT ( 'NONE',  ( 22.98749999999999716, -2.886751345948125991, -5.000000000000000000 ) ) ;
#52859 = CARTESIAN_POINT ( 'NONE',  ( 6.140625000614516438, -3.027376345333610441, -5.243569643749999898 ) ) ;
#52860 = CARTESIAN_POINT ( 'NONE',  ( 22.05937500061451217, 2.746126346562643317, 4.756430356249998326 ) ) ;
#52861 = CARTESIAN_POINT ( 'NONE',  ( 15.60937500061451644, -4.541064518000417216, -2.621784821875001281 ) ) ;
#52862 = CARTESIAN_POINT ( 'NONE',  ( 9.421875000614514661, 4.119189519843966529, 2.378215178124999607 ) ) ;
#52863 = CARTESIAN_POINT ( 'NONE',  ( 3.928125000614516527, 6.421520780324663323E-16, -5.243569643749999010 ) ) ;
#52864 = CARTESIAN_POINT ( 'NONE',  ( 9.384375000614518569, 6.421520780324663323E-16, -5.243569643749999010 ) ) ;
#52865 = CARTESIAN_POINT ( 'NONE',  ( 17.97187500061451715, 3.027376345333613106, -5.243569643749998122 ) ) ;
#52866 = CARTESIAN_POINT ( 'NONE',  ( 21.67500000000000071, 6.123233995736764310E-16, -4.999999999999998224 ) ) ;
#52867 = CARTESIAN_POINT ( 'NONE',  ( 27.75000000000000000, 0.000000000000000000, 4.999999999999998224 ) ) ;
#52868 = CARTESIAN_POINT ( 'NONE',  ( 27.57187500061451857, 3.027376345333611329, 5.243569643749999010 ) ) ;
#52869 = CARTESIAN_POINT ( 'NONE',  ( 19.23750000000000071, -2.886751345948157965, 4.999999999999948486 ) ) ;
#52870 = CARTESIAN_POINT ( 'NONE',  ( 16.05000000000000071, 0.000000000000000000, 4.999999999999998224 ) ) ;
#52871 = ORIENTED_EDGE ( 'NONE', *, *, #57914, .T. ) ;
#52872 = CARTESIAN_POINT ( 'NONE',  ( 11.36250000000000071, 2.886751345948129099, -4.999999999999998224 ) ) ;
#52873 = CARTESIAN_POINT ( 'NONE',  ( 11.40937500061451360, -5.492252693125287522, -1.008910452111647106E-15 ) ) ;
#52874 = CARTESIAN_POINT ( 'NONE',  ( 21.25312500061451715, 0.000000000000000000, 5.243569643749999010 ) ) ;
#52875 = CARTESIAN_POINT ( 'NONE',  ( 11.62500000000000000, -4.330127018922194537, 2.499999999999995559 ) ) ;
#52876 = CARTESIAN_POINT ( 'NONE',  ( 9.262500001229033941, 4.330127018922192761, -2.499999999999997780 ) ) ;
#52877 = CARTESIAN_POINT ( 'NONE',  ( 6.815625000614517148, 3.027376345333611329, 5.243569643749999010 ) ) ;
#52878 = CARTESIAN_POINT ( 'NONE',  ( 21.78750000000000142, 5.773502691896255534, 3.535250795749688894E-16 ) ) ;
#52879 = CARTESIAN_POINT ( 'NONE',  ( 20.91562500061451502, -6.054752690667223547, -1.112240025338166033E-15 ) ) ;
#52880 = CARTESIAN_POINT ( 'NONE',  ( 12.22499999999999964, 6.123233995736764310E-16, -4.999999999999998224 ) ) ;
#52881 = CARTESIAN_POINT ( 'NONE',  ( 26.77500000122903145, 2.886751345948129099, -4.999999999999998224 ) ) ;
#52882 = CARTESIAN_POINT ( 'NONE',  ( 3.756430356250000546, 20.32812499938548711, 27.83122392262697886 ) ) ;
#52883 = CARTESIAN_POINT ( 'NONE',  ( 5.325000000000000178, -4.330127018922194537, 2.499999999999995559 ) ) ;
#52884 = ORIENTED_EDGE ( 'NONE', *, *, #66833, .T. ) ;
#52885 = CARTESIAN_POINT ( 'NONE',  ( 19.15312500061451573, -4.541064518000417216, -2.621784821875001281 ) ) ;
#52886 = CARTESIAN_POINT ( 'NONE',  ( 27.77812500061451573, 6.421520780324663323E-16, -5.243569643749999010 ) ) ;
#52887 = CARTESIAN_POINT ( 'NONE',  ( 28.02187500061451431, 3.027376345333611329, 5.243569643749999010 ) ) ;
#52888 = CARTESIAN_POINT ( 'NONE',  ( 14.65312500061451573, -4.541064518000417216, -2.621784821875001281 ) ) ;
#52889 = CARTESIAN_POINT ( 'NONE',  ( 3.999999999999998668, 11.26250000000000107, 27.69059892324149530 ) ) ;
#52890 = EDGE_CURVE ( 'NONE', #29218, #50573, #58723, .T. ) ;
#52891 = CARTESIAN_POINT ( 'NONE',  ( 7.865625000614516971, -6.054752690667223547, -1.112240025338166033E-15 ) ) ;
#52892 = CARTESIAN_POINT ( 'NONE',  ( 4.758977648302459507, 1.540231855627056223, -4.851099530879135813 ) ) ;
#52893 = CARTESIAN_POINT ( 'NONE',  ( 26.85000000122903430, 5.773502691896255534, 3.535250795749688894E-16 ) ) ;
#52894 = CARTESIAN_POINT ( 'NONE',  ( 18.34687500061451715, -2.746126346562641984, -4.756430356249999214 ) ) ;
#52895 = CARTESIAN_POINT ( 'NONE',  ( 17.16562500061451502, 3.027376345333611329, 5.243569643749999010 ) ) ;
#52896 = CARTESIAN_POINT ( 'NONE',  ( 29.55937500061451573, -4.541064518000417216, -2.621784821875001281 ) ) ;
#52897 =( BOUNDED_CURVE ( )  B_SPLINE_CURVE ( 2, ( #64029, #57757, #29694, #47054, #51869, #30425, #6442 ),
 .UNSPECIFIED., .F., .F. ) 
 B_SPLINE_CURVE_WITH_KNOTS ( ( 3, 2, 2, 3 ),
 ( 0.4083333333333333814, 0.4111111111111111494, 0.4138888888888889173, 0.4166666666666667407 ),
 .UNSPECIFIED. ) 
 CURVE ( )  GEOMETRIC_REPRESENTATION_ITEM ( )  RATIONAL_B_SPLINE_CURVE ( ( 0.9999999999999973355, 0.8660254037844413721, 1.000000000000000000, 0.8660254037844387076, 1.000000000000000000, 0.8660254037844360431, 1.000000000000002665 ) ) 
 REPRESENTATION_ITEM ( '' )  );
#52898 = CARTESIAN_POINT ( 'NONE',  ( 10.17187500061451999, -6.054752690667223547, -1.112240025338166033E-15 ) ) ;
#52899 = CARTESIAN_POINT ( 'NONE',  ( 10.20937500061451786, -4.541064518000417216, -2.621784821875001281 ) ) ;
#52900 = CARTESIAN_POINT ( 'NONE',  ( 18.64687500061451786, -3.027376345333614438, 5.243569643749998122 ) ) ;
#52901 = ORIENTED_EDGE ( 'NONE', *, *, #65368, .T. ) ;
#52902 = CARTESIAN_POINT ( 'NONE',  ( 29.74687500061451217, 6.054752690667223547, 3.707466751127219781E-16 ) ) ;
#52903 = CARTESIAN_POINT ( 'NONE',  ( 21.96562500061451573, 3.027376345333613106, -5.243569643749998122 ) ) ;
#52904 = CARTESIAN_POINT ( 'NONE',  ( 17.59687500061451715, 6.054752690667223547, 3.707466751127219781E-16 ) ) ;
#52905 = CARTESIAN_POINT ( 'NONE',  ( 21.44062500061452070, -3.027376345333610441, -5.243569643749999898 ) ) ;
#52906 = CARTESIAN_POINT ( 'NONE',  ( 2.000000000000001332, 13.40000000000000213, 33.46410161513774995 ) ) ;
#52907 = CARTESIAN_POINT ( 'NONE',  ( 3.496875000614518836, -3.027376345333610441, -5.243569643749999898 ) ) ;
#52908 = CARTESIAN_POINT ( 'NONE',  ( 8.812500001229034652, 4.330127018922192761, -2.499999999999997780 ) ) ;
#52909 = ORIENTED_EDGE ( 'NONE', *, *, #31467, .T. ) ;
#52910 = CARTESIAN_POINT ( 'NONE',  ( 5.662500001229035185, 4.330127018922192761, -2.499999999999997780 ) ) ;
#52911 = CARTESIAN_POINT ( 'NONE',  ( 3.999999999999999112, 17.07499999999999929, -30.00000000000000000 ) ) ;
#52912 = CARTESIAN_POINT ( 'NONE',  ( 24.86250000122903359, -4.330127018922190985, -2.500000000000001332 ) ) ;
#52913 = CARTESIAN_POINT ( 'NONE',  ( 3.999999999999998668, 20.50624999877096499, 32.30940107675850470 ) ) ;
#52914 = CARTESIAN_POINT ( 'NONE',  ( 7.621875000614519280, 3.027376345333613106, -5.243569643749998122 ) ) ;
#52915 = DIRECTION ( 'NONE',  ( -1.000000000000000000, -0.000000000000000000, -0.000000000000000000 ) ) ;
#52916 = CARTESIAN_POINT ( 'NONE',  ( 13.94062500061451892, 6.054752690667223547, 3.707466751127219781E-16 ) ) ;
#52917 = CARTESIAN_POINT ( 'NONE',  ( 9.796875000614519990, -3.027376345333610441, -5.243569643749999898 ) ) ;
#52918 = CARTESIAN_POINT ( 'NONE',  ( 3.665625000614517681, 3.027376345333611329, 5.243569643749999010 ) ) ;
#52919 = CARTESIAN_POINT ( 'NONE',  ( 17.44687500061451502, -3.027376345333610441, -5.243569643749999898 ) ) ;
#52920 = CARTESIAN_POINT ( 'NONE',  ( 6.571875000614517681, -6.054752690667223547, -1.112240025338166033E-15 ) ) ;
#52921 = CARTESIAN_POINT ( 'NONE',  ( 3.999999999999998668, 17.56250000000000000, -32.30940107675850470 ) ) ;
#52922 = CARTESIAN_POINT ( 'NONE',  ( 6.815625000614517148, 3.027376345333611329, 5.243569643749999010 ) ) ;
#52923 = CARTESIAN_POINT ( 'NONE',  ( 18.62812500061451715, -4.541064518000419881, 2.621784821874995952 ) ) ;
#52924 = EDGE_CURVE ( 'NONE', #13105, #4055, #25867, .T. ) ;
#52925 = ORIENTED_EDGE ( 'NONE', *, *, #59515, .T. ) ;
#52926 = CARTESIAN_POINT ( 'NONE',  ( 14.69062500061451537, -3.027376345333610441, -5.243569643749999898 ) ) ;
#52927 = CARTESIAN_POINT ( 'NONE',  ( 10.04062500061451502, -3.027376345333614438, 5.243569643749998122 ) ) ;
#52928 = CARTESIAN_POINT ( 'NONE',  ( 24.68437500061451573, 5.824947211148865298E-16, -4.756430356249998326 ) ) ;
#52929 = CARTESIAN_POINT ( 'NONE',  ( 11.77500000000000036, 6.123233995736764310E-16, -4.999999999999998224 ) ) ;
#52930 = CARTESIAN_POINT ( 'NONE',  ( 6.112500001229034474, 4.330127018922192761, -2.499999999999997780 ) ) ;
#52931 = CARTESIAN_POINT ( 'NONE',  ( 14.03437500061451715, 4.541064518000418104, 2.621784821874999949 ) ) ;
#52932 = CARTESIAN_POINT ( 'NONE',  ( 16.65000000122903501, -2.886751345948129988, 4.999999999999997335 ) ) ;
#52933 = CARTESIAN_POINT ( 'NONE',  ( 24.60000000000000142, 0.000000000000000000, 4.999999999999998224 ) ) ;
#52934 = CARTESIAN_POINT ( 'NONE',  ( -4.243569643749999898, 9.921875000614519990, -32.45002607614398471 ) ) ;
#52935 = LINE ( 'NONE', #35220, #20605 ) ;
#52936 = LINE ( 'NONE', #2333, #18350 ) ;
#52937 = CARTESIAN_POINT ( 'NONE',  ( 12.73125000122903394, 6.123233995736764310E-16, -4.999999999999998224 ) ) ;
#52938 =( BOUNDED_CURVE ( )  B_SPLINE_CURVE ( 2, ( #67266, #5914, #18067, #5560, #61695, #17353, #62424, #39911, #67979 ),
 .UNSPECIFIED., .F., .F. ) 
 B_SPLINE_CURVE_WITH_KNOTS ( ( 3, 2, 2, 2, 3 ),
 ( 0.5543478260869565410, 0.5579710144927536586, 0.5652173913043477826, 0.5724637681159420177, 0.5760869565217391353 ),
 .UNSPECIFIED. ) 
 CURVE ( )  GEOMETRIC_REPRESENTATION_ITEM ( )  RATIONAL_B_SPLINE_CURVE ( ( 0.9330127018922194093, 0.9330127018922194093, 1.000000000000000000, 0.8660254037844387076, 1.000000000000000000, 0.8660254037844387076, 1.000000000000000000, 0.9330127018922194093, 0.9330127018922194093 ) ) 
 REPRESENTATION_ITEM ( '' )  );
#52939 = CARTESIAN_POINT ( 'NONE',  ( 30.00000000000000000, 0.000000000000000000, 0.000000000000000000 ) ) ;
#52940 = CARTESIAN_POINT ( 'NONE',  ( 18.87187500061451573, 3.027376345333613106, -5.243569643749998122 ) ) ;
#52941 = CARTESIAN_POINT ( 'NONE',  ( 29.47499999999999787, 4.330127018922191873, 2.499999999999999556 ) ) ;
#52942 = B_SPLINE_CURVE_WITH_KNOTS ( 'NONE', 3,
 ( #60945, #43608, #9620, #48421, #20319, #71685, #66129, #55419, #65395, #4456 ),
 .UNSPECIFIED., .F., .F.,
 ( 4, 3, 3, 4 ),
 ( 1.859757873009560816E-16, 7.861633092733088819E-05, 0.0001572323307352020715, 0.0002910318696070817368 ),
 .UNSPECIFIED. ) ;
#52943 = CARTESIAN_POINT ( 'NONE',  ( 14.95312500061451644, 0.000000000000000000, 5.243569643749999010 ) ) ;
#52944 = CARTESIAN_POINT ( 'NONE',  ( 7.368750001229035007, 2.886751345948129099, -4.999999999999998224 ) ) ;
#52945 = CARTESIAN_POINT ( 'NONE',  ( 23.78437500061451360, 6.421520780324663323E-16, -5.243569643749999010 ) ) ;
#52946 = CARTESIAN_POINT ( 'NONE',  ( 16.43437500061451573, -2.746126346562641984, -4.756430356249999214 ) ) ;
#52947 = CARTESIAN_POINT ( 'NONE',  ( 8.990625000614516082, 6.054752690667223547, 3.707466751127219781E-16 ) ) ;
#52948 = CARTESIAN_POINT ( 'NONE',  ( 15.83437500061451608, 4.541064518000418104, 2.621784821874999949 ) ) ;
#52949 = ORIENTED_EDGE ( 'NONE', *, *, #62426, .T. ) ;
#52950 = CARTESIAN_POINT ( 'NONE',  ( 25.05937500061451573, -4.541064518000417216, -2.621784821875001281 ) ) ;
#52951 = CARTESIAN_POINT ( 'NONE',  ( 27.59062500061451573, -3.027376345333614438, 5.243569643749998122 ) ) ;
#52952 = CARTESIAN_POINT ( 'NONE',  ( 16.79062500061451857, -3.027376345333614438, 5.243569643749998122 ) ) ;
#52953 = CARTESIAN_POINT ( 'NONE',  ( 29.69062500061451715, 6.054752690667223547, 3.707466751127219781E-16 ) ) ;
#52954 = CARTESIAN_POINT ( 'NONE',  ( 30.00000000000000000, 0.000000000000000000, 0.000000000000000000 ) ) ;
#52955 = CARTESIAN_POINT ( 'NONE',  ( 8.137500000000002842, -2.886751345948125991, -5.000000000000000000 ) ) ;
#52956 = CARTESIAN_POINT ( 'NONE',  ( 19.42500000122903714, -5.773502691896255534, -1.060575238724906372E-15 ) ) ;
#52957 = CARTESIAN_POINT ( 'NONE',  ( -3.999999999999997335, 10.13750000000000284, 32.30940107675850470 ) ) ;
#52958 = CARTESIAN_POINT ( 'NONE',  ( 11.67187500061451644, 4.119189519843966529, 2.378215178124999607 ) ) ;
#52959 = ORIENTED_EDGE ( 'NONE', *, *, #1978, .T. ) ;
#52960 = CARTESIAN_POINT ( 'NONE',  ( 18.33749999999999858, -2.886751345948129988, 4.999999999999997335 ) ) ;
#52961 = CARTESIAN_POINT ( 'NONE',  ( 18.56250000000000000, 2.886751345948129099, -4.999999999999998224 ) ) ;
#52962 = CARTESIAN_POINT ( 'NONE',  ( 19.69687500061451857, -3.027376345333610441, -5.243569643749999898 ) ) ;
#52963 = CARTESIAN_POINT ( 'NONE',  ( 13.90312500061451750, 4.541064518000418104, -2.621784821874998173 ) ) ;
#52964 =( BOUNDED_CURVE ( )  B_SPLINE_CURVE ( 2, ( #69734, #2146, #17655, #7672, #12850, #52380, #19103 ),
 .UNSPECIFIED., .F., .F. ) 
 B_SPLINE_CURVE_WITH_KNOTS ( ( 3, 2, 2, 3 ),
 ( 0.09166666666666660468, 0.09444444444444442810, 0.09722222222222223764, 0.1000000000000000611 ),
 .UNSPECIFIED. ) 
 CURVE ( )  GEOMETRIC_REPRESENTATION_ITEM ( )  RATIONAL_B_SPLINE_CURVE ( ( 1.000000000000002665, 0.8660254037844360431, 1.000000000000000000, 0.8660254037844387076, 1.000000000000000000, 0.8660254037844360431, 1.000000000000002665 ) ) 
 REPRESENTATION_ITEM ( '' )  );
#52965 = VERTEX_POINT ( 'NONE', #36943 ) ;
#52966 = CARTESIAN_POINT ( 'NONE',  ( 10.23750000000000071, -2.886751345948130876, 4.999999999999996447 ) ) ;
#52967 = CARTESIAN_POINT ( 'NONE',  ( 6.665625000614515905, 3.027376345333613106, -5.243569643749998122 ) ) ;
#52968 = CARTESIAN_POINT ( 'NONE',  ( 10.35000000000000142, -4.330127018922190985, -2.500000000000001332 ) ) ;
#52969 = CARTESIAN_POINT ( 'NONE',  ( 12.26249999999999929, 2.886751345948129099, -4.999999999999998224 ) ) ;
#52970 = CARTESIAN_POINT ( 'NONE',  ( 27.94687500061451502, 0.000000000000000000, 4.756430356249998326 ) ) ;
#52971 = CARTESIAN_POINT ( 'NONE',  ( -2.121784821874999949, 16.12812500061451715, 26.32496088578401938 ) ) ;
#52972 = CARTESIAN_POINT ( 'NONE',  ( 27.66562500061451146, -6.054752690667223547, -1.112240025338166033E-15 ) ) ;
#52973 = CARTESIAN_POINT ( 'NONE',  ( 8.849999999999999645, 0.000000000000000000, 4.999999999999998224 ) ) ;
#52974 = CARTESIAN_POINT ( 'NONE',  ( -3.756430356250000102, 17.36562499938548498, 30.00000000000000000 ) ) ;
#52975 = CARTESIAN_POINT ( 'NONE',  ( 24.98437500061451644, -4.541064518000419881, 2.621784821874995952 ) ) ;
#52976 = ORIENTED_EDGE ( 'NONE', *, *, #36421, .F. ) ;
#52977 = CARTESIAN_POINT ( 'NONE',  ( 22.30312500061451431, -4.541064518000417216, -2.621784821875001281 ) ) ;
#52978 = CARTESIAN_POINT ( 'NONE',  ( 22.73437500061451644, -4.541064518000419881, 2.621784821874995952 ) ) ;
#52979 = CARTESIAN_POINT ( 'NONE',  ( -2.121784821874996840, 15.37812500061459531, -26.32496088578401583 ) ) ;
#52980 = CARTESIAN_POINT ( 'NONE',  ( 7.528125000614515727, 6.421520780324663323E-16, -5.243569643749999010 ) ) ;
#52981 = CARTESIAN_POINT ( 'NONE',  ( 25.84687500061451715, -2.746126346562646425, 4.756430356249996549 ) ) ;
#52982 = CARTESIAN_POINT ( 'NONE',  ( 24.29062500061452212, 6.054752690667223547, 3.707466751127219781E-16 ) ) ;
#52983 = CARTESIAN_POINT ( 'NONE',  ( 10.20937500061451786, -4.119189519843965641, -2.378215178125001383 ) ) ;
#52984 = CARTESIAN_POINT ( 'NONE',  ( -3.756430356250001434, 16.95312499938548356, 32.16877607737301048 ) ) ;
#52985 = CARTESIAN_POINT ( 'NONE',  ( 17.37187500061451573, -6.054752690667223547, -1.112240025338166033E-15 ) ) ;
#52986 = CARTESIAN_POINT ( 'NONE',  ( 25.47187500061451715, -6.054752690667223547, -1.112240025338166033E-15 ) ) ;
#52987 = CARTESIAN_POINT ( 'NONE',  ( 4.243569643749999010, 14.27187500061451786, 27.54997392385601174 ) ) ;
#52988 = CARTESIAN_POINT ( 'NONE',  ( 7.753125000614518036, 0.000000000000000000, 5.243569643749999010 ) ) ;
#52989 = CARTESIAN_POINT ( 'NONE',  ( 28.07812500061451289, -4.541064518000419881, 2.621784821874995952 ) ) ;
#52990 = CARTESIAN_POINT ( 'NONE',  ( 3.159375000614518036, 4.541064518000418104, -2.621784821874998173 ) ) ;
#52991 = CARTESIAN_POINT ( 'NONE',  ( 26.39999999999999858, 0.000000000000000000, 4.999999999999998224 ) ) ;
#52992 =( BOUNDED_CURVE ( )  B_SPLINE_CURVE ( 2, ( #3687, #26211, #31388, #64998, #9584, #13651, #43210 ),
 .UNSPECIFIED., .F., .F. ) 
 B_SPLINE_CURVE_WITH_KNOTS ( ( 3, 2, 2, 3 ),
 ( 0.7333333333333332815, 0.7361111111111111605, 0.7388888888888889284, 0.7416666666666666963 ),
 .UNSPECIFIED. ) 
 CURVE ( )  GEOMETRIC_REPRESENTATION_ITEM ( )  RATIONAL_B_SPLINE_CURVE ( ( 1.000000000000000000, 0.8660254037844387076, 1.000000000000000000, 0.8660254037844387076, 1.000000000000000000, 0.8660254037844387076, 1.000000000000000000 ) ) 
 REPRESENTATION_ITEM ( '' )  );
#52993 = CARTESIAN_POINT ( 'NONE',  ( 4.415625000614518569, 3.027376345333613106, -5.243569643749998122 ) ) ;
#52994 = CARTESIAN_POINT ( 'NONE',  ( 10.28437500061451715, 6.421520780324663323E-16, -5.243569643749999010 ) ) ;
#52995 = CARTESIAN_POINT ( 'NONE',  ( 16.57500000122903216, 2.886751345948126879, 4.999999999999999112 ) ) ;
#52996 = CARTESIAN_POINT ( 'NONE',  ( 3.496875000614518836, -3.027376345333610441, -5.243569643749999898 ) ) ;
#52997 = CARTESIAN_POINT ( 'NONE',  ( 5.090625000614516615, -3.027376345333614438, 5.243569643749998122 ) ) ;
#52998 = CARTESIAN_POINT ( 'NONE',  ( -2.000000000000001776, 13.19374999877096677, 33.46410161513775705 ) ) ;
#52999 = CARTESIAN_POINT ( 'NONE',  ( 21.58125000122903359, -4.330127018922194537, 2.499999999999995559 ) ) ;
#53000 = CARTESIAN_POINT ( 'NONE',  ( 16.77187500061451786, 3.027376345333611329, 5.243569643749999010 ) ) ;
#53001 = CARTESIAN_POINT ( 'NONE',  ( 27.67499999999999716, 4.330127018922191873, 2.499999999999999556 ) ) ;
#53002 = ORIENTED_EDGE ( 'NONE', *, *, #26320, .F. ) ;
#53003 = CARTESIAN_POINT ( 'NONE',  ( 21.92812500061451431, 6.421520780324663323E-16, -5.243569643749999010 ) ) ;
#53004 = CARTESIAN_POINT ( 'NONE',  ( 10.19062500061451892, -3.027376345333610441, -5.243569643749999898 ) ) ;
#53005 = CARTESIAN_POINT ( 'NONE',  ( 25.80937500061451928, 0.000000000000000000, 5.243569643749999010 ) ) ;
#53006 = CARTESIAN_POINT ( 'NONE',  ( 10.60312500061451679, -4.541064518000417216, -2.621784821875001281 ) ) ;
#53007 = CARTESIAN_POINT ( 'NONE',  ( 7.968750001229034652, 2.886751345948126879, 4.999999999999998224 ) ) ;
#53008 = CARTESIAN_POINT ( 'NONE',  ( 9.375000001229036428, 2.886751345948126879, 4.999999999999999112 ) ) ;
#53009 = CARTESIAN_POINT ( 'NONE',  ( 25.04062500061451502, -3.027376345333610441, -5.243569643749999898 ) ) ;
#53010 = EDGE_CURVE ( 'NONE', #19466, #10804, #7811, .T. ) ;
#53011 = CARTESIAN_POINT ( 'NONE',  ( 4.243569643749999898, 10.57812500061451821, -30.00000000000000000 ) ) ;
#53012 = CARTESIAN_POINT ( 'NONE',  ( 11.70000000122903216, -2.886751345948129988, 4.999999999999997335 ) ) ;
#53013 = CARTESIAN_POINT ( 'NONE',  ( 22.60312500061451857, 0.000000000000000000, 5.243569643749999010 ) ) ;
#53014 = CARTESIAN_POINT ( 'NONE',  ( 18.51562500061451289, 3.027376345333611329, 5.243569643749999010 ) ) ;
#53015 = CARTESIAN_POINT ( 'NONE',  ( 5.821875000614519458, 3.027376345333612662, -5.243569643749998122 ) ) ;
#53016 = CARTESIAN_POINT ( 'NONE',  ( 17.69999999999999929, 4.330127018922192761, -2.499999999999997780 ) ) ;
#53017 = CARTESIAN_POINT ( 'NONE',  ( 13.95000000122903572, -2.886751345948129988, 4.999999999999997335 ) ) ;
#53018 = CARTESIAN_POINT ( 'NONE',  ( 11.31562500061451892, 3.027376345333611329, 5.243569643749999010 ) ) ;
#53019 = CARTESIAN_POINT ( 'NONE',  ( 14.42812500061451786, 4.541064518000418104, 2.621784821874999949 ) ) ;
#53020 = CARTESIAN_POINT ( 'NONE',  ( 24.15000000122903145, 5.773502691896255534, 3.535250795749688894E-16 ) ) ;
#53021 = CARTESIAN_POINT ( 'NONE',  ( 22.24687500061451217, -3.027376345333614438, 5.243569643749998122 ) ) ;
#53022 = CARTESIAN_POINT ( 'NONE',  ( 21.49687500061451573, -3.027376345333610441, -5.243569643749999898 ) ) ;
#53023 = CARTESIAN_POINT ( 'NONE',  ( 25.31249999999999645, 2.886751345948101122, -5.000000000000046185 ) ) ;
#53024 = CARTESIAN_POINT ( 'NONE',  ( 7.575000001229033053, 2.886751345948126879, 4.999999999999999112 ) ) ;
#53025 = CARTESIAN_POINT ( 'NONE',  ( 6.871875000614517504, 3.027376345333611329, 5.243569643749999010 ) ) ;
#53026 = CARTESIAN_POINT ( 'NONE',  ( 25.35937500061451644, 0.000000000000000000, 5.243569643749999010 ) ) ;
#53027 = CARTESIAN_POINT ( 'NONE',  ( 5.000000000000000000, 6.123233995736766282E-16, 50.00000000000000000 ) ) ;
#53028 = CARTESIAN_POINT ( 'NONE',  ( 20.46562500061451928, -6.054752690667223547, -1.112240025338166033E-15 ) ) ;
#53029 = CARTESIAN_POINT ( 'NONE',  ( 25.73437500061451644, 4.541064518000418104, 2.621784821874999949 ) ) ;
#53030 = CARTESIAN_POINT ( 'NONE',  ( 3.756430356249998770, 17.21562499938548285, 32.16877607737301759 ) ) ;
#53031 = CARTESIAN_POINT ( 'NONE',  ( -0.7368881354385758975, 9.803648613939513368, 25.82089971438751519 ) ) ;
#53032 = CARTESIAN_POINT ( 'NONE',  ( 6.046875000614519102, -3.027376345333614438, 5.243569643749998122 ) ) ;
#53033 = CARTESIAN_POINT ( 'NONE',  ( 16.64062500061451289, 6.054752690667223547, 3.707466751127219781E-16 ) ) ;
#53034 = ORIENTED_EDGE ( 'NONE', *, *, #39683, .T. ) ;
#53035 = CARTESIAN_POINT ( 'NONE',  ( 45.00000000000000000, -7.332543590861054561, 5.218601775200177428 ) ) ;
#53036 = CARTESIAN_POINT ( 'NONE',  ( 25.45312500061451644, -4.541064518000417216, -2.621784821875001281 ) ) ;
#53037 = CARTESIAN_POINT ( 'NONE',  ( 3.459375000614519635, -4.541064518000417216, -2.621784821875001281 ) ) ;
#53038 = CARTESIAN_POINT ( 'NONE',  ( 45.00000000000000000, 0.000000000000000000, 0.000000000000000000 ) ) ;
#53039 = CARTESIAN_POINT ( 'NONE',  ( 0.000000000000000000, 20.00000000000000000, 30.00000000000000000 ) ) ;
#53040 = CARTESIAN_POINT ( 'NONE',  ( 16.98750000000000426, -2.886751345948129988, 4.999999999999997335 ) ) ;
#53041 = CARTESIAN_POINT ( 'NONE',  ( 20.09062500061451573, -3.027376345333610441, -5.243569643749999898 ) ) ;
#53042 = VERTEX_POINT ( 'NONE', #26232 ) ;
#53043 = CARTESIAN_POINT ( 'NONE',  ( 23.77499999999999858, -4.330127018922194537, 2.499999999999995559 ) ) ;
#53044 = CARTESIAN_POINT ( 'NONE',  ( 25.13437500061451502, 6.421520780324663323E-16, -5.243569643749999010 ) ) ;
#53045 = EDGE_CURVE ( 'NONE', #48156, #52599, #30900, .T. ) ;
#53046 = ORIENTED_EDGE ( 'NONE', *, *, #19843, .T. ) ;
#53047 = DIRECTION ( 'NONE',  ( -0.000000000000000000, -1.000000000000000000, -0.000000000000000000 ) ) ;
#53048 = CARTESIAN_POINT ( 'NONE',  ( 13.67812500061451786, -4.541064518000419881, 2.621784821874995952 ) ) ;
#53049 = CARTESIAN_POINT ( 'NONE',  ( 6.065625000614516260, -6.054752690667223547, -1.112240025338166033E-15 ) ) ;
#53050 = CARTESIAN_POINT ( 'NONE',  ( 16.28437500061451715, -2.746126346562646425, 4.756430356249996549 ) ) ;
#53051 = CARTESIAN_POINT ( 'NONE',  ( 28.56562500061451715, -6.054752690667223547, -1.112240025338166033E-15 ) ) ;
#53052 = CARTESIAN_POINT ( 'NONE',  ( 15.56250000122903465, 4.330127018922192761, -2.499999999999997780 ) ) ;
#53053 = CARTESIAN_POINT ( 'NONE',  ( 19.12500000000000000, 4.330127018922191873, 2.499999999999999556 ) ) ;
#53054 = CARTESIAN_POINT ( 'NONE',  ( 26.66250000000000142, 2.886751345948129099, -4.999999999999998224 ) ) ;
#53055 = CARTESIAN_POINT ( 'NONE',  ( 3.196875000614516793, 6.054752690667223547, 3.707466751127219781E-16 ) ) ;
#53056 = CARTESIAN_POINT ( 'NONE',  ( 8.446875000614518569, -3.027376345333610441, -5.243569643749999898 ) ) ;
#53057 = CARTESIAN_POINT ( 'NONE',  ( 20.18437500061451573, 6.421520780324663323E-16, -5.243569643749999010 ) ) ;
#53058 = CARTESIAN_POINT ( 'NONE',  ( 65.00000000000000000, -1.494782592887582195, 8.875000000000012434 ) ) ;
#53059 = ORIENTED_EDGE ( 'NONE', *, *, #7959, .F. ) ;
#53060 = CARTESIAN_POINT ( 'NONE',  ( 28.07812500061451289, -4.541064518000419881, 2.621784821874995952 ) ) ;
#53061 = CARTESIAN_POINT ( 'NONE',  ( 4.387500000000002842, -2.886751345948129988, 4.999999999999997335 ) ) ;
#53062 = CARTESIAN_POINT ( 'NONE',  ( 4.734375000614518214, -4.541064518000419881, 2.621784821874995952 ) ) ;
#53063 = CARTESIAN_POINT ( 'NONE',  ( 15.71250000000000213, -5.773502691896255534, -1.060575238724906372E-15 ) ) ;
#53064 = CARTESIAN_POINT ( 'NONE',  ( 13.56562500061451892, 3.027376345333611329, 5.243569643749999010 ) ) ;
#53065 = LINE ( 'NONE', #13904, #28929 ) ;
#53066 = CARTESIAN_POINT ( 'NONE',  ( 45.00000000000000000, 0.000000000000000000, 0.000000000000000000 ) ) ;
#53067 = CARTESIAN_POINT ( 'NONE',  ( 18.26250000122903216, 4.330127018922192761, -2.499999999999997780 ) ) ;
#53068 = CARTESIAN_POINT ( 'NONE',  ( 28.03125000122903288, 6.123233995736764310E-16, -4.999999999999998224 ) ) ;
#53069 = CARTESIAN_POINT ( 'NONE',  ( 18.27187500061451431, -5.492252693125287522, -1.008910452111647106E-15 ) ) ;
#53070 = CARTESIAN_POINT ( 'NONE',  ( 8.390625000614518214, -3.027376345333610441, -5.243569643749999898 ) ) ;
#53071 = CARTESIAN_POINT ( 'NONE',  ( 24.23437500061451644, 6.421520780324663323E-16, -5.243569643749999010 ) ) ;
#53072 = CARTESIAN_POINT ( 'NONE',  ( 19.72500000122903074, 2.886751345948126879, 4.999999999999998224 ) ) ;
#53073 = CARTESIAN_POINT ( 'NONE',  ( 23.22187500061451715, -6.054752690667223547, -1.112240025338166033E-15 ) ) ;
#53074 = CARTESIAN_POINT ( 'NONE',  ( 6.375000000000001776, 6.123233995736764310E-16, -4.999999999999998224 ) ) ;
#53075 = CARTESIAN_POINT ( 'NONE',  ( -2.000000000000000000, 10.13750000122903572, 26.53589838486224650 ) ) ;
#53076 = CARTESIAN_POINT ( 'NONE',  ( 13.60312500061451679, 0.000000000000000000, 5.243569643749999010 ) ) ;
#53077 = CARTESIAN_POINT ( 'NONE',  ( 7.725000001229034297, -5.773502691896255534, -1.060575238724906372E-15 ) ) ;
#53078 = CARTESIAN_POINT ( 'NONE',  ( 8.221875000614518925, 3.027376345333611329, 5.243569643749999010 ) ) ;
#53079 = CARTESIAN_POINT ( 'NONE',  ( 3.882888313307707229, -3.150174730667082201, 4.026983590546891811 ) ) ;
#53080 = ORIENTED_EDGE ( 'NONE', *, *, #21079, .T. ) ;
#53081 = CARTESIAN_POINT ( 'NONE',  ( 13.26562500061451644, -6.054752690667223547, -1.112240025338166033E-15 ) ) ;
#53082 = CARTESIAN_POINT ( 'NONE',  ( 3.439498972087754236, -3.629028357702141161, -3.784861396121385724 ) ) ;
#53083 = CARTESIAN_POINT ( 'NONE',  ( 22.87500000122903288, 2.886751345948126879, 4.999999999999999112 ) ) ;
#53084 = CARTESIAN_POINT ( 'NONE',  ( 9.984375000614518214, 4.541064518000418104, 2.621784821874999949 ) ) ;
#53085 = CARTESIAN_POINT ( 'NONE',  ( 15.47812500061451679, -4.541064518000419881, 2.621784821874995952 ) ) ;
#53086 = EDGE_CURVE ( 'NONE', #66635, #13629, #60539, .T. ) ;
#53087 = CARTESIAN_POINT ( 'NONE',  ( 27.69375000122902719, 5.773502691896255534, 3.535250795749688894E-16 ) ) ;
#53088 = CARTESIAN_POINT ( 'NONE',  ( 23.89687500061451786, 6.054752690667223547, 3.707466751127219781E-16 ) ) ;
#53089 = DIRECTION ( 'NONE',  ( 0.000000000000000000, 0.000000000000000000, -1.000000000000000000 ) ) ;
#53090 = CARTESIAN_POINT ( 'NONE',  ( 19.20000000000000284, 0.000000000000000000, 4.999999999999998224 ) ) ;
#53091 = CARTESIAN_POINT ( 'NONE',  ( -4.243569643749998122, 14.49687500061451750, -27.54997392385601174 ) ) ;
#53092 = CARTESIAN_POINT ( 'NONE',  ( 15.83437500061451608, 4.541064518000418104, 2.621784821874999949 ) ) ;
#53093 = CARTESIAN_POINT ( 'NONE',  ( 17.70000000122903216, -2.886751345948125991, -5.000000000000000000 ) ) ;
#53094 = CARTESIAN_POINT ( 'NONE',  ( 11.85937500061451644, 0.000000000000000000, 5.243569643749999010 ) ) ;
#53095 = CARTESIAN_POINT ( 'NONE',  ( -2.121784821874996840, 17.62812500061451715, -26.32496088578401583 ) ) ;
#53096 = CARTESIAN_POINT ( 'NONE',  ( 18.82500000122903216, 2.886751345948126879, 4.999999999999999112 ) ) ;
#53097 = CARTESIAN_POINT ( 'NONE',  ( 12.47812500061451502, 6.421520780324663323E-16, -5.243569643749999010 ) ) ;
#53098 = ORIENTED_EDGE ( 'NONE', *, *, #47219, .T. ) ;
#53099 = ORIENTED_EDGE ( 'NONE', *, *, #25113, .T. ) ;
#53100 = CARTESIAN_POINT ( 'NONE',  ( 18.78749999999999432, -2.886751345948129988, 4.999999999999997335 ) ) ;
#53101 = CARTESIAN_POINT ( 'NONE',  ( -5.000000000000000000, 0.000000000000000000, 50.00000000000000000 ) ) ;
#53102 = CARTESIAN_POINT ( 'NONE',  ( 13.47187500061451537, 3.027376345333612662, -5.243569643749998122 ) ) ;
#53103 = CARTESIAN_POINT ( 'NONE',  ( 22.57499999999999929, 6.123233995736764310E-16, -4.999999999999998224 ) ) ;
#53104 = CARTESIAN_POINT ( 'NONE',  ( 13.61250000122903359, -4.330127018922190985, -2.500000000000001332 ) ) ;
#53105 = CARTESIAN_POINT ( 'NONE',  ( 21.26250000122903572, -4.330127018922190985, -2.500000000000001332 ) ) ;
#53106 = CARTESIAN_POINT ( 'NONE',  ( 16.49062500061451786, -3.027376345333610441, -5.243569643749999898 ) ) ;
#53107 = CARTESIAN_POINT ( 'NONE',  ( 20.76562500061451644, 3.027376345333611329, 5.243569643749999010 ) ) ;
#53108 = CARTESIAN_POINT ( 'NONE',  ( 27.11250000122903359, -4.330127018922190985, -2.500000000000001332 ) ) ;
#53109 = CARTESIAN_POINT ( 'NONE',  ( 28.31250000000000000, -5.773502691896255534, -1.060575238724906372E-15 ) ) ;
#53110 = CARTESIAN_POINT ( 'NONE',  ( -3.756430356250000102, 12.86562499938548321, 30.00000000000000000 ) ) ;
#53111 = CARTESIAN_POINT ( 'NONE',  ( 7.771875000614516971, 2.746126346562643317, 4.756430356249998326 ) ) ;
#53112 = CARTESIAN_POINT ( 'NONE',  ( 27.08437500061451786, 4.541064518000418104, 2.621784821874999949 ) ) ;
#53113 = FACE_OUTER_BOUND ( 'NONE', #52801, .T. ) ;
#53114 = CARTESIAN_POINT ( 'NONE',  ( -4.243569643749999898, 16.25937500061451857, -30.00000000000000000 ) ) ;
#53115 = CARTESIAN_POINT ( 'NONE',  ( 4.500000001229034652, -2.886751345948129988, 4.999999999999997335 ) ) ;
#53116 = CARTESIAN_POINT ( 'NONE',  ( 6.187500000000002665, -2.886751345948129988, 4.999999999999997335 ) ) ;
#53117 =( BOUNDED_SURFACE ( )  B_SPLINE_SURFACE ( 1, 2, ( 
 ( #27485, #61091, #26382, #15648, #26015, #15286, #65165, #48923, #4952, #43382, #71081, #71454, #37465, #60713, #37091, #32656, #49289, #59615, #70710, #65537, #20455, #26757, #55556, #3497, #32288, #48554, #20084, #66642, #16019, #38567, #14923, #55197, #4591, #10490, #43008, #27120, #9029, #49654, #54822, #59984, #72182, #21561, #33017, #9395, #44115, #31560, #42641, #4230, #60345, #37826, #31925, #20828, #71822, #21194, #43745, #39665, #45200, #57352, #68453, #5312, #68099, #33381, #40024, #33742, #50742, #23009, #55917, #11216, #16743, #27854, #16380, #56637, #17105, #22651, #56988, #72543, #62184, #67019, #45568, #38935, #67731, #34824, #6757, #61813, #11935, #62538, #50019, #145, #34097, #61453, #44845, #10847, #6033, #50386, #56287, #11581, #28567, #72911, #5677, #22293, #21931, #28926, #12289, #44486, #51463, #34460, #28213, #51103, #499, #17465, #67381, #39298, #6394, #866, #23373, #45921, #62895, #17815, #40376, #35187, #7117, #53266, #63981, #7840, #14099, #8205, #29646, #12652, #2664, #24095, #52184, #18544, #47366, #41817, #1586, #52545, #13009, #59161, #19634, #58066, #24819, #57712, #24459, #23730, #35547, #36639, #1952, #46643, #30002, #69184, #69897, #46279, #19263, #30377, #68819, #29291, #41109, #63619, #58429, #51821, #7476, #41462, #47007, #1224, #25181, #47724, #70263, #64348, #13739, #63260, #40744, #13363, #69542, #18901, #36281, #35904, #52906, #58795, #2304, #30734, #42191, #18175, #64715, #65816, #25560, #37376, #71362, #48832, #20737, #44027, #8569, #43295, #15560, #38103, #60625, #14470, #14835, #55108, #4139, #26670, #31839, #48469, #66549, #65079, #21474, #70624, #70993, #19999, #37004, #42552, #60256, #25929, #4508, #15198, #49203, #37736, #59900, #3770, #9305, #10035, #59526, #31097, #9670, #8939, #32203, #53636, #54375, #66182, #48101, #31470, #71737, #21107, #54737, #26295, #27037, #3029, #72090, #49568, #54013, #43660, #32570, #15928, #38478, #20369, #3409, #42920, #65443, #51014, #11491, #67649, #11850, #45476, #44762, #45114, #50303, #61002, #777, #4863, #33653, #17015, #33296, #72825, #5221, #55834, #39213, #50656, #5944, #5591, #62097 ),
 ( #49929, #72454, #34369, #17732, #68009, #27399, #410, #56902, #22919, #28477, #45834, #67297, #28128, #62452, #56550, #38851, #39573, #60, #23285, #10401, #22566, #17381, #39939, #6307, #66928, #16655, #28835, #51374, #68371, #11126, #27763, #32933, #44402, #55471, #21838, #22208, #16297, #61366, #10763, #34013, #61725, #56198, #24373, #58342, #40653, #1867, #70174, #25097, #57262, #7392, #41023, #18459, #53181, #35459, #51738, #46193, #18092, #64261, #46921, #18817, #47641, #19180, #63173, #23648, #13648, #35102, #12568, #29561, #7752, #52821, #57627, #63539, #24008, #40291, #30649, #69097, #35820, #68734, #57982, #34733, #46556, #62813, #12925, #7031, #29920, #52098, #30289, #6675, #2223, #41380, #29203, #12205, #1503, #52460, #69459, #1138, #63891, #13281, #24736, #47280, #36192, #58710, #8121, #69814, #41733, #2578, #15472, #42473, #60173, #31014, #4052, #54292, #9218, #65358, #19919, #32114, #64996, #4421, #36556, #31755, #14748, #26950, #38016, #48018, #37650, #2943, #9582, #3320, #20282, #65727, #25472, #53925, #59442, #70544, #59076, #26209, #59813, #37290, #26578, #42108, #3685, #8480, #15113, #53547, #48748, #49476, #71272, #14386, #42836, #8849, #54648, #36921, #49118, #20650, #31385, #19551, #25846, #48383, #43207, #64631, #70910, #71646, #21019, #14017, #60538, #9945, #32483, #43572, #66093, #55016, #67922, #21748, #39482, #10313, #56467, #33562, #61635, #44676, #72368, #11406, #44309, #56814, #15840, #11037, #67207, #6221, #17294, #27310, #16928, #55382, #62005, #55743, #72734, #45028, #4776, #33204, #38762, #49843, #38386, #5501, #39120, #16568, #5858, #21383, #56111, #60909, #67563, #32845, #28040, #28749, #72008, #10674, #33925, #28390, #43939, #22121, #50569, #66838, #16209, #61281, #73096, #5137, #27672, #22478, #50928, #50210, #325, #22834, #66463, #45386, #34282, #39856, #62368, #11766, #6948, #41652, #51654, #12844, #8034, #36106, #68288, #18375, #52017, #29480, #64173, #46474, #62730, #57177, #29120, #2140, #35377, #29839, #58627, #30204, #1056, #34649, #24651, #46111, #23566, #40569, #69379, #63808, #68648, #1418, #35017, #51289, #13561, #23924, #46839 ) ),
 .UNSPECIFIED., .F., .F., .F. ) 
 B_SPLINE_SURFACE_WITH_KNOTS ( ( 2, 2 ),
 ( 3, 2, 2, 2, 2, 2, 2, 2, 2, 2, 2, 2, 2, 2, 2, 2, 2, 2, 2, 2, 2, 2, 2, 2, 2, 2, 2, 2, 2, 2, 2, 2, 2, 2, 2, 2, 2, 2, 2, 2, 2, 2, 2, 2, 2, 2, 2, 2, 2, 2, 2, 2, 2, 2, 2, 2, 2, 2, 2, 2, 2, 2, 2, 2, 2, 2, 2, 2, 2, 2, 2, 2, 2, 2, 2, 2, 2, 2, 2, 2, 2, 2, 2, 2, 2, 2, 2, 2, 2, 2, 2, 2, 2, 2, 2, 2, 2, 2, 2, 2, 2, 2, 2, 2, 2, 2, 2, 2, 2, 2, 2, 2, 2, 2, 2, 2, 2, 2, 2, 2, 2, 2, 2, 2, 2, 2, 2, 2, 2, 2, 2, 2, 2, 2, 3 ),
 ( 0.000000000000000000, 1.000000000000000000 ),
 ( 0.000000000000000000, 0.007246376811594202987, 0.01449275362318840597, 0.02173913043478260809, 0.02898550724637681195, 0.03623188405797101580, 0.04347826086956521618, 0.05072463768115942351, 0.05797101449275362389, 0.06521739130434782428, 0.07246376811594203160, 0.07971014492753622505, 0.08695652173913043237, 0.09420289855072463969, 0.1014492753623188470, 0.1086956521739130405, 0.1159420289855072478, 0.1231884057971014551, 0.1304347826086956486, 0.1376811594202898559, 0.1449275362318840632, 0.1521739130434782705, 0.1594202898550724501, 0.1666666666666666574, 0.1739130434782608647, 0.1811594202898550721, 0.1884057971014492794, 0.1956521739130434867, 0.2028985507246376940, 0.2101449275362318736, 0.2173913043478260809, 0.2246376811594202882, 0.2318840579710144956, 0.2391304347826087029, 0.2463768115942029102, 0.2536231884057971175, 0.2608695652173912971, 0.2681159420289855322, 0.2753623188405797118, 0.2826086956521738913, 0.2898550724637681264, 0.2971014492753623060, 0.3043478260869565410, 0.3115942028985507206, 0.3188405797101449002, 0.3260869565217391353, 0.3333333333333333148, 0.3405797101449275499, 0.3478260869565217295, 0.3550724637681159646, 0.3623188405797101441, 0.3695652173913043237, 0.3768115942028985588, 0.3840579710144927383, 0.3913043478260869734, 0.3985507246376811530, 0.4057971014492753881, 0.4130434782608695676, 0.4202898550724637472, 0.4275362318840579823, 0.4347826086956521618, 0.4420289855072463969, 0.4492753623188405765, 0.4565217391304347561, 0.4637681159420289911, 0.4710144927536231707, 0.4782608695652174058, 0.4855072463768115854, 0.4927536231884058204, 0.5000000000000000000, 0.5072463768115942351, 0.5144927536231883591, 0.5217391304347825942, 0.5289855072463768293, 0.5362318840579710644, 0.5434782608695651884, 0.5507246376811594235, 0.5579710144927536586, 0.5652173913043477826, 0.5724637681159420177, 0.5797101449275362528, 0.5869565217391304879, 0.5942028985507246119, 0.6014492753623188470, 0.6086956521739130821, 0.6159420289855072062, 0.6231884057971014412, 0.6304347826086956763, 0.6376811594202898004, 0.6449275362318840354, 0.6521739130434782705, 0.6594202898550725056, 0.6666666666666666297, 0.6739130434782608647, 0.6811594202898550998, 0.6884057971014492239, 0.6956521739130434590, 0.7028985507246376940, 0.7101449275362319291, 0.7173913043478260532, 0.7246376811594202882, 0.7318840579710145233, 0.7391304347826086474, 0.7463768115942028825, 0.7536231884057971175, 0.7608695652173913526, 0.7681159420289854767, 0.7753623188405797118, 0.7826086956521739468, 0.7898550724637680709, 0.7971014492753623060, 0.8043478260869565410, 0.8115942028985507761, 0.8188405797101449002, 0.8260869565217391353, 0.8333333333333333703, 0.8405797101449274944, 0.8478260869565217295, 0.8550724637681159646, 0.8623188405797101996, 0.8695652173913043237, 0.8768115942028985588, 0.8840579710144927938, 0.8913043478260869179, 0.8985507246376811530, 0.9057971014492753881, 0.9130434782608695121, 0.9202898550724637472, 0.9275362318840579823, 0.9347826086956522174, 0.9420289855072463414, 0.9492753623188405765, 0.9565217391304348116, 0.9637681159420289356, 0.9662083017040261623 ),
 .UNSPECIFIED. ) 
 GEOMETRIC_REPRESENTATION_ITEM ( )  RATIONAL_B_SPLINE_SURFACE ( (
 ( 1.000000000000000000, 0.8660254037844387076, 1.000000000000000000, 0.8660254037844387076, 1.000000000000000000, 0.8660254037844387076, 1.000000000000000000, 0.8660254037844387076, 1.000000000000000000, 0.8660254037844387076, 1.000000000000000000, 0.8660254037844387076, 1.000000000000000000, 0.8660254037844387076, 1.000000000000000000, 0.8660254037844387076, 1.000000000000000000, 0.8660254037844387076, 1.000000000000000000, 0.8660254037844387076, 1.000000000000000000, 0.8660254037844387076, 1.000000000000000000, 0.8660254037844387076, 1.000000000000000000, 0.8660254037844387076, 1.000000000000000000, 0.8660254037844387076, 1.000000000000000000, 0.8660254037844387076, 1.000000000000000000, 0.8660254037844387076, 1.000000000000000000, 0.8660254037844387076, 1.000000000000000000, 0.8660254037844387076, 1.000000000000000000, 0.8660254037844387076, 1.000000000000000000, 0.8660254037844387076, 1.000000000000000000, 0.8660254037844387076, 1.000000000000000000, 0.8660254037844387076, 1.000000000000000000, 0.8660254037844387076, 1.000000000000000000, 0.8660254037844387076, 1.000000000000000000, 0.8660254037844387076, 1.000000000000000000, 0.8660254037844387076, 1.000000000000000000, 0.8660254037844387076, 1.000000000000000000, 0.8660254037844387076, 1.000000000000000000, 0.8660254037844387076, 1.000000000000000000, 0.8660254037844387076, 1.000000000000000000, 0.8660254037844387076, 1.000000000000000000, 0.8660254037844387076, 1.000000000000000000, 0.8660254037844387076, 1.000000000000000000, 0.8660254037844387076, 1.000000000000000000, 0.8660254037844387076, 1.000000000000000000, 0.8660254037844387076, 1.000000000000000000, 0.8660254037844387076, 1.000000000000000000, 0.8660254037844387076, 1.000000000000000000, 0.8660254037844387076, 1.000000000000000000, 0.8660254037844387076, 1.000000000000000000, 0.8660254037844387076, 1.000000000000000000, 0.8660254037844387076, 1.000000000000000000, 0.8660254037844387076, 1.000000000000000000, 0.8660254037844387076, 1.000000000000000000, 0.8660254037844387076, 1.000000000000000000, 0.8660254037844387076, 1.000000000000000000, 0.8660254037844387076, 1.000000000000000000, 0.8660254037844387076, 1.000000000000000000, 0.8660254037844387076, 1.000000000000000000, 0.8660254037844387076, 1.000000000000000000, 0.8660254037844387076, 1.000000000000000000, 0.8660254037844387076, 1.000000000000000000, 0.8660254037844387076, 1.000000000000000000, 0.8660254037844387076, 1.000000000000000000, 0.8660254037844387076, 1.000000000000000000, 0.8660254037844387076, 1.000000000000000000, 0.8660254037844387076, 1.000000000000000000, 0.8660254037844387076, 1.000000000000000000, 0.8660254037844387076, 1.000000000000000000, 0.8660254037844387076, 1.000000000000000000, 0.8660254037844387076, 1.000000000000000000, 0.8660254037844387076, 1.000000000000000000, 0.8660254037844387076, 1.000000000000000000, 0.8660254037844387076, 1.000000000000000000, 0.8660254037844387076, 1.000000000000000000, 0.8660254037844387076, 1.000000000000000000, 0.8660254037844387076, 1.000000000000000000, 0.8660254037844387076, 1.000000000000000000, 0.8660254037844387076, 1.000000000000000000, 0.8660254037844387076, 1.000000000000000000, 0.8660254037844387076, 1.000000000000000000, 0.8660254037844387076, 1.000000000000000000, 0.8660254037844387076, 1.000000000000000000, 0.8660254037844387076, 1.000000000000000000, 0.8660254037844387076, 1.000000000000000000, 0.8660254037844387076, 1.000000000000000000, 0.8660254037844387076, 1.000000000000000000, 0.8660254037844387076, 1.000000000000000000, 0.8660254037844387076, 1.000000000000000000, 0.8660254037844387076, 1.000000000000000000, 0.8660254037844387076, 1.000000000000000000, 0.8660254037844387076, 1.000000000000000000, 0.8660254037844387076, 1.000000000000000000, 0.8660254037844387076, 1.000000000000000000, 0.8660254037844387076, 1.000000000000000000, 0.8660254037844387076, 1.000000000000000000, 0.8660254037844387076, 1.000000000000000000, 0.8660254037844387076, 1.000000000000000000, 0.8660254037844387076, 1.000000000000000000, 0.8660254037844387076, 1.000000000000000000, 0.8660254037844387076, 1.000000000000000000, 0.8660254037844387076, 1.000000000000000000, 0.8660254037844387076, 1.000000000000000000, 0.8660254037844387076, 1.000000000000000000, 0.8660254037844387076, 1.000000000000000000, 0.8660254037844387076, 1.000000000000000000, 0.8660254037844387076, 1.000000000000000000, 0.8660254037844387076, 1.000000000000000000, 0.8660254037844387076, 1.000000000000000000, 0.8660254037844387076, 1.000000000000000000, 0.8660254037844387076, 1.000000000000000000, 0.8660254037844387076, 1.000000000000000000, 0.8660254037844387076, 1.000000000000000000, 0.8660254037844387076, 1.000000000000000000, 0.8660254037844387076, 1.000000000000000000, 0.8660254037844387076, 1.000000000000000000, 0.8660254037844387076, 1.000000000000000000, 0.8660254037844387076, 1.000000000000000000, 0.8660254037844387076, 1.000000000000000000, 0.8660254037844387076, 1.000000000000000000, 0.8660254037844387076, 1.000000000000000000, 0.8660254037844387076, 1.000000000000000000, 0.8660254037844387076, 1.000000000000000000, 0.8660254037844387076, 1.000000000000000000, 0.8660254037844387076, 1.000000000000000000, 0.8660254037844387076, 1.000000000000000000, 0.8660254037844387076, 1.000000000000000000, 0.8660254037844387076, 1.000000000000000000, 0.8660254037844387076, 1.000000000000000000, 0.8660254037844387076, 1.000000000000000000, 0.8660254037844387076, 1.000000000000000000, 0.8660254037844387076, 1.000000000000000000, 0.8660254037844387076, 1.000000000000000000, 0.8660254037844387076, 1.000000000000000000, 0.8660254037844387076, 1.000000000000000000, 0.8660254037844387076, 1.000000000000000000, 0.8660254037844387076, 1.000000000000000000, 0.8660254037844387076, 1.000000000000000000, 0.8660254037844387076, 1.000000000000000000, 0.8660254037844387076, 1.000000000000000000, 0.8660254037844387076, 1.000000000000000000, 0.8660254037844387076, 1.000000000000000000, 0.8660254037844387076, 1.000000000000000000, 0.9548846395026737710, 0.9401540804572410259),
 ( 1.000000000000000000, 0.8660254037844387076, 1.000000000000000000, 0.8660254037844387076, 1.000000000000000000, 0.8660254037844387076, 1.000000000000000000, 0.8660254037844387076, 1.000000000000000000, 0.8660254037844387076, 1.000000000000000000, 0.8660254037844387076, 1.000000000000000000, 0.8660254037844387076, 1.000000000000000000, 0.8660254037844387076, 1.000000000000000000, 0.8660254037844387076, 1.000000000000000000, 0.8660254037844387076, 1.000000000000000000, 0.8660254037844387076, 1.000000000000000000, 0.8660254037844387076, 1.000000000000000000, 0.8660254037844387076, 1.000000000000000000, 0.8660254037844387076, 1.000000000000000000, 0.8660254037844387076, 1.000000000000000000, 0.8660254037844387076, 1.000000000000000000, 0.8660254037844387076, 1.000000000000000000, 0.8660254037844387076, 1.000000000000000000, 0.8660254037844387076, 1.000000000000000000, 0.8660254037844387076, 1.000000000000000000, 0.8660254037844387076, 1.000000000000000000, 0.8660254037844387076, 1.000000000000000000, 0.8660254037844387076, 1.000000000000000000, 0.8660254037844387076, 1.000000000000000000, 0.8660254037844387076, 1.000000000000000000, 0.8660254037844387076, 1.000000000000000000, 0.8660254037844387076, 1.000000000000000000, 0.8660254037844387076, 1.000000000000000000, 0.8660254037844387076, 1.000000000000000000, 0.8660254037844387076, 1.000000000000000000, 0.8660254037844387076, 1.000000000000000000, 0.8660254037844387076, 1.000000000000000000, 0.8660254037844387076, 1.000000000000000000, 0.8660254037844387076, 1.000000000000000000, 0.8660254037844387076, 1.000000000000000000, 0.8660254037844387076, 1.000000000000000000, 0.8660254037844387076, 1.000000000000000000, 0.8660254037844387076, 1.000000000000000000, 0.8660254037844387076, 1.000000000000000000, 0.8660254037844387076, 1.000000000000000000, 0.8660254037844387076, 1.000000000000000000, 0.8660254037844387076, 1.000000000000000000, 0.8660254037844387076, 1.000000000000000000, 0.8660254037844387076, 1.000000000000000000, 0.8660254037844387076, 1.000000000000000000, 0.8660254037844387076, 1.000000000000000000, 0.8660254037844387076, 1.000000000000000000, 0.8660254037844387076, 1.000000000000000000, 0.8660254037844387076, 1.000000000000000000, 0.8660254037844387076, 1.000000000000000000, 0.8660254037844387076, 1.000000000000000000, 0.8660254037844387076, 1.000000000000000000, 0.8660254037844387076, 1.000000000000000000, 0.8660254037844387076, 1.000000000000000000, 0.8660254037844387076, 1.000000000000000000, 0.8660254037844387076, 1.000000000000000000, 0.8660254037844387076, 1.000000000000000000, 0.8660254037844387076, 1.000000000000000000, 0.8660254037844387076, 1.000000000000000000, 0.8660254037844387076, 1.000000000000000000, 0.8660254037844387076, 1.000000000000000000, 0.8660254037844387076, 1.000000000000000000, 0.8660254037844387076, 1.000000000000000000, 0.8660254037844387076, 1.000000000000000000, 0.8660254037844387076, 1.000000000000000000, 0.8660254037844387076, 1.000000000000000000, 0.8660254037844387076, 1.000000000000000000, 0.8660254037844387076, 1.000000000000000000, 0.8660254037844387076, 1.000000000000000000, 0.8660254037844387076, 1.000000000000000000, 0.8660254037844387076, 1.000000000000000000, 0.8660254037844387076, 1.000000000000000000, 0.8660254037844387076, 1.000000000000000000, 0.8660254037844387076, 1.000000000000000000, 0.8660254037844387076, 1.000000000000000000, 0.8660254037844387076, 1.000000000000000000, 0.8660254037844387076, 1.000000000000000000, 0.8660254037844387076, 1.000000000000000000, 0.8660254037844387076, 1.000000000000000000, 0.8660254037844387076, 1.000000000000000000, 0.8660254037844387076, 1.000000000000000000, 0.8660254037844387076, 1.000000000000000000, 0.8660254037844387076, 1.000000000000000000, 0.8660254037844387076, 1.000000000000000000, 0.8660254037844387076, 1.000000000000000000, 0.8660254037844387076, 1.000000000000000000, 0.8660254037844387076, 1.000000000000000000, 0.8660254037844387076, 1.000000000000000000, 0.8660254037844387076, 1.000000000000000000, 0.8660254037844387076, 1.000000000000000000, 0.8660254037844387076, 1.000000000000000000, 0.8660254037844387076, 1.000000000000000000, 0.8660254037844387076, 1.000000000000000000, 0.8660254037844387076, 1.000000000000000000, 0.8660254037844387076, 1.000000000000000000, 0.8660254037844387076, 1.000000000000000000, 0.8660254037844387076, 1.000000000000000000, 0.8660254037844387076, 1.000000000000000000, 0.8660254037844387076, 1.000000000000000000, 0.8660254037844387076, 1.000000000000000000, 0.8660254037844387076, 1.000000000000000000, 0.8660254037844387076, 1.000000000000000000, 0.8660254037844387076, 1.000000000000000000, 0.8660254037844387076, 1.000000000000000000, 0.8660254037844387076, 1.000000000000000000, 0.8660254037844387076, 1.000000000000000000, 0.8660254037844387076, 1.000000000000000000, 0.8660254037844387076, 1.000000000000000000, 0.8660254037844387076, 1.000000000000000000, 0.8660254037844387076, 1.000000000000000000, 0.8660254037844387076, 1.000000000000000000, 0.8660254037844387076, 1.000000000000000000, 0.8660254037844387076, 1.000000000000000000, 0.8660254037844387076, 1.000000000000000000, 0.8660254037844387076, 1.000000000000000000, 0.8660254037844387076, 1.000000000000000000, 0.8660254037844387076, 1.000000000000000000, 0.8660254037844387076, 1.000000000000000000, 0.8660254037844387076, 1.000000000000000000, 0.8660254037844387076, 1.000000000000000000, 0.8660254037844387076, 1.000000000000000000, 0.8660254037844387076, 1.000000000000000000, 0.8660254037844387076, 1.000000000000000000, 0.8660254037844387076, 1.000000000000000000, 0.8660254037844387076, 1.000000000000000000, 0.8660254037844387076, 1.000000000000000000, 0.8660254037844387076, 1.000000000000000000, 0.8660254037844387076, 1.000000000000000000, 0.8660254037844387076, 1.000000000000000000, 0.8660254037844387076, 1.000000000000000000, 0.8660254037844387076, 1.000000000000000000, 0.8660254037844387076, 1.000000000000000000, 0.8660254037844387076, 1.000000000000000000, 0.9548846395026737710, 0.9401540804572410259) ) ) 
 REPRESENTATION_ITEM ( '' )  SURFACE ( )  );
#53118 = CARTESIAN_POINT ( 'NONE',  ( 27.41250000000000142, -5.773502691896255534, -1.060575238724906372E-15 ) ) ;
#53119 = CARTESIAN_POINT ( 'NONE',  ( 9.309375000614517504, -4.541064518000417216, -2.621784821875001281 ) ) ;
#53120 = CARTESIAN_POINT ( 'NONE',  ( 27.59062500061451573, -3.027376345333614438, 5.243569643749998122 ) ) ;
#53121 = FACE_OUTER_BOUND ( 'NONE', #42025, .T. ) ;
#53122 = CARTESIAN_POINT ( 'NONE',  ( -2.698377630233219193, 9.636255672932172445, -35.37338662132845712 ) ) ;
#53123 = CARTESIAN_POINT ( 'NONE',  ( 20.78732959644809952, 2.500000000000000444, 5.500000000000000000 ) ) ;
#53124 = CARTESIAN_POINT ( 'NONE',  ( 6.759375000614516793, 4.541064518000418104, -2.621784821874998173 ) ) ;
#53125 = CARTESIAN_POINT ( 'NONE',  ( 11.67187500061451821, 3.027376345333613106, -5.243569643749998122 ) ) ;
#53126 = CARTESIAN_POINT ( 'NONE',  ( 3.937500000000000444, -2.886751345948129988, 4.999999999999997335 ) ) ;
#53127 = CARTESIAN_POINT ( 'NONE',  ( 9.001249775931846008E-16, 14.06562500061459886, 34.90005215228797653 ) ) ;
#53128 = CARTESIAN_POINT ( 'NONE',  ( 1.592000809091587073E-14, 16.73750000000000071, -34.00000000000000000 ) ) ;
#53129 = CARTESIAN_POINT ( 'NONE',  ( 5.962500000000002132, 2.886751345948129099, -4.999999999999998224 ) ) ;
#53130 = EDGE_CURVE ( 'NONE', #71973, #12632, #70932, .T. ) ;
#53131 = CARTESIAN_POINT ( 'NONE',  ( 14.29687500061451644, 4.119189519843966529, -2.378215178124998275 ) ) ;
#53132 = CARTESIAN_POINT ( 'NONE',  ( 20.05312500061451431, -4.541064518000417216, -2.621784821875001281 ) ) ;
#53133 = CARTESIAN_POINT ( 'NONE',  ( 13.56562500061451892, 3.027376345333611329, 5.243569643749999010 ) ) ;
#53134 = CARTESIAN_POINT ( 'NONE',  ( 23.85937500061451644, 2.746126346562643317, 4.756430356249998326 ) ) ;
#53135 = CARTESIAN_POINT ( 'NONE',  ( 9.909375000614517148, 4.541064518000418104, -2.621784821874998173 ) ) ;
#53136 = CARTESIAN_POINT ( 'NONE',  ( 25.38749999999999929, 5.773502691896255534, 3.535250795749688894E-16 ) ) ;
#53137 = CARTESIAN_POINT ( 'NONE',  ( 22.42500000122903359, 2.886751345948126879, 4.999999999999999112 ) ) ;
#53138 = CARTESIAN_POINT ( 'NONE',  ( 24.14999999999999858, 0.000000000000000000, 4.999999999999998224 ) ) ;
#53139 = CARTESIAN_POINT ( 'NONE',  ( 9.121875000614517504, 3.027376345333611329, 5.243569643749999010 ) ) ;
#53140 = CARTESIAN_POINT ( 'NONE',  ( 27.75937500061451502, -4.541064518000417216, -2.621784821875001281 ) ) ;
#53141 = EDGE_CURVE ( 'NONE', #41179, #22787, #43652, .T. ) ;
#53142 = DIRECTION ( 'NONE',  ( -1.000000000000000000, -0.000000000000000000, -0.000000000000000000 ) ) ;
#53143 = LINE ( 'NONE', #69423, #34860 ) ;
#53144 = CARTESIAN_POINT ( 'NONE',  ( 19.35937500061451644, 4.541064518000418104, -2.621784821874998173 ) ) ;
#53145 = CARTESIAN_POINT ( 'NONE',  ( 10.92187500061451644, 3.027376345333611329, 5.243569643749999010 ) ) ;
#53146 = CARTESIAN_POINT ( 'NONE',  ( -3.756430356250001434, 20.66562499938548569, 32.16877607737301048 ) ) ;
#53147 = CARTESIAN_POINT ( 'NONE',  ( 22.31250000000000000, 2.886751345948126879, 4.999999999999999112 ) ) ;
#53148 = CARTESIAN_POINT ( 'NONE',  ( 2.828200636599751609E-16, 13.06250000000000355, 25.38119784648299415 ) ) ;
#53149 = CARTESIAN_POINT ( 'NONE',  ( 9.001249775931846008E-16, 13.22187500061451715, -25.09994784771203058 ) ) ;
#53150 = CARTESIAN_POINT ( 'NONE',  ( 23.82187500061451502, 2.746126346562645981, -4.756430356249997438 ) ) ;
#53151 = CARTESIAN_POINT ( 'NONE',  ( 14.80312500061451608, 4.541064518000418104, -2.621784821874998173 ) ) ;
#53152 = CARTESIAN_POINT ( 'NONE',  ( 4.425000000000001599, -4.330127018922194537, 2.499999999999995559 ) ) ;
#53153 = ADVANCED_FACE ( 'NONE', ( #60560 ), #15791, .T. ) ;
#53154 = CARTESIAN_POINT ( 'NONE',  ( 25.19999999999999929, -4.330127018922190985, -2.500000000000001332 ) ) ;
#53155 = LINE ( 'NONE', #2553, #1997 ) ;
#53156 = CARTESIAN_POINT ( 'NONE',  ( 13.61250000000000071, 2.886751345948129099, -4.999999999999998224 ) ) ;
#53157 = CARTESIAN_POINT ( 'NONE',  ( 4.243569643749999898, 10.54062500061451679, 32.45002607614398471 ) ) ;
#53158 = CARTESIAN_POINT ( 'NONE',  ( 14.73750000122903359, 4.330127018922191873, 2.499999999999999556 ) ) ;
#53159 = CARTESIAN_POINT ( 'NONE',  ( 24.90937500061451715, 0.000000000000000000, 5.243569643749999010 ) ) ;
#53160 = CARTESIAN_POINT ( 'NONE',  ( 7.256250001229033408, -4.330127018922190985, -2.500000000000001332 ) ) ;
#53161 = ORIENTED_EDGE ( 'NONE', *, *, #61105, .T. ) ;
#53162 = CARTESIAN_POINT ( 'NONE',  ( 18.85312500061451502, 4.541064518000418104, -2.621784821874998173 ) ) ;
#53163 = CARTESIAN_POINT ( 'NONE',  ( 3.178125000614515638, 4.541064518000418104, 2.621784821874999949 ) ) ;
#53164 = CARTESIAN_POINT ( 'NONE',  ( 20.78437500061451715, 4.541064518000418104, 2.621784821874999949 ) ) ;
#53165 = CARTESIAN_POINT ( 'NONE',  ( 29.40937500061451715, 0.000000000000000000, 5.243569643749999010 ) ) ;
#53166 = CARTESIAN_POINT ( 'NONE',  ( 4.040625000614517681, 6.054752690667223547, 3.707466751127219781E-16 ) ) ;
#53167 = CARTESIAN_POINT ( 'NONE',  ( 21.59062500061451928, 6.054752690667223547, 3.707466751127219781E-16 ) ) ;
#53168 = CARTESIAN_POINT ( 'NONE',  ( 2.121784821875001281, 16.35312500061451857, 33.67503911421598417 ) ) ;
#53169 = CARTESIAN_POINT ( 'NONE',  ( 15.86250000122903181, -4.330127018922190985, -2.500000000000001332 ) ) ;
#53170 = CARTESIAN_POINT ( 'NONE',  ( 12.38437500061451857, -4.119189519843968306, 2.378215178124996054 ) ) ;
#53171 = CARTESIAN_POINT ( 'NONE',  ( 7.678125000614516082, 4.541064518000418104, 2.621784821874999949 ) ) ;
#53172 = CARTESIAN_POINT ( 'NONE',  ( 3.159375000614518036, 4.541064518000418104, -2.621784821874998173 ) ) ;
#53173 = CARTESIAN_POINT ( 'NONE',  ( 2.971875000614517592, -6.054752690667223547, -1.112240025338166033E-15 ) ) ;
#53174 = CARTESIAN_POINT ( 'NONE',  ( 23.07187500061451857, 3.027376345333611329, 5.243569643749999010 ) ) ;
#53175 = CARTESIAN_POINT ( 'NONE',  ( 14.27812500061451573, 6.421520780324663323E-16, -5.243569643749999010 ) ) ;
#53176 = CARTESIAN_POINT ( 'NONE',  ( 25.72500000122903074, -5.773502691896255534, -1.060575238724906372E-15 ) ) ;
#53177 =( BOUNDED_CURVE ( )  B_SPLINE_CURVE ( 2, ( #15157, #60217, #60586, #32890, #61324, #27720, #54337 ),
 .UNSPECIFIED., .F., .F. ) 
 B_SPLINE_CURVE_WITH_KNOTS ( ( 3, 2, 2, 3 ),
 ( 0.5500000000000000444, 0.5527777777777778123, 0.5555555555555555802, 0.5583333333333333481 ),
 .UNSPECIFIED. ) 
 CURVE ( )  GEOMETRIC_REPRESENTATION_ITEM ( )  RATIONAL_B_SPLINE_CURVE ( ( 1.000000000000000000, 0.8660254037844387076, 1.000000000000000000, 0.8660254037844387076, 1.000000000000000000, 0.8660254037844387076, 1.000000000000000000 ) ) 
 REPRESENTATION_ITEM ( '' )  );
#53178 = CARTESIAN_POINT ( 'NONE',  ( 24.77812500061451217, 4.541064518000418104, 2.621784821874999949 ) ) ;
#53179 = CARTESIAN_POINT ( 'NONE',  ( 19.80937500061451573, 4.541064518000418104, -2.621784821874998173 ) ) ;
#53180 = CARTESIAN_POINT ( 'NONE',  ( 13.94062500061451892, 6.054752690667223547, 3.707466751127219781E-16 ) ) ;
#53181 = CARTESIAN_POINT ( 'NONE',  ( 2.121784821874999061, 17.90937500061451715, 26.32496088578401583 ) ) ;
#53182 = CARTESIAN_POINT ( 'NONE',  ( 19.19062500061452070, -3.027376345333610441, -5.243569643749999898 ) ) ;
#53183 = CARTESIAN_POINT ( 'NONE',  ( 5.810221930991193690E-16, 17.56250000000000000, 26.00000000000000000 ) ) ;
#53184 = EDGE_LOOP ( 'NONE', ( #38928, #12990, #18227, #32848 ) ) ;
#53185 = CARTESIAN_POINT ( 'NONE',  ( 24.18750000000000355, -2.886751345948129988, 4.999999999999997335 ) ) ;
#53186 = CARTESIAN_POINT ( 'NONE',  ( -4.243569643749999898, 19.85937500061451644, -30.00000000000000000 ) ) ;
#53187 = CARTESIAN_POINT ( 'NONE',  ( 1.878215178124997609, 19.42812499938548143, 33.25316411605952993 ) ) ;
#53188 = CARTESIAN_POINT ( 'NONE',  ( 26.87812500061451360, 6.421520780324663323E-16, -5.243569643749999010 ) ) ;
#53189 = CARTESIAN_POINT ( 'NONE',  ( 8.990625000614516082, 6.054752690667223547, 3.707466751127219781E-16 ) ) ;
#53190 = CARTESIAN_POINT ( 'NONE',  ( 20.81250000122903643, -4.330127018922190985, -2.500000000000001332 ) ) ;
#53191 = EDGE_CURVE ( 'NONE', #2372, #16272, #60566, .T. ) ;
#53192 = CARTESIAN_POINT ( 'NONE',  ( 24.44062500061451715, -3.027376345333614438, 5.243569643749998122 ) ) ;
#53193 = CARTESIAN_POINT ( 'NONE',  ( 26.32499999999999929, 4.330127018922191873, 2.499999999999999556 ) ) ;
#53194 = CARTESIAN_POINT ( 'NONE',  ( -2.000000000000000000, 16.88750000122903572, -33.46410161513775705 ) ) ;
#53195 = CARTESIAN_POINT ( 'NONE',  ( 26.99062500061451431, 6.054752690667223547, 3.707466751127219781E-16 ) ) ;
#53196 = CARTESIAN_POINT ( 'NONE',  ( 11.50312500061451892, -4.541064518000417216, -2.621784821875001281 ) ) ;
#53197 = VERTEX_POINT ( 'NONE', #3713 ) ;
#53198 = CARTESIAN_POINT ( 'NONE',  ( 26.24062500061451431, -3.027376345333614438, 5.243569643749998122 ) ) ;
#53199 = CARTESIAN_POINT ( 'NONE',  ( 4.790625000614518569, -3.027376345333610441, -5.243569643749999898 ) ) ;
#53200 = CARTESIAN_POINT ( 'NONE',  ( 15.04687500061451644, -2.746126346562646425, 4.756430356249996549 ) ) ;
#53201 = CARTESIAN_POINT ( 'NONE',  ( 30.00000000000000000, 0.000000000000000000, 0.000000000000000000 ) ) ;
#53202 = CARTESIAN_POINT ( 'NONE',  ( 12.15000000000000036, -4.330127018922190985, -2.500000000000001332 ) ) ;
#53203 = CARTESIAN_POINT ( 'NONE',  ( 13.09687500061451892, 6.054752690667223547, 3.707466751127219781E-16 ) ) ;
#53204 = CARTESIAN_POINT ( 'NONE',  ( 9.712500001229033231, 4.330127018922192761, -2.499999999999997780 ) ) ;
#53205 = CARTESIAN_POINT ( 'NONE',  ( 17.40937500061451715, -4.541064518000417216, -2.621784821875001281 ) ) ;
#53206 = CARTESIAN_POINT ( 'NONE',  ( 14.69999999999999929, 0.000000000000000000, 4.999999999999998224 ) ) ;
#53207 = CARTESIAN_POINT ( 'NONE',  ( 9.534375000614517148, 4.541064518000418104, 2.621784821874999949 ) ) ;
#53208 = CARTESIAN_POINT ( 'NONE',  ( 2.121784821874999061, 11.55312500061451786, -33.67503911421598417 ) ) ;
#53209 = CARTESIAN_POINT ( 'NONE',  ( 20.17499999999999716, -4.330127018922194537, 2.499999999999995559 ) ) ;
#53210 = CARTESIAN_POINT ( 'NONE',  ( 22.54687500061451644, 0.000000000000000000, 4.756430356249998326 ) ) ;
#53211 = CARTESIAN_POINT ( 'NONE',  ( 15.75000000000000000, -4.330127018922190985, -2.500000000000001332 ) ) ;
#53212 = CARTESIAN_POINT ( 'NONE',  ( 23.39062500061451289, 6.054752690667223547, 3.707466751127219781E-16 ) ) ;
#53213 = CARTESIAN_POINT ( 'NONE',  ( 9.001249775931846008E-16, 10.97187500061451715, 34.90005215228797653 ) ) ;
#53214 = CARTESIAN_POINT ( 'NONE',  ( 26.47499999999999787, -4.330127018922194537, 2.499999999999995559 ) ) ;
#53215 = CARTESIAN_POINT ( 'NONE',  ( 25.05937500061451573, -4.541064518000417216, -2.621784821875001281 ) ) ;
#53216 = CARTESIAN_POINT ( 'NONE',  ( 28.02187500061451431, 3.027376345333611329, 5.243569643749999010 ) ) ;
#53217 = CARTESIAN_POINT ( 'NONE',  ( 4.003125000614518925, 4.541064518000418104, -2.621784821874998173 ) ) ;
#53218 = CARTESIAN_POINT ( 'NONE',  ( 23.48437500061451644, -2.746126346562646425, 4.756430356249996549 ) ) ;
#53219 = CARTESIAN_POINT ( 'NONE',  ( 16.62187500061451573, 3.027376345333613106, -5.243569643749998122 ) ) ;
#53220 = CARTESIAN_POINT ( 'NONE',  ( 8.296875000614518214, -4.119189519843965641, -2.378215178125001383 ) ) ;
#53221 = CARTESIAN_POINT ( 'NONE',  ( 29.25000000122903288, -2.886751345948129988, 4.999999999999997335 ) ) ;
#53222 = CARTESIAN_POINT ( 'NONE',  ( 7.209375000614519635, 4.541064518000418104, -2.621784821874998173 ) ) ;
#53223 = CARTESIAN_POINT ( 'NONE',  ( 18.90937500061451360, 4.541064518000418104, -2.621784821874998173 ) ) ;
#53224 = CARTESIAN_POINT ( 'NONE',  ( -1.297222828952121931, 25.48705884896387985, 26.20721131224835787 ) ) ;
#53225 = CARTESIAN_POINT ( 'NONE',  ( 25.94999999999999929, 0.000000000000000000, 4.999999999999998224 ) ) ;
#53226 = CARTESIAN_POINT ( 'NONE',  ( 26.89687500061451431, -3.027376345333610441, -5.243569643749999898 ) ) ;
#53227 = CARTESIAN_POINT ( 'NONE',  ( 3.756430356249998770, 14.51562499938548356, 32.16877607737302469 ) ) ;
#53228 = CARTESIAN_POINT ( 'NONE',  ( 14.25000000122903288, 5.773502691896255534, 3.535250795749688401E-16 ) ) ;
#53229 = ORIENTED_EDGE ( 'NONE', *, *, #32685, .T. ) ;
#53230 = CARTESIAN_POINT ( 'NONE',  ( 7.350000000000002309, 4.330127018922192761, -2.499999999999997780 ) ) ;
#53231 = CARTESIAN_POINT ( 'NONE',  ( 10.02187500061451431, -4.119189519843968306, 2.378215178124996054 ) ) ;
#53232 = CARTESIAN_POINT ( 'NONE',  ( 20.87812500061451715, -4.541064518000419881, 2.621784821874995952 ) ) ;
#53233 = CARTESIAN_POINT ( 'NONE',  ( 12.11250000000000249, -5.773502691896255534, -1.060575238724906372E-15 ) ) ;
#53234 = ADVANCED_FACE ( 'NONE', ( #20680 ), #21048, .F. ) ;
#53235 = CARTESIAN_POINT ( 'NONE',  ( 8.175000001229031810, -5.773502691896255534, -1.060575238724906372E-15 ) ) ;
#53236 = CARTESIAN_POINT ( 'NONE',  ( 5.390625000614518214, 6.054752690667223547, 3.707466751127219781E-16 ) ) ;
#53237 = CARTESIAN_POINT ( 'NONE',  ( 21.15000000000000213, -4.330127018922190985, -2.500000000000001332 ) ) ;
#53238 = CARTESIAN_POINT ( 'NONE',  ( 17.80312500061451786, -4.541064518000417216, -2.621784821875001281 ) ) ;
#53239 = CARTESIAN_POINT ( 'NONE',  ( 12.15000000000000036, -4.330127018922190985, -2.500000000000001332 ) ) ;
#53240 = CARTESIAN_POINT ( 'NONE',  ( 25.76250000122903216, -4.330127018922190985, -2.500000000000001332 ) ) ;
#53241 = CARTESIAN_POINT ( 'NONE',  ( 1.878215178124997609, 19.31562499938548427, 33.25316411605952993 ) ) ;
#53242 = CARTESIAN_POINT ( 'NONE',  ( 4.875000000000000888, -4.330127018922194537, 2.499999999999995559 ) ) ;
#53243 = ORIENTED_EDGE ( 'NONE', *, *, #53130, .T. ) ;
#53244 = CARTESIAN_POINT ( 'NONE',  ( 18.92812500061451431, 4.541064518000418104, 2.621784821874999949 ) ) ;
#53245 = CARTESIAN_POINT ( 'NONE',  ( 26.65312500061451573, 0.000000000000000000, 5.243569643749999010 ) ) ;
#53246 = CARTESIAN_POINT ( 'NONE',  ( 26.10937500061451644, 4.541064518000418104, -2.621784821874998173 ) ) ;
#53247 = CARTESIAN_POINT ( 'NONE',  ( 9.975000000000001421, 6.123233995736764310E-16, -4.999999999999998224 ) ) ;
#53248 = CARTESIAN_POINT ( 'NONE',  ( 14.42812500061451786, 4.541064518000418104, 2.621784821874999949 ) ) ;
#53249 = DIRECTION ( 'NONE',  ( -0.000000000000000000, -1.000000000000000000, -0.000000000000000000 ) ) ;
#53250 = CARTESIAN_POINT ( 'NONE',  ( 8.315625000614515372, -6.054752690667223547, -1.112240025338166033E-15 ) ) ;
#53251 = DIRECTION ( 'NONE',  ( 0.000000000000000000, 0.000000000000000000, 1.000000000000000000 ) ) ;
#53252 = CARTESIAN_POINT ( 'NONE',  ( 4.243569643749999898, 11.98437500061451821, 30.00000000000000000 ) ) ;
#53253 = CARTESIAN_POINT ( 'NONE',  ( 25.72500000122903074, -5.773502691896255534, -1.060575238724906372E-15 ) ) ;
#53254 = CARTESIAN_POINT ( 'NONE',  ( 20.48437500061451289, -4.119189519843968306, 2.378215178124996054 ) ) ;
#53255 = CARTESIAN_POINT ( 'NONE',  ( 17.65312500061451573, 0.000000000000000000, 5.243569643749999010 ) ) ;
#53256 = CARTESIAN_POINT ( 'NONE',  ( 1.626862140677534273E-15, 13.36250000000000071, 34.00000000000000000 ) ) ;
#53257 = VECTOR ( 'NONE', #64158, 1000.000000000000000 ) ;
#53258 = CARTESIAN_POINT ( 'NONE',  ( 9.309375000614517504, -4.541064518000417216, -2.621784821875001281 ) ) ;
#53259 = CARTESIAN_POINT ( 'NONE',  ( 10.50937500061451679, 0.000000000000000000, 5.243569643749999010 ) ) ;
#53260 = CARTESIAN_POINT ( 'NONE',  ( 17.33437500061451431, -4.541064518000419881, 2.621784821874995952 ) ) ;
#53261 = ORIENTED_EDGE ( 'NONE', *, *, #42409, .T. ) ;
#53262 = CARTESIAN_POINT ( 'NONE',  ( 15.18750000000000000, -2.886751345948130876, 4.999999999999996447 ) ) ;
#53263 = CARTESIAN_POINT ( 'NONE',  ( 20.95312500061451999, -4.541064518000417216, -2.621784821875001281 ) ) ;
#53264 = CARTESIAN_POINT ( 'NONE',  ( 16.32187500061451502, 3.027376345333611329, 5.243569643749999010 ) ) ;
#53265 = CARTESIAN_POINT ( 'NONE',  ( 21.70312500061451644, 0.000000000000000000, 5.243569643749999010 ) ) ;
#53266 = CARTESIAN_POINT ( 'NONE',  ( -3.999999999999999556, 15.46250000000000036, 27.69059892324149530 ) ) ;
#53267 = CARTESIAN_POINT ( 'NONE',  ( 27.44062500061451715, 6.054752690667223547, 3.707466751127219781E-16 ) ) ;
#53268 = CARTESIAN_POINT ( 'NONE',  ( 7.462500001229035007, 4.330127018922192761, -2.499999999999997780 ) ) ;
#53269 = EDGE_LOOP ( 'NONE', ( #13053, #23889, #31896, #1727, #48992, #36276, #16931, #15579, #60355, #16516, #30151, #51866, #72553, #70257, #32464, #3078, #28044, #9198, #18017, #4725, #65834, #47772, #24822, #51965, #39230, #60677, #27312, #18904, #43920, #35882, #68950, #6596, #69676, #68737, #69732, #53773, #2495, #42687, #35154, #16910, #26674, #68236, #37714, #50306, #9283, #38233, #62860, #38844, #2819, #43062, #9462, #62805, #24654, #9806, #25018, #65220, #37355, #43790, #463, #18016, #28268, #62469, #388, #54514, #28373, #12940, #60036, #61718, #5584, #9862, #33809, #35118, #45260, #51066, #23108, #28519, #16337, #25019, #70240, #44555, #33704, #33696, #33441, #56201, #13496, #15192, #17994, #14607, #3549, #37568, #62714, #41749, #53563, #53875, #34194, #57312, #1141, #1291, #9947, #64294, #48487, #69252, #59257, #23419, #18797, #13458, #47425, #52838, #6448, #72749, #36325, #64076, #50891, #4484, #40478, #30652, #1244, #47329 ) ) ;
#53270 = CARTESIAN_POINT ( 'NONE',  ( 4.950000001229033941, -2.886751345948129988, 4.999999999999997335 ) ) ;
#53271 = CARTESIAN_POINT ( 'NONE',  ( -2.828200636599751609E-16, 18.98749999999999716, -34.61880215351700230 ) ) ;
#53272 = CARTESIAN_POINT ( 'NONE',  ( 24.07500000122903216, 2.886751345948129099, -4.999999999999998224 ) ) ;
#53273 = CARTESIAN_POINT ( 'NONE',  ( 2.000000000000000444, 20.61874999877096570, 26.53589838486224650 ) ) ;
#53274 = CARTESIAN_POINT ( 'NONE',  ( 6.721875000614518925, 3.027376345333613106, -5.243569643749998122 ) ) ;
#53275 = CARTESIAN_POINT ( 'NONE',  ( 45.00000000000000000, 0.000000000000000000, 4.999999999999998224 ) ) ;
#53276 = CARTESIAN_POINT ( 'NONE',  ( 13.82812500061451466, 6.421520780324663323E-16, -5.243569643749999010 ) ) ;
#53277 = CARTESIAN_POINT ( 'NONE',  ( 9.534375000614517148, 4.541064518000418104, 2.621784821874999949 ) ) ;
#53278 = CARTESIAN_POINT ( 'NONE',  ( 26.96250000122903145, 0.000000000000000000, 4.999999999999998224 ) ) ;
#53279 = CARTESIAN_POINT ( 'NONE',  ( 18.08437500061451431, 4.541064518000418104, 2.621784821874999949 ) ) ;
#53280 = CARTESIAN_POINT ( 'NONE',  ( 4.659375000614518925, 0.000000000000000000, 5.243569643749999010 ) ) ;
#53281 = DIRECTION ( 'NONE',  ( -1.000000000000000000, -0.000000000000000000, -0.000000000000000000 ) ) ;
#53282 = CARTESIAN_POINT ( 'NONE',  ( 4.378125000614518925, 6.421520780324663323E-16, -5.243569643749999010 ) ) ;
#53283 = CARTESIAN_POINT ( 'NONE',  ( 18.10312500061451502, 0.000000000000000000, 5.243569643749999010 ) ) ;
#53284 = ORIENTED_EDGE ( 'NONE', *, *, #10988, .T. ) ;
#53285 = CARTESIAN_POINT ( 'NONE',  ( 11.54062500061451857, -3.027376345333610441, -5.243569643749999898 ) ) ;
#53286 = CARTESIAN_POINT ( 'NONE',  ( 5.212500001229032343, 4.330127018922192761, -2.499999999999997780 ) ) ;
#53287 = CARTESIAN_POINT ( 'NONE',  ( 10.67812500061451608, 6.421520780324663323E-16, -5.243569643749999010 ) ) ;
#53288 = CARTESIAN_POINT ( 'NONE',  ( 20.70937500061451786, 4.119189519843966529, -2.378215178124998275 ) ) ;
#53289 = CARTESIAN_POINT ( 'NONE',  ( 10.16249999999999964, 2.886751345948126879, 4.999999999999999112 ) ) ;
#53290 = EDGE_CURVE ( 'NONE', #16431, #21477, #714, .T. ) ;
#53291 = CARTESIAN_POINT ( 'NONE',  ( 6.262500001229034829, 0.000000000000000000, 4.999999999999998224 ) ) ;
#53292 = CARTESIAN_POINT ( 'NONE',  ( 21.30000000000000071, 4.330127018922192761, -2.499999999999997780 ) ) ;
#53293 = CARTESIAN_POINT ( 'NONE',  ( 14.82187500061451679, 3.027376345333613106, -5.243569643749998122 ) ) ;
#53294 = CARTESIAN_POINT ( 'NONE',  ( 15.00000000122903465, -2.886751345948125991, -5.000000000000000000 ) ) ;
#53295 = CARTESIAN_POINT ( 'NONE',  ( 22.19999999999999574, 4.330127018922192761, -2.499999999999997780 ) ) ;
#53296 = CARTESIAN_POINT ( 'NONE',  ( 2.121784821874999061, 18.30312500061451431, -33.67503911421598417 ) ) ;
#53297 = CARTESIAN_POINT ( 'NONE',  ( -5.810221930991193690E-16, 14.93750000000000000, 26.00000000000000355 ) ) ;
#53298 = CARTESIAN_POINT ( 'NONE',  ( -1.999999999999997113, 18.72500000000000142, 33.46410161513775705 ) ) ;
#53299 = CARTESIAN_POINT ( 'NONE',  ( 4.321875000614518569, -6.054752690667223547, -1.112240025338166033E-15 ) ) ;
#53300 = CYLINDRICAL_SURFACE ( 'NONE', #25680, 4.000000000000000000 ) ;
#53301 = CARTESIAN_POINT ( 'NONE',  ( 30.00000000000000000, 0.000000000000000000, 0.000000000000000000 ) ) ;
#53302 = CARTESIAN_POINT ( 'NONE',  ( 15.72187500061451892, 3.027376345333613106, -5.243569643749998122 ) ) ;
#53303 = CARTESIAN_POINT ( 'NONE',  ( 29.25000000000000000, -4.330127018922190985, -2.500000000000001332 ) ) ;
#53304 = CARTESIAN_POINT ( 'NONE',  ( 10.94062500061451537, -3.027376345333614438, 5.243569643749998122 ) ) ;
#53305 = CIRCLE ( 'NONE', #27396, 5.999999999999998224 ) ;
#53306 = CARTESIAN_POINT ( 'NONE',  ( 29.14687500061451431, 4.119189519843966529, -2.378215178124998275 ) ) ;
#53307 = CARTESIAN_POINT ( 'NONE',  ( 24.53437500061451715, -4.541064518000419881, 2.621784821874995952 ) ) ;
#53308 = CARTESIAN_POINT ( 'NONE',  ( 17.07187500061451502, 4.119189519843966529, 2.378215178124999607 ) ) ;
#53309 = CARTESIAN_POINT ( 'NONE',  ( 10.49062500061451431, -3.027376345333614438, 5.243569643749998122 ) ) ;
#53310 = CARTESIAN_POINT ( 'NONE',  ( 16.58437500061451786, 6.421520780324663323E-16, -5.243569643749999010 ) ) ;
#53311 = VERTEX_POINT ( 'NONE', #42864 ) ;
#53312 = CARTESIAN_POINT ( 'NONE',  ( 25.28437500061451715, 4.541064518000418104, 2.621784821874999949 ) ) ;
#53313 = CARTESIAN_POINT ( 'NONE',  ( 28.04062500061451502, -3.027376345333614438, 5.243569643749998122 ) ) ;
#53314 = CARTESIAN_POINT ( 'NONE',  ( 19.00312500061451715, 0.000000000000000000, 5.243569643749999010 ) ) ;
#53315 = CARTESIAN_POINT ( 'NONE',  ( 27.96562500061451928, 3.027376345333611329, 5.243569643749999010 ) ) ;
#53316 = CARTESIAN_POINT ( 'NONE',  ( 4.864635650123212862, 1.155751203253316817, -5.114655441610994835 ) ) ;
#53317 = CARTESIAN_POINT ( 'NONE',  ( 7.012500000000001066, 2.886751345948126879, 4.999999999999999112 ) ) ;
#53318 = CARTESIAN_POINT ( 'NONE',  ( 19.72500000122903074, 2.886751345948126879, 4.999999999999999112 ) ) ;
#53319 = DIRECTION ( 'NONE',  ( -0.000000000000000000, -1.000000000000000000, -0.000000000000000000 ) ) ;
#53320 = CARTESIAN_POINT ( 'NONE',  ( 7.696875000614517681, 0.000000000000000000, 4.756430356249998326 ) ) ;
#53321 = ORIENTED_EDGE ( 'NONE', *, *, #643, .F. ) ;
#53322 = CARTESIAN_POINT ( 'NONE',  ( 15.97499999999999964, 4.330127018922191873, 2.499999999999999556 ) ) ;
#53323 = CARTESIAN_POINT ( 'NONE',  ( 19.79999999999999716, -4.330127018922190985, -2.500000000000001332 ) ) ;
#53324 = CARTESIAN_POINT ( 'NONE',  ( 15.87187500061451573, 3.027376345333611329, 5.243569643749999010 ) ) ;
#53325 = CARTESIAN_POINT ( 'NONE',  ( 14.46562500061451750, 3.027376345333611329, 5.243569643749999010 ) ) ;
#53326 = EDGE_CURVE ( 'NONE', #3324, #34631, #56387, .T. ) ;
#53327 = ORIENTED_EDGE ( 'NONE', *, *, #33228, .F. ) ;
#53328 = LINE ( 'NONE', #42977, #72577 ) ;
#53329 = CARTESIAN_POINT ( 'NONE',  ( 2.121784821874999061, 16.10937500061451644, -33.67503911421598417 ) ) ;
#53330 = CARTESIAN_POINT ( 'NONE',  ( 6.328125000614515550, 4.541064518000418104, 2.621784821874999949 ) ) ;
#53331 = CARTESIAN_POINT ( 'NONE',  ( -1.071796769724490339, 13.98259618943233740, 26.00000000000000000 ) ) ;
#53332 = CARTESIAN_POINT ( 'NONE',  ( 11.73750000000000249, -2.886751345948125991, -5.000000000000000000 ) ) ;
#53333 = CARTESIAN_POINT ( 'NONE',  ( 28.73437500061451644, 5.492252693125287522, 3.363034840372157021E-16 ) ) ;
#53334 = CARTESIAN_POINT ( 'NONE',  ( 2.121784821874999061, 14.25312500061451715, 26.32496088578401583 ) ) ;
#53335 = CARTESIAN_POINT ( 'NONE',  ( 26.95312500061451644, 4.541064518000418104, -2.621784821874998173 ) ) ;
#53336 = CARTESIAN_POINT ( 'NONE',  ( 7.650000000000000355, -4.330127018922190985, -2.500000000000001332 ) ) ;
#53337 = CARTESIAN_POINT ( 'NONE',  ( -7.967954043666661671E-16, 17.02812499938548285, 34.33755215474603517 ) ) ;
#53338 = CARTESIAN_POINT ( 'NONE',  ( 24.53437500061451715, -4.541064518000419881, 2.621784821874995952 ) ) ;
#53339 = CARTESIAN_POINT ( 'NONE',  ( 20.61562500061451431, 3.027376345333613106, -5.243569643749998122 ) ) ;
#53340 = CARTESIAN_POINT ( 'NONE',  ( -3.000416591977282496E-16, 15.19062500061459353, -34.90005215228797653 ) ) ;
#53341 = CARTESIAN_POINT ( 'NONE',  ( 22.46250000122903501, 0.000000000000000000, 4.999999999999998224 ) ) ;
#53342 = CARTESIAN_POINT ( 'NONE',  ( 6.478125000614516793, -4.541064518000419881, 2.621784821874995952 ) ) ;
#53343 = CARTESIAN_POINT ( 'NONE',  ( 27.00937500061451857, 4.119189519843966529, -2.378215178124998275 ) ) ;
#53344 = CARTESIAN_POINT ( 'NONE',  ( 24.70312500061451644, 4.541064518000418104, -2.621784821874998173 ) ) ;
#53345 = CARTESIAN_POINT ( 'NONE',  ( 10.95937500061451964, 0.000000000000000000, 4.756430356249998326 ) ) ;
#53346 = CARTESIAN_POINT ( 'NONE',  ( -1.878215178124999163, 15.04062499938548392, 26.74683588394047007 ) ) ;
#53347 = CARTESIAN_POINT ( 'NONE',  ( 15.68437500061451573, 6.421520780324663323E-16, -5.243569643749999010 ) ) ;
#53348 = CARTESIAN_POINT ( 'NONE',  ( 24.45937500061451786, 0.000000000000000000, 5.243569643749999010 ) ) ;
#53349 = CARTESIAN_POINT ( 'NONE',  ( -4.243569643749999898, 14.00937500061451857, 30.00000000000000000 ) ) ;
#53350 = CARTESIAN_POINT ( 'NONE',  ( 5.165625000614518569, -6.054752690667223547, -1.112240025338166033E-15 ) ) ;
#53351 = CARTESIAN_POINT ( 'NONE',  ( 29.76562500061451644, 3.027376345333611329, 5.243569643749999010 ) ) ;
#53352 = CARTESIAN_POINT ( 'NONE',  ( 29.54062500061451502, -3.027376345333610441, -5.243569643749999898 ) ) ;
#53353 = CARTESIAN_POINT ( 'NONE',  ( -1.071796769724486120, 15.06740381056766687, 34.00000000000000000 ) ) ;
#53354 = CARTESIAN_POINT ( 'NONE',  ( 2.516621263038615997, 9.679961675009989719, -35.45028981414222358 ) ) ;
#53355 = CARTESIAN_POINT ( 'NONE',  ( 3.103125000614517237, 4.541064518000418104, -2.621784821874998173 ) ) ;
#53356 = CARTESIAN_POINT ( 'NONE',  ( 7.584375000614516082, 6.421520780324663323E-16, -5.243569643749999010 ) ) ;
#53357 =( LENGTH_UNIT ( ) NAMED_UNIT ( * ) SI_UNIT ( .MILLI., .METRE. ) );
#53358 = CARTESIAN_POINT ( 'NONE',  ( 16.08750000122903501, 4.330127018922191873, 2.499999999999999556 ) ) ;
#53359 = CARTESIAN_POINT ( 'NONE',  ( 29.31562500061451715, 3.027376345333611329, 5.243569643749999010 ) ) ;
#53360 = CARTESIAN_POINT ( 'NONE',  ( 4.490625000614516971, 6.054752690667223547, 3.707466751127219781E-16 ) ) ;
#53361 = CARTESIAN_POINT ( 'NONE',  ( 2.828200636599751609E-16, 14.35624999877096641, 25.38119784648299415 ) ) ;
#53362 = CARTESIAN_POINT ( 'NONE',  ( 21.24375000122903501, -2.886751345948125991, -5.000000000000000000 ) ) ;
#53363 = CARTESIAN_POINT ( 'NONE',  ( 13.24687500061451750, -3.027376345333614438, 5.243569643749998122 ) ) ;
#53364 = CARTESIAN_POINT ( 'NONE',  ( 27.56250000000000000, 2.886751345948162850, -4.999999999999940492 ) ) ;
#53365 = ORIENTED_EDGE ( 'NONE', *, *, #51961, .F. ) ;
#53366 = CARTESIAN_POINT ( 'NONE',  ( 22.22812500061451502, -4.541064518000419881, 2.621784821874995952 ) ) ;
#53367 = CARTESIAN_POINT ( 'NONE',  ( 8.128125000614515372, 4.541064518000418104, 2.621784821874999949 ) ) ;
#53368 = CARTESIAN_POINT ( 'NONE',  ( 23.97187500061451715, 3.027376345333611329, 5.243569643749999010 ) ) ;
#53369 = CARTESIAN_POINT ( 'NONE',  ( 7.678125000614516082, 4.541064518000418104, 2.621784821874999949 ) ) ;
#53370 = CARTESIAN_POINT ( 'NONE',  ( 29.77499999999999858, 6.123233995736764310E-16, -4.999999999999998224 ) ) ;
#53371 = CARTESIAN_POINT ( 'NONE',  ( 10.01250000122903394, -4.330127018922190985, -2.500000000000001332 ) ) ;
#53372 = CARTESIAN_POINT ( 'NONE',  ( 24.70312500061451644, 4.541064518000418104, -2.621784821874998173 ) ) ;
#53373 = VECTOR ( 'NONE', #15202, 1000.000000000000000 ) ;
#53374 = CARTESIAN_POINT ( 'NONE',  ( 3.999999999999998668, 19.47500000122903430, -32.30940107675850470 ) ) ;
#53375 = CARTESIAN_POINT ( 'NONE',  ( 10.23750000122903359, 4.330127018922191873, 2.499999999999999556 ) ) ;
#53376 = CARTESIAN_POINT ( 'NONE',  ( 22.82812500061451644, 6.421520780324663323E-16, -5.243569643749999010 ) ) ;
#53377 = CARTESIAN_POINT ( 'NONE',  ( 17.80312500061451786, -4.541064518000417216, -2.621784821875001281 ) ) ;
#53378 = CARTESIAN_POINT ( 'NONE',  ( 28.47187500061451715, 2.746126346562643317, 4.756430356249998326 ) ) ;
#53379 = CARTESIAN_POINT ( 'NONE',  ( 17.77499999999999858, 4.330127018922191873, 2.499999999999999556 ) ) ;
#53380 = CARTESIAN_POINT ( 'NONE',  ( 14.85000000122903252, -2.886751345948129988, 4.999999999999997335 ) ) ;
#53381 =( BOUNDED_CURVE ( )  B_SPLINE_CURVE ( 2, ( #217, #44562, #72984, #22366, #44918, #50815, #22722 ),
 .UNSPECIFIED., .F., .F. ) 
 B_SPLINE_CURVE_WITH_KNOTS ( ( 3, 2, 2, 3 ),
 ( 0.7299999999999999822, 0.7333333333333332815, 0.7366666666666666918, 0.7399999999999999911 ),
 .UNSPECIFIED. ) 
 CURVE ( )  GEOMETRIC_REPRESENTATION_ITEM ( )  RATIONAL_B_SPLINE_CURVE ( ( 1.000000000000000000, 0.8660254037844387076, 1.000000000000000000, 0.8660254037844387076, 1.000000000000000000, 0.8660254037844387076, 1.000000000000000000 ) ) 
 REPRESENTATION_ITEM ( '' )  );
#53382 = CARTESIAN_POINT ( 'NONE',  ( 10.71562500061451928, 3.027376345333613106, -5.243569643749998122 ) ) ;
#53383 = CARTESIAN_POINT ( 'NONE',  ( 12.51562500061451821, 3.027376345333613106, -5.243569643749998122 ) ) ;
#53384 = CARTESIAN_POINT ( 'NONE',  ( 23.25000000122903288, 5.773502691896255534, 3.535250795749688894E-16 ) ) ;
#53385 = CARTESIAN_POINT ( 'NONE',  ( 22.65937500061451715, 0.000000000000000000, 5.243569643749999010 ) ) ;
#53386 = CARTESIAN_POINT ( 'NONE',  ( 21.53437500061451715, 6.421520780324663323E-16, -5.243569643749999010 ) ) ;
#53387 = CARTESIAN_POINT ( 'NONE',  ( 24.86250000000000071, 2.886751345948129099, -4.999999999999997335 ) ) ;
#53388 = CARTESIAN_POINT ( 'NONE',  ( 8.737500001229033586, 6.123233995736764310E-16, -4.999999999999998224 ) ) ;
#53389 = CARTESIAN_POINT ( 'NONE',  ( 6.609375000614519102, -4.541064518000417216, -2.621784821875001281 ) ) ;
#53390 = CARTESIAN_POINT ( 'NONE',  ( 24.27187500061452141, 3.027376345333613106, -5.243569643749998122 ) ) ;
#53391 = VECTOR ( 'NONE', #13314, 1000.000000000000000 ) ;
#53392 =( BOUNDED_CURVE ( )  B_SPLINE_CURVE ( 2, ( #60790, #27923, #49728, #16816, #10196, #66345, #22005 ),
 .UNSPECIFIED., .F., .F. ) 
 B_SPLINE_CURVE_WITH_KNOTS ( ( 3, 2, 2, 3 ),
 ( 0.8833333333333333037, 0.8861111111111110716, 0.8888888888888888395, 0.8916666666666667185 ),
 .UNSPECIFIED. ) 
 CURVE ( )  GEOMETRIC_REPRESENTATION_ITEM ( )  RATIONAL_B_SPLINE_CURVE ( ( 1.000000000000000000, 0.8660254037844387076, 1.000000000000000000, 0.8660254037844387076, 1.000000000000000000, 0.8660254037844387076, 1.000000000000000000 ) ) 
 REPRESENTATION_ITEM ( '' )  );
#53393 = CARTESIAN_POINT ( 'NONE',  ( 4.699789363897854955, -1.707107682658927095, 4.926740801328898911 ) ) ;
#53394 = EDGE_CURVE ( 'NONE', #71040, #58014, #71674, .T. ) ;
#53395 = CARTESIAN_POINT ( 'NONE',  ( 22.34062500061451573, -3.027376345333610441, -5.243569643749999898 ) ) ;
#53396 = CARTESIAN_POINT ( 'NONE',  ( 24.75937500061451502, 4.541064518000418104, -2.621784821874998173 ) ) ;
#53397 = CARTESIAN_POINT ( 'NONE',  ( 3.756430356250000546, 18.64062499938548356, 27.83122392262697886 ) ) ;
#53398 = CARTESIAN_POINT ( 'NONE',  ( 3.375730161298836407, -4.192115423953711506, 3.226182382019024519 ) ) ;
#53399 = CARTESIAN_POINT ( 'NONE',  ( 27.63750000122903216, 6.123233995736764310E-16, -4.999999999999998224 ) ) ;
#53400 = CARTESIAN_POINT ( 'NONE',  ( 5.971875000614516260, 3.027376345333611329, 5.243569643749999010 ) ) ;
#53401 = CARTESIAN_POINT ( 'NONE',  ( 16.45312500061451289, -4.541064518000417216, -2.621784821875001281 ) ) ;
#53402 = ORIENTED_EDGE ( 'NONE', *, *, #63906, .F. ) ;
#53403 = CARTESIAN_POINT ( 'NONE',  ( 28.19999999999999929, 0.000000000000000000, 4.999999999999998224 ) ) ;
#53404 = CARTESIAN_POINT ( 'NONE',  ( 25.49062500061451786, -3.027376345333610441, -5.243569643749999898 ) ) ;
#53405 = CARTESIAN_POINT ( 'NONE',  ( 4.509375000614518569, 4.541064518000418104, -2.621784821874998173 ) ) ;
#53406 = CARTESIAN_POINT ( 'NONE',  ( 4.750580614020113224, 1.560202551697607465, 4.800619732442354071 ) ) ;
#53407 = CARTESIAN_POINT ( 'NONE',  ( 11.21250000000000036, -5.773502691896255534, -1.060575238724906372E-15 ) ) ;
#53408 = CARTESIAN_POINT ( 'NONE',  ( 15.07499999999999929, 4.330127018922191873, 2.499999999999999556 ) ) ;
#53409 = CARTESIAN_POINT ( 'NONE',  ( 26.02500000122903145, 2.886751345948126879, 4.999999999999999112 ) ) ;
#53410 = CARTESIAN_POINT ( 'NONE',  ( 22.11562500061451786, 3.027376345333611329, 5.243569643749999010 ) ) ;
#53411 = VERTEX_POINT ( 'NONE', #26976 ) ;
#53412 = CARTESIAN_POINT ( 'NONE',  ( 25.61250000000000071, -5.773502691896255534, -1.060575238724906372E-15 ) ) ;
#53413 = CARTESIAN_POINT ( 'NONE',  ( 26.85937500061451644, -4.541064518000417216, -2.621784821875001281 ) ) ;
#53414 = ADVANCED_FACE ( 'NONE', ( #72034 ), #21410, .T. ) ;
#53415 = ORIENTED_EDGE ( 'NONE', *, *, #12441, .F. ) ;
#53416 = CARTESIAN_POINT ( 'NONE',  ( 30.00000000000000000, 0.000000000000000000, 0.000000000000000000 ) ) ;
#53417 = CARTESIAN_POINT ( 'NONE',  ( 12.40312500061451573, -4.541064518000417216, -2.621784821875001281 ) ) ;
#53418 = CARTESIAN_POINT ( 'NONE',  ( 24.97500000122903074, 2.886751345948112668, -5.000000000000024869 ) ) ;
#53419 = CARTESIAN_POINT ( 'NONE',  ( 17.14687500061451431, 0.000000000000000000, 4.756430356249998326 ) ) ;
#53420 = CARTESIAN_POINT ( 'NONE',  ( 28.30312500061451431, 4.541064518000418104, -2.621784821874998173 ) ) ;
#53421 =( BOUNDED_CURVE ( )  B_SPLINE_CURVE ( 2, ( #57450, #57804, #36005, #63362, #64075, #69278, #12746 ),
 .UNSPECIFIED., .F., .F. ) 
 B_SPLINE_CURVE_WITH_KNOTS ( ( 3, 2, 2, 3 ),
 ( 0.3199999999999999512, 0.3233333333333333059, 0.3266666666666666607, 0.3300000000000000711 ),
 .UNSPECIFIED. ) 
 CURVE ( )  GEOMETRIC_REPRESENTATION_ITEM ( )  RATIONAL_B_SPLINE_CURVE ( ( 1.000000000000002220, 0.8660254037844364872, 1.000000000000000000, 0.8660254037844387076, 1.000000000000000000, 0.8660254037844364872, 1.000000000000002220 ) ) 
 REPRESENTATION_ITEM ( '' )  );
#53422 = CARTESIAN_POINT ( 'NONE',  ( 13.87500000122903465, 2.886751345948126879, 4.999999999999999112 ) ) ;
#53423 = CARTESIAN_POINT ( 'NONE',  ( 20.51249999999999929, 2.886751345948126879, 4.999999999999999112 ) ) ;
#53424 = CARTESIAN_POINT ( 'NONE',  ( 26.77499999999999858, 4.330127018922191873, 2.499999999999999556 ) ) ;
#53425 = CARTESIAN_POINT ( 'NONE',  ( 4.000000000000000000, 14.28124999877096890, 27.69059892324149885 ) ) ;
#53426 = CARTESIAN_POINT ( 'NONE',  ( 7.996875000614519280, -3.027376345333610441, -5.243569643749999898 ) ) ;
#53427 = CARTESIAN_POINT ( 'NONE',  ( 20.55937500061451573, -4.541064518000417216, -2.621784821875001281 ) ) ;
#53428 = CARTESIAN_POINT ( 'NONE',  ( 45.00000000000000000, 0.000000000000000000, 0.000000000000000000 ) ) ;
#53429 = EDGE_LOOP ( 'NONE', ( #18832, #51169, #68145, #42287 ) ) ;
#53430 = CARTESIAN_POINT ( 'NONE',  ( 27.96562500061451928, 3.027376345333611329, 5.243569643749999010 ) ) ;
#53431 = CARTESIAN_POINT ( 'NONE',  ( 29.25937500061451502, 4.541064518000418104, -2.621784821874998173 ) ) ;
#53432 = CARTESIAN_POINT ( 'NONE',  ( 3.534375000614518036, 6.421520780324663323E-16, -5.243569643749999010 ) ) ;
#53433 = CARTESIAN_POINT ( 'NONE',  ( 15.75000000000000000, -4.330127018922190985, -2.500000000000001332 ) ) ;
#53434 = CARTESIAN_POINT ( 'NONE',  ( 12.62812500061451537, 4.541064518000418104, 2.621784821874999949 ) ) ;
#53435 = FACE_OUTER_BOUND ( 'NONE', #7493, .T. ) ;
#53436 = DIRECTION ( 'NONE',  ( 0.000000000000000000, 0.000000000000000000, -1.000000000000000000 ) ) ;
#53437 = CARTESIAN_POINT ( 'NONE',  ( 4.050000000000001599, -4.330127018922190985, -2.500000000000001332 ) ) ;
#53438 = CARTESIAN_POINT ( 'NONE',  ( 17.66250000122903430, -4.330127018922190985, -2.500000000000001332 ) ) ;
#53439 = CARTESIAN_POINT ( 'NONE',  ( 17.29687500061451999, -2.746126346562646425, 4.756430356249996549 ) ) ;
#53440 = CARTESIAN_POINT ( 'NONE',  ( 6.890625000614516438, -3.027376345333614438, 5.243569643749998122 ) ) ;
#53441 = CARTESIAN_POINT ( 'NONE',  ( 24.60937500061451644, -4.541064518000417216, -2.621784821875001281 ) ) ;
#53442 = ADVANCED_FACE ( 'NONE', ( #60936 ), #10340, .T. ) ;
#53443 = CARTESIAN_POINT ( 'NONE',  ( -2.121784821874999949, 17.08437500061451786, 26.32496088578401938 ) ) ;
#53444 = CARTESIAN_POINT ( 'NONE',  ( 24.12187500061451217, -6.054752690667223547, -1.112240025338166033E-15 ) ) ;
#53445 = CARTESIAN_POINT ( 'NONE',  ( 4.537500000000000533, -2.886751345948125991, -5.000000000000000000 ) ) ;
#53446 = CARTESIAN_POINT ( 'NONE',  ( -2.828200636599751609E-16, 10.10000000122903430, 25.38119784648299770 ) ) ;
#53447 = CARTESIAN_POINT ( 'NONE',  ( 12.96562500061451750, 3.027376345333613106, -5.243569643749998122 ) ) ;
#53448 = CARTESIAN_POINT ( 'NONE',  ( 4.425000001229032698, 2.886751345948126879, 4.999999999999999112 ) ) ;
#53449 = CARTESIAN_POINT ( 'NONE',  ( 9.909375000614517148, 4.541064518000418104, -2.621784821874998173 ) ) ;
#53450 = CARTESIAN_POINT ( 'NONE',  ( -0.6906555412606095734, 4.953935347589260019, -26.05769473322559548 ) ) ;
#53451 = ORIENTED_EDGE ( 'NONE', *, *, #3140, .F. ) ;
#53452 = CARTESIAN_POINT ( 'NONE',  ( 12.02812500061451573, 6.421520780324663323E-16, -5.243569643749999010 ) ) ;
#53453 = DIRECTION ( 'NONE',  ( -0.000000000000000000, -1.000000000000000000, -0.000000000000000000 ) ) ;
#53454 = CARTESIAN_POINT ( 'NONE',  ( 23.58750000122903145, 6.123233995736764310E-16, -4.999999999999998224 ) ) ;
#53455 = CARTESIAN_POINT ( 'NONE',  ( 10.43437500061451750, 4.541064518000418104, 2.621784821874999949 ) ) ;
#53456 = CARTESIAN_POINT ( 'NONE',  ( 12.02812500061451573, 6.421520780324663323E-16, -5.243569643749999010 ) ) ;
#53457 = CARTESIAN_POINT ( 'NONE',  ( 27.13125000122903430, 6.123233995736764310E-16, -4.999999999999998224 ) ) ;
#53458 = CARTESIAN_POINT ( 'NONE',  ( 21.72187500061451715, 3.027376345333611329, 5.243569643749999010 ) ) ;
#53459 = CARTESIAN_POINT ( 'NONE',  ( 2.000000000000001332, 15.76250000122903216, 33.46410161513774995 ) ) ;
#53460 = DIRECTION ( 'NONE',  ( -1.000000000000000000, -0.000000000000000000, -0.000000000000000000 ) ) ;
#53461 = CARTESIAN_POINT ( 'NONE',  ( 3.167073630078104607, 3.869168037755827960, -3.482309847224001054 ) ) ;
#53462 = CARTESIAN_POINT ( 'NONE',  ( -2.121784821874996840, 13.63437500061451857, -26.32496088578401583 ) ) ;
#53463 = CARTESIAN_POINT ( 'NONE',  ( 16.05937500061451573, -4.541064518000417216, -2.621784821875001281 ) ) ;
#53464 = CARTESIAN_POINT ( 'NONE',  ( 18.37500000122903288, 2.886751345948126879, 4.999999999999999112 ) ) ;
#53465 = CARTESIAN_POINT ( 'NONE',  ( 12.04687500061451821, -3.027376345333610441, -5.243569643749999898 ) ) ;
#53466 = CARTESIAN_POINT ( 'NONE',  ( 9.001249775931846008E-16, 18.56562500061451715, -25.09994784771203058 ) ) ;
#53467 = CARTESIAN_POINT ( 'NONE',  ( 17.55000000122903359, -2.886751345948129988, 4.999999999999997335 ) ) ;
#53468 = CARTESIAN_POINT ( 'NONE',  ( 13.30312500061451786, -4.541064518000417216, -2.621784821875001281 ) ) ;
#53469 = VERTEX_POINT ( 'NONE', #13167 ) ;
#53470 = CARTESIAN_POINT ( 'NONE',  ( 16.19999999999999929, -4.330127018922190985, -2.500000000000001332 ) ) ;
#53471 = CARTESIAN_POINT ( 'NONE',  ( 65.00000000000000000, 5.218601775200212955, 7.332543590861030580 ) ) ;
#53472 = CARTESIAN_POINT ( 'NONE',  ( 12.98437500061451821, 6.421520780324663323E-16, -5.243569643749999010 ) ) ;
#53473 = DIRECTION ( 'NONE',  ( 0.000000000000000000, 0.000000000000000000, -1.000000000000000000 ) ) ;
#53474 = CARTESIAN_POINT ( 'NONE',  ( 12.18750000122903465, -4.330127018922194537, 2.499999999999995559 ) ) ;
#53475 = CARTESIAN_POINT ( 'NONE',  ( 21.18750000122903288, -4.330127018922194537, 2.499999999999995559 ) ) ;
#53476 = CARTESIAN_POINT ( 'NONE',  ( 17.87812500061451715, 6.421520780324663323E-16, -5.243569643749999010 ) ) ;
#53477 = CARTESIAN_POINT ( 'NONE',  ( 19.86562500061451786, 3.027376345333611329, 5.243569643749999010 ) ) ;
#53478 = CARTESIAN_POINT ( 'NONE',  ( 28.65000000122903145, 5.773502691896255534, 3.535250795749688894E-16 ) ) ;
#53479 = CARTESIAN_POINT ( 'NONE',  ( 25.16249999999999432, -5.773502691896255534, -1.060575238724906372E-15 ) ) ;
#53480 = CARTESIAN_POINT ( 'NONE',  ( 17.64375000122903003, -2.886751345948126435, -5.000000000000000000 ) ) ;
#53481 = CARTESIAN_POINT ( 'NONE',  ( 29.51249999999999929, 2.886751345948126879, 4.999999999999999112 ) ) ;
#53482 = CARTESIAN_POINT ( 'NONE',  ( 27.72187500061451715, -6.054752690667223547, -1.112240025338166033E-15 ) ) ;
#53483 = CARTESIAN_POINT ( 'NONE',  ( -3.999999999999999112, 9.762500001229033941, -30.00000000000000000 ) ) ;
#53484 = CARTESIAN_POINT ( 'NONE',  ( 4.243569643749999898, 14.23437500061451821, -30.00000000000000000 ) ) ;
#53485 = CARTESIAN_POINT ( 'NONE',  ( 3.037500001229032964, 4.330127018922191873, 2.499999999999999556 ) ) ;
#53486 = CARTESIAN_POINT ( 'NONE',  ( 3.374999999999999556, 4.330127018922191873, 2.499999999999999556 ) ) ;
#53487 = CARTESIAN_POINT ( 'NONE',  ( 3.586992791275801729, 3.483314903268937446, -3.919380039434936513 ) ) ;
#53488 = CARTESIAN_POINT ( 'NONE',  ( 6.684375000614518392, 6.421520780324663323E-16, -5.243569643749999010 ) ) ;
#53489 = CARTESIAN_POINT ( 'NONE',  ( 28.60312500061451502, -4.541064518000417216, -2.621784821875001281 ) ) ;
#53490 = FACE_OUTER_BOUND ( 'NONE', #37442, .T. ) ;
#53491 = CARTESIAN_POINT ( 'NONE',  ( 1.071796769724491893, 17.54509619066136850, -26.00000000000000355 ) ) ;
#53492 = EDGE_CURVE ( 'NONE', #46701, #65074, #62394, .T. ) ;
#53493 = CARTESIAN_POINT ( 'NONE',  ( 5.296875000614518214, -3.027376345333610441, -5.243569643749999898 ) ) ;
#53494 = CARTESIAN_POINT ( 'NONE',  ( 11.07187500061451679, -6.054752690667223547, -1.112240025338166033E-15 ) ) ;
#53495 = CARTESIAN_POINT ( 'NONE',  ( 5.250000000000000888, 0.000000000000000000, 4.999999999999998224 ) ) ;
#53496 = CARTESIAN_POINT ( 'NONE',  ( 4.243569643749999898, 15.04062500061459495, 32.45002607614398471 ) ) ;
#53497 = CARTESIAN_POINT ( 'NONE',  ( 1.042938436496270160, 25.50788288962337447, 33.87058137810289793 ) ) ;
#53498 = CARTESIAN_POINT ( 'NONE',  ( 6.524999999999999467, 4.330127018922191873, 2.499999999999999556 ) ) ;
#53499 = CARTESIAN_POINT ( 'NONE',  ( 14.70937500061451431, 2.746126346562645981, -4.756430356249997438 ) ) ;
#53500 = CARTESIAN_POINT ( 'NONE',  ( 20.16562500061451146, 3.027376345333613106, -5.243569643749998122 ) ) ;
#53501 = CARTESIAN_POINT ( 'NONE',  ( 10.04062500061451502, -3.027376345333614438, 5.243569643749998122 ) ) ;
#53502 = CARTESIAN_POINT ( 'NONE',  ( 24.45937500061451786, -5.492252693125287522, -1.008910452111647106E-15 ) ) ;
#53503 = CARTESIAN_POINT ( 'NONE',  ( 10.20937500061451786, -4.541064518000417216, -2.621784821875001281 ) ) ;
#53504 = CARTESIAN_POINT ( 'NONE',  ( 25.19999999999999929, -4.330127018922190985, -2.500000000000001332 ) ) ;
#53505 = CARTESIAN_POINT ( 'NONE',  ( 20.58750000122903145, 4.330127018922191873, 2.499999999999999556 ) ) ;
#53506 = CARTESIAN_POINT ( 'NONE',  ( 26.91562500061451146, 3.027376345333613106, -5.243569643749998122 ) ) ;
#53507 = DIRECTION ( 'NONE',  ( -0.000000000000000000, -1.000000000000000000, -0.000000000000000000 ) ) ;
#53508 = CARTESIAN_POINT ( 'NONE',  ( 9.009375000614518569, 4.541064518000418104, -2.621784821874998173 ) ) ;
#53509 = CARTESIAN_POINT ( 'NONE',  ( 13.62187500061451750, 3.027376345333611329, 5.243569643749999010 ) ) ;
#53510 = CARTESIAN_POINT ( 'NONE',  ( 26.78437500061451360, -4.541064518000419881, 2.621784821874995952 ) ) ;
#53511 = CARTESIAN_POINT ( 'NONE',  ( -5.810221930991193690E-16, 13.70000000122903394, -34.00000000000000000 ) ) ;
#53512 = CARTESIAN_POINT ( 'NONE',  ( 20.85937500061451644, 0.000000000000000000, 5.243569643749999010 ) ) ;
#53513 = CARTESIAN_POINT ( 'NONE',  ( 10.69687500061451679, -3.027376345333610441, -5.243569643749999898 ) ) ;
#53514 = CARTESIAN_POINT ( 'NONE',  ( -1.878215178125001827, 13.39062499938548356, 33.25316411605952283 ) ) ;
#53515 = CARTESIAN_POINT ( 'NONE',  ( 22.46250000000000213, -5.773502691896255534, -1.060575238724906372E-15 ) ) ;
#53516 = CARTESIAN_POINT ( 'NONE',  ( 4.000000000000000000, 15.23750000000000071, 27.69059892324149530 ) ) ;
#53517 = CARTESIAN_POINT ( 'NONE',  ( -3.000416591977282496E-16, 12.09687500061451715, -34.90005215228797653 ) ) ;
#53518 = CARTESIAN_POINT ( 'NONE',  ( 24.12187500061451217, -5.492252693125287522, -1.008910452111647106E-15 ) ) ;
#53519 = CARTESIAN_POINT ( 'NONE',  ( 14.61562500061451608, -6.054752690667223547, -1.112240025338166033E-15 ) ) ;
#53520 = CARTESIAN_POINT ( 'NONE',  ( 5.100000000000000533, 4.330127018922192761, -2.499999999999997780 ) ) ;
#53521 = LINE ( 'NONE', #7005, #14838 ) ;
#53522 = CARTESIAN_POINT ( 'NONE',  ( 25.50000000000000000, 0.000000000000000000, 4.999999999999998224 ) ) ;
#53523 = CARTESIAN_POINT ( 'NONE',  ( 11.73750000000000249, -2.886751345948125991, -5.000000000000000000 ) ) ;
#53524 = CARTESIAN_POINT ( 'NONE',  ( 1.999999999999998668, 16.81250000122903643, 26.53589838486224650 ) ) ;
#53525 = CARTESIAN_POINT ( 'NONE',  ( 12.45000000122903394, 5.773502691896255534, 3.535250795749688894E-16 ) ) ;
#53526 = CARTESIAN_POINT ( 'NONE',  ( 25.47187500061451715, -6.054752690667223547, -1.112240025338166033E-15 ) ) ;
#53527 = CARTESIAN_POINT ( 'NONE',  ( 15.60937500061451644, -4.541064518000417216, -2.621784821875001281 ) ) ;
#53528 = CARTESIAN_POINT ( 'NONE',  ( 7.320879633048903241E-15, 18.08749999999999858, 26.00000000000000355 ) ) ;
#53529 = VERTEX_POINT ( 'NONE', #33951 ) ;
#53530 = CARTESIAN_POINT ( 'NONE',  ( 19.90312500061451573, 0.000000000000000000, 5.243569643749999010 ) ) ;
#53531 = CARTESIAN_POINT ( 'NONE',  ( 4.640625000614518214, -3.027376345333614438, 5.243569643749998122 ) ) ;
#53532 = CARTESIAN_POINT ( 'NONE',  ( 16.92187500061451999, -6.054752690667223547, -1.112240025338166033E-15 ) ) ;
#53533 = CARTESIAN_POINT ( 'NONE',  ( 28.28437500061451715, 6.421520780324663323E-16, -5.243569643749999010 ) ) ;
#53534 = CARTESIAN_POINT ( 'NONE',  ( 4.678125000614516971, -4.541064518000419881, 2.621784821874995952 ) ) ;
#53535 = CARTESIAN_POINT ( 'NONE',  ( 19.07812500061451644, -4.541064518000419881, 2.621784821874995952 ) ) ;
#53536 = CARTESIAN_POINT ( 'NONE',  ( -2.121784821874999949, 14.77812500061451750, 26.32496088578401938 ) ) ;
#53537 = CARTESIAN_POINT ( 'NONE',  ( 16.76250000122903216, -4.330127018922190985, -2.500000000000001332 ) ) ;
#53538 = CARTESIAN_POINT ( 'NONE',  ( 12.04687500061451821, -2.746126346562641984, -4.756430356249999214 ) ) ;
#53539 = CARTESIAN_POINT ( 'NONE',  ( 7.978125000614517681, 6.421520780324663323E-16, -5.243569643749999010 ) ) ;
#53540 = CARTESIAN_POINT ( 'NONE',  ( 29.65312500061451573, 4.541064518000418104, -2.621784821874998173 ) ) ;
#53541 = CARTESIAN_POINT ( 'NONE',  ( 22.47187500061451715, 3.027376345333613106, -5.243569643749998122 ) ) ;
#53542 = CARTESIAN_POINT ( 'NONE',  ( 15.55312500061451608, -4.541064518000417216, -2.621784821875001281 ) ) ;
#53543 = CARTESIAN_POINT ( 'NONE',  ( 24.97500000122903430, 2.886751345948129099, -4.999999999999998224 ) ) ;
#53544 = CARTESIAN_POINT ( 'NONE',  ( 23.24062500061451786, -3.027376345333610441, -5.243569643749999898 ) ) ;
#53545 = CARTESIAN_POINT ( 'NONE',  ( 19.02187500061451786, 3.027376345333611329, 5.243569643749999010 ) ) ;
#53546 = CARTESIAN_POINT ( 'NONE',  ( 15.14062500061451644, -3.027376345333610441, -5.243569643749999898 ) ) ;
#53547 = CARTESIAN_POINT ( 'NONE',  ( -4.243569643749997233, 14.49687500061451928, 32.45002607614398471 ) ) ;
#53548 = CARTESIAN_POINT ( 'NONE',  ( 20.65312500061451573, 4.541064518000418104, -2.621784821874998173 ) ) ;
#53549 = CARTESIAN_POINT ( 'NONE',  ( 28.94062500061452070, -3.027376345333614438, 5.243569643749998122 ) ) ;
#53550 = VERTEX_POINT ( 'NONE', #16957 ) ;
#53551 = ORIENTED_EDGE ( 'NONE', *, *, #71833, .F. ) ;
#53552 = CARTESIAN_POINT ( 'NONE',  ( 21.82499999999999574, 4.330127018922191873, 2.499999999999999556 ) ) ;
#53553 = CARTESIAN_POINT ( 'NONE',  ( -2.000000000000000000, 11.37500000000000178, -33.46410161513775705 ) ) ;
#53554 = CARTESIAN_POINT ( 'NONE',  ( 1.592000809091587073E-14, 15.38750000000000284, 26.00000000000000000 ) ) ;
#53555 = CARTESIAN_POINT ( 'NONE',  ( 26.05312500061451431, 4.541064518000418104, -2.621784821874998173 ) ) ;
#53556 = CARTESIAN_POINT ( 'NONE',  ( 8.540625000614518569, 6.054752690667223547, 3.707466751127219781E-16 ) ) ;
#53557 = CARTESIAN_POINT ( 'NONE',  ( 19.76250000122903216, 0.000000000000000000, 4.999999999999998224 ) ) ;
#53558 = CARTESIAN_POINT ( 'NONE',  ( 24.89062500061451644, -3.027376345333614438, 5.243569643749998122 ) ) ;
#53559 = CARTESIAN_POINT ( 'NONE',  ( 24.56250000000000000, 2.886751345948126879, 4.999999999999999112 ) ) ;
#53560 =( BOUNDED_CURVE ( )  B_SPLINE_CURVE ( 2, ( #43878, #8420, #65666, #9885, #37593, #32420, #14326, #14685, #4362 ),
 .UNSPECIFIED., .F., .F. ) 
 B_SPLINE_CURVE_WITH_KNOTS ( ( 3, 2, 2, 2, 3 ),
 ( 0.8804347826086956763, 0.8840579710144927938, 0.8913043478260869179, 0.8985507246376811530, 0.9021739130434782705 ),
 .UNSPECIFIED. ) 
 CURVE ( )  GEOMETRIC_REPRESENTATION_ITEM ( )  RATIONAL_B_SPLINE_CURVE ( ( 0.9330127018922194093, 0.9330127018922194093, 1.000000000000000000, 0.8660254037844387076, 1.000000000000000000, 0.8660254037844387076, 1.000000000000000000, 0.9330127018922194093, 0.9330127018922194093 ) ) 
 REPRESENTATION_ITEM ( '' )  );
#53561 = CARTESIAN_POINT ( 'NONE',  ( 26.76562500061451644, -6.054752690667223547, -1.112240025338166033E-15 ) ) ;
#53562 = CARTESIAN_POINT ( 'NONE',  ( 8.015625000614518214, 3.027376345333613106, -5.243569643749998122 ) ) ;
#53563 = ORIENTED_EDGE ( 'NONE', *, *, #38471, .F. ) ;
#53564 = EDGE_CURVE ( 'NONE', #34347, #63177, #68671, .T. ) ;
#53565 = CARTESIAN_POINT ( 'NONE',  ( 23.16562500061451502, -6.054752690667223547, -1.112240025338166033E-15 ) ) ;
#53566 = CARTESIAN_POINT ( 'NONE',  ( 4.340625000614515727, -3.027376345333610441, -5.243569643749999898 ) ) ;
#53567 = CARTESIAN_POINT ( 'NONE',  ( 14.82187500061451679, 2.746126346562645981, -4.756430356249997438 ) ) ;
#53568 = CARTESIAN_POINT ( 'NONE',  ( 2.840625000614518392, -3.027376345333614438, 5.243569643749998122 ) ) ;
#53569 = CARTESIAN_POINT ( 'NONE',  ( -3.999999999999999112, 13.66250000000000142, -32.30940107675850470 ) ) ;
#53570 = CARTESIAN_POINT ( 'NONE',  ( 14.32500000000000107, -4.330127018922194537, 2.499999999999995559 ) ) ;
#53571 = CARTESIAN_POINT ( 'NONE',  ( 14.85937500061451644, 4.541064518000418104, -2.621784821874998173 ) ) ;
#53572 = CARTESIAN_POINT ( 'NONE',  ( 8.025000001229035007, 2.886751345948126879, 4.999999999999999112 ) ) ;
#53573 = CARTESIAN_POINT ( 'NONE',  ( 15.60937500061451644, -4.541064518000417216, -2.621784821875001281 ) ) ;
#53574 = CARTESIAN_POINT ( 'NONE',  ( 15.07499999999999929, 4.330127018922191873, 2.499999999999999556 ) ) ;
#53575 = CARTESIAN_POINT ( 'NONE',  ( 9.346875000614517148, -3.027376345333610441, -5.243569643749999898 ) ) ;
#53576 = CARTESIAN_POINT ( 'NONE',  ( 2.121784821875001281, 11.85312500061451857, -26.32496088578401938 ) ) ;
#53577 = VECTOR ( 'NONE', #27161, 1000.000000000000000 ) ;
#53578 = CARTESIAN_POINT ( 'NONE',  ( 20.28750000000000142, -2.886751345948159742, -4.999999999999942268 ) ) ;
#53579 = ADVANCED_FACE ( 'NONE', ( #56492 ), #23226, .T. ) ;
#53580 = CARTESIAN_POINT ( 'NONE',  ( 13.65937500061451715, 0.000000000000000000, 5.243569643749999010 ) ) ;
#53581 = VERTEX_POINT ( 'NONE', #6248 ) ;
#53582 = CARTESIAN_POINT ( 'NONE',  ( 22.15312500061451573, 0.000000000000000000, 5.243569643749999010 ) ) ;
#53583 = CARTESIAN_POINT ( 'NONE',  ( -2.121784821874996840, 10.48437500061451821, 33.67503911421598417 ) ) ;
#53584 = CARTESIAN_POINT ( 'NONE',  ( 3.999999999999998668, 20.50624999877096499, 32.30940107675850470 ) ) ;
#53585 = CARTESIAN_POINT ( 'NONE',  ( 26.59687500061451360, 6.054752690667223547, 3.707466751127219781E-16 ) ) ;
#53586 = CARTESIAN_POINT ( 'NONE',  ( 29.29687500061451644, 6.054752690667223547, 3.707466751127219781E-16 ) ) ;
#53587 = CARTESIAN_POINT ( 'NONE',  ( 3.403125000614518836, -4.541064518000417216, -2.621784821875001281 ) ) ;
#53588 = CARTESIAN_POINT ( 'NONE',  ( 22.95937500061451786, 2.746126346562643317, 4.756430356249998326 ) ) ;
#53589 = CARTESIAN_POINT ( 'NONE',  ( 16.13437500061451502, 6.421520780324663323E-16, -5.243569643749999010 ) ) ;
#53590 = CARTESIAN_POINT ( 'NONE',  ( 9.834375000614514306, 5.492252693125287522, 3.363034840372157021E-16 ) ) ;
#53591 = CARTESIAN_POINT ( 'NONE',  ( 3.028125000614518392, 6.421520780324663323E-16, -5.243569643749999010 ) ) ;
#53592 = CARTESIAN_POINT ( 'NONE',  ( 4.959375000614516971, 4.541064518000418104, -2.621784821874998173 ) ) ;
#53593 = CARTESIAN_POINT ( 'NONE',  ( 17.78437500061451715, -4.541064518000419881, 2.621784821874995952 ) ) ;
#53594 = CARTESIAN_POINT ( 'NONE',  ( 9.918750001229033941, -5.773502691896255534, -1.060575238724906372E-15 ) ) ;
#53595 = CARTESIAN_POINT ( 'NONE',  ( 23.55000000000000071, 4.330127018922192761, -2.499999999999997780 ) ) ;
#53597 = ADVANCED_FACE ( 'NONE', ( #61306 ), #39510, .F. ) ;
#53596 = CARTESIAN_POINT ( 'NONE',  ( 26.37187500061451217, -6.054752690667223547, -1.112240025338166033E-15 ) ) ;
#53598 = CARTESIAN_POINT ( 'NONE',  ( 1.878215178125000495, 13.72812499938548392, 26.74683588394047007 ) ) ;
#53599 = CARTESIAN_POINT ( 'NONE',  ( 9.975000000000001421, 6.123233995736764310E-16, -4.999999999999998224 ) ) ;
#53600 = ORIENTED_EDGE ( 'NONE', *, *, #34883, .T. ) ;
#53601 = CARTESIAN_POINT ( 'NONE',  ( 8.849999999999999645, 0.000000000000000000, 4.999999999999998224 ) ) ;
#53602 = CARTESIAN_POINT ( 'NONE',  ( 8.784375000614515372, -2.746126346562642428, -4.756430356249999214 ) ) ;
#53603 = CARTESIAN_POINT ( 'NONE',  ( 21.92812500061451431, 6.421520780324663323E-16, -5.243569643749999010 ) ) ;
#53604 = CARTESIAN_POINT ( 'NONE',  ( 11.13750000000000284, -2.886751345948129988, 4.999999999999997335 ) ) ;
#53605 = CARTESIAN_POINT ( 'NONE',  ( 8.137500001229033941, -4.330127018922194537, 2.499999999999995559 ) ) ;
#53606 = CARTESIAN_POINT ( 'NONE',  ( 6.065625000614516260, -6.054752690667223547, -1.112240025338166033E-15 ) ) ;
#53607 =( BOUNDED_CURVE ( )  B_SPLINE_CURVE ( 2, ( #52058, #46516, #46881, #69055, #52418, #41693, #18775 ),
 .UNSPECIFIED., .F., .F. ) 
 B_SPLINE_CURVE_WITH_KNOTS ( ( 3, 2, 2, 3 ),
 ( 0.6750000000000000444, 0.6777777777777778123, 0.6805555555555555802, 0.6833333333333333481 ),
 .UNSPECIFIED. ) 
 CURVE ( )  GEOMETRIC_REPRESENTATION_ITEM ( )  RATIONAL_B_SPLINE_CURVE ( ( 1.000000000000000000, 0.8660254037844387076, 1.000000000000000000, 0.8660254037844387076, 1.000000000000000000, 0.8660254037844387076, 1.000000000000000000 ) ) 
 REPRESENTATION_ITEM ( '' )  );
#53608 = CARTESIAN_POINT ( 'NONE',  ( 19.79999999999999716, -4.330127018922190985, -2.500000000000001332 ) ) ;
#53610 = AXIS2_PLACEMENT_3D ( 'NONE', #7365, #2195, #29894 ) ;
#53609 = CARTESIAN_POINT ( 'NONE',  ( 19.37812500061451715, 4.541064518000418104, 2.621784821874999949 ) ) ;
#53611 = CARTESIAN_POINT ( 'NONE',  ( 23.55000000000000071, 4.330127018922192761, -2.499999999999997780 ) ) ;
#53612 = CARTESIAN_POINT ( 'NONE',  ( 23.88750000122903216, -4.330127018922194537, 2.499999999999995559 ) ) ;
#53613 = CARTESIAN_POINT ( 'NONE',  ( -1.878215178124999163, 19.99062499938548143, 26.74683588394047007 ) ) ;
#53614 = CARTESIAN_POINT ( 'NONE',  ( 4.575000000000002842, 6.123233995736764310E-16, -4.999999999999998224 ) ) ;
#53615 = VERTEX_POINT ( 'NONE', #56134 ) ;
#53616 = CARTESIAN_POINT ( 'NONE',  ( 20.20312500061451644, 4.541064518000418104, -2.621784821874998173 ) ) ;
#53617 = CARTESIAN_POINT ( 'NONE',  ( 26.01562500061451289, 3.027376345333613106, -5.243569643749998122 ) ) ;
#53618 = CARTESIAN_POINT ( 'NONE',  ( 24.38437500061451502, 4.541064518000418104, 2.621784821874999949 ) ) ;
#53619 = CARTESIAN_POINT ( 'NONE',  ( 8.250000000000000000, 4.330127018922192761, -2.499999999999997780 ) ) ;
#53620 = CARTESIAN_POINT ( 'NONE',  ( 13.07812500061451821, 4.541064518000418104, 2.621784821874999949 ) ) ;
#53621 = LINE ( 'NONE', #42174, #58432 ) ;
#53622 = CARTESIAN_POINT ( 'NONE',  ( 9.590625000614517504, -3.027376345333614438, 5.243569643749998122 ) ) ;
#53623 = CARTESIAN_POINT ( 'NONE',  ( 0.000000000000000000, 20.00000000000000000, -30.00000000000000000 ) ) ;
#53624 = CARTESIAN_POINT ( 'NONE',  ( -2.121784821874999949, 12.13437500061451857, 26.32496088578401938 ) ) ;
#53625 = CARTESIAN_POINT ( 'NONE',  ( 24.11250000122903359, 4.330127018922192761, -2.499999999999997780 ) ) ;
#53626 = CARTESIAN_POINT ( 'NONE',  ( 19.32187500061451857, 2.746126346562645981, -4.756430356249997438 ) ) ;
#53627 = CARTESIAN_POINT ( 'NONE',  ( 14.01562500061451644, 3.027376345333611329, 5.243569643749999010 ) ) ;
#53628 = CARTESIAN_POINT ( 'NONE',  ( 10.58437500061451964, -4.541064518000419881, 2.621784821874995952 ) ) ;
#53629 = CARTESIAN_POINT ( 'NONE',  ( 10.02187500061451964, 3.027376345333611329, 5.243569643749999010 ) ) ;
#53630 = CARTESIAN_POINT ( 'NONE',  ( 16.73437500061451644, 4.541064518000418104, 2.621784821874999949 ) ) ;
#53631 = ORIENTED_EDGE ( 'NONE', *, *, #27951, .F. ) ;
#53632 = CARTESIAN_POINT ( 'NONE',  ( 15.37500000000000000, 6.123233995736764310E-16, -4.999999999999998224 ) ) ;
#53633 = CARTESIAN_POINT ( 'NONE',  ( 20.99062500061451431, -3.027376345333610441, -5.243569643749999898 ) ) ;
#53634 = CARTESIAN_POINT ( 'NONE',  ( 16.13437500061451502, 6.421520780324663323E-16, -5.243569643749999010 ) ) ;
#53635 = CARTESIAN_POINT ( 'NONE',  ( 20.84062500061451573, -3.027376345333614438, 5.243569643749998122 ) ) ;
#53636 = CARTESIAN_POINT ( 'NONE',  ( 8.484601909799253346E-16, 11.56250000000000000, 34.61880215351700230 ) ) ;
#53637 = AXIS2_PLACEMENT_3D ( 'NONE', #21593, #66675, #39696 ) ;
#53638 = CARTESIAN_POINT ( 'NONE',  ( 26.50312500061451360, 4.541064518000418104, -2.621784821874998173 ) ) ;
#53639 = CARTESIAN_POINT ( 'NONE',  ( 6.675000001229034474, 2.886751345948126879, 4.999999999999999112 ) ) ;
#53640 = ORIENTED_EDGE ( 'NONE', *, *, #28075, .T. ) ;
#53641 = CARTESIAN_POINT ( 'NONE',  ( 5.437500001229035540, -4.330127018922194537, 2.499999999999995559 ) ) ;
#53642 = CARTESIAN_POINT ( 'NONE',  ( -3.999999999999999112, 17.75000000000000355, -30.00000000000000000 ) ) ;
#53643 = CARTESIAN_POINT ( 'NONE',  ( 24.90000000122903145, -2.886751345948125991, -5.000000000000000000 ) ) ;
#53644 = CARTESIAN_POINT ( 'NONE',  ( -3.756430356249999214, 14.74062499938548498, 27.83122392262697531 ) ) ;
#53645 = CARTESIAN_POINT ( 'NONE',  ( 6.909375000614518036, 0.000000000000000000, 5.243569643749999010 ) ) ;
#53646 = CARTESIAN_POINT ( 'NONE',  ( -10.00000000000000000, 0.000000000000000000, -50.00000000000000000 ) ) ;
#53647 = CARTESIAN_POINT ( 'NONE',  ( 14.69062500061451537, -3.027376345333610441, -5.243569643749999898 ) ) ;
#53648 = CARTESIAN_POINT ( 'NONE',  ( 9.721875000614517148, -6.054752690667223547, -1.112240025338166033E-15 ) ) ;
#53649 = CARTESIAN_POINT ( 'NONE',  ( 28.20000000122903216, 5.773502691896255534, 3.535250795749688894E-16 ) ) ;
#53650 = CARTESIAN_POINT ( 'NONE',  ( 16.32187500061451502, 3.027376345333611329, 5.243569643749999010 ) ) ;
#53651 = CARTESIAN_POINT ( 'NONE',  ( 3.871875000614519280, -6.054752690667223547, -1.112240025338166033E-15 ) ) ;
#53652 = CARTESIAN_POINT ( 'NONE',  ( 4.000000000000000000, 18.80000000000000071, 30.00000000000000000 ) ) ;
#53653 = CARTESIAN_POINT ( 'NONE',  ( 4.865625000614517859, 3.027376345333613106, -5.243569643749998122 ) ) ;
#53654 = CARTESIAN_POINT ( 'NONE',  ( 15.06562500061451537, -6.054752690667223547, -1.112240025338166033E-15 ) ) ;
#53655 = ORIENTED_EDGE ( 'NONE', *, *, #4530, .T. ) ;
#53656 = VECTOR ( 'NONE', #58569, 1000.000000000000000 ) ;
#53657 = CARTESIAN_POINT ( 'NONE',  ( 12.89062500061451821, -3.027376345333610441, -5.243569643749999898 ) ) ;
#53658 = CARTESIAN_POINT ( 'NONE',  ( 4.987500001229032698, -4.330127018922194537, 2.499999999999995559 ) ) ;
#53659 = AXIS2_PLACEMENT_3D ( 'NONE', #7784, #46952, #18848 ) ;
#53660 = CARTESIAN_POINT ( 'NONE',  ( 10.94062500061451537, -3.027376345333614438, 5.243569643749998122 ) ) ;
#53661 = CARTESIAN_POINT ( 'NONE',  ( 21.83437500061451786, -4.119189519843968306, 2.378215178124996054 ) ) ;
#53662 = CARTESIAN_POINT ( 'NONE',  ( 10.53750000000000320, 5.773502691896255534, 3.535250795749688894E-16 ) ) ;
#53663 = CARTESIAN_POINT ( 'NONE',  ( 5.700000001229033941, 5.773502691896255534, 3.535250795749688894E-16 ) ) ;
#53664 = CARTESIAN_POINT ( 'NONE',  ( 20.85000000000000142, 4.330127018922192761, -2.499999999999997780 ) ) ;
#53665 = EDGE_CURVE ( 'NONE', #50344, #51146, #28066, .T. ) ;
#53666 = CARTESIAN_POINT ( 'NONE',  ( 13.88437500061451679, 6.421520780324663323E-16, -5.243569643749999010 ) ) ;
#53667 = CARTESIAN_POINT ( 'NONE',  ( 16.61250000122903359, 0.000000000000000000, 4.999999999999998224 ) ) ;
#53668 = CARTESIAN_POINT ( 'NONE',  ( 22.01249999999999574, -5.773502691896255534, -1.060575238724906372E-15 ) ) ;
#53669 = CARTESIAN_POINT ( 'NONE',  ( 4.243569643749999898, 18.19062500061451360, -27.54997392385601529 ) ) ;
#53670 = CARTESIAN_POINT ( 'NONE',  ( 3.250662400336420177, 3.799104362746421604, 3.614115195980558859 ) ) ;
#53671 = LINE ( 'NONE', #8601, #59549 ) ;
#53672 = CARTESIAN_POINT ( 'NONE',  ( 23.13750000122903216, 6.123233995736764310E-16, -4.999999999999998224 ) ) ;
#53673 = CARTESIAN_POINT ( 'NONE',  ( 9.412500001229034297, 0.000000000000000000, 4.999999999999998224 ) ) ;
#53674 = CARTESIAN_POINT ( 'NONE',  ( 19.63125000122903430, 4.330127018922191873, 2.499999999999999556 ) ) ;
#53675 = CARTESIAN_POINT ( 'NONE',  ( 14.93437500061451750, 4.541064518000418104, 2.621784821874999949 ) ) ;
#53676 = CARTESIAN_POINT ( 'NONE',  ( 29.17500000000000071, -4.330127018922194537, 2.499999999999995559 ) ) ;
#53677 = CARTESIAN_POINT ( 'NONE',  ( 12.21562500061451573, 3.027376345333611329, 5.243569643749999010 ) ) ;
#53678 = CARTESIAN_POINT ( 'NONE',  ( 8.043750001229032165, -2.886751345948129988, 4.999999999999997335 ) ) ;
#53679 = CARTESIAN_POINT ( 'NONE',  ( 23.74687500061451573, -3.027376345333610441, -5.243569643749999898 ) ) ;
#53680 = CARTESIAN_POINT ( 'NONE',  ( 15.57187500061451679, 5.824947211148865298E-16, -4.756430356249998326 ) ) ;
#53681 = CARTESIAN_POINT ( 'NONE',  ( 10.52812500061451750, -4.541064518000419881, 2.621784821874995952 ) ) ;
#53682 = CARTESIAN_POINT ( 'NONE',  ( 12.19687500061451679, 6.054752690667223547, 3.707466751127219781E-16 ) ) ;
#53683 = VERTEX_POINT ( 'NONE', #67949 ) ;
#53684 = CARTESIAN_POINT ( 'NONE',  ( 24.87187500061451573, 3.027376345333611329, 5.243569643749999010 ) ) ;
#53685 = CARTESIAN_POINT ( 'NONE',  ( 27.17812500061451786, -4.541064518000419881, 2.621784821874995952 ) ) ;
#53686 = LINE ( 'NONE', #14518, #7770 ) ;
#53687 = AXIS2_PLACEMENT_3D ( 'NONE', #43049, #70753, #20128 ) ;
#53688 = CARTESIAN_POINT ( 'NONE',  ( 6.487499999999999822, 5.773502691896255534, 3.535250795749688894E-16 ) ) ;
#53689 = CARTESIAN_POINT ( 'NONE',  ( 18.15000000122903501, -2.886751345948125991, -5.000000000000000000 ) ) ;
#53690 = CARTESIAN_POINT ( 'NONE',  ( 4.898587196589411843E-16, 20.00000000000000000, 33.99999999999999289 ) ) ;
#53691 = CARTESIAN_POINT ( 'NONE',  ( 29.21250000122903145, 0.000000000000000000, 4.999999999999998224 ) ) ;
#53692 = ORIENTED_EDGE ( 'NONE', *, *, #55194, .T. ) ;
#53693 = CARTESIAN_POINT ( 'NONE',  ( 15.56250000000000000, 2.886751345948126879, 4.999999999999999112 ) ) ;
#53694 = CARTESIAN_POINT ( 'NONE',  ( 19.04999999999999716, 4.330127018922192761, -2.499999999999997780 ) ) ;
#53695 = CARTESIAN_POINT ( 'NONE',  ( 13.00312500061451537, 4.541064518000418104, -2.621784821874998173 ) ) ;
#53697 = ORIENTED_EDGE ( 'NONE', *, *, #22115, .F. ) ;
#53696 = VECTOR ( 'NONE', #2184, 1000.000000000000000 ) ;
#53698 = CARTESIAN_POINT ( 'NONE',  ( 10.31250000000000178, -5.773502691896255534, -1.060575238724906372E-15 ) ) ;
#53699 = CARTESIAN_POINT ( 'NONE',  ( 9.001249775931846008E-16, 15.92187500061451821, -25.09994784771203058 ) ) ;
#53700 = CARTESIAN_POINT ( 'NONE',  ( 5.128125000614516260, -4.541064518000419881, 2.621784821874995952 ) ) ;
#53701 = CARTESIAN_POINT ( 'NONE',  ( 19.74375000122903145, -2.886751345948130876, 4.999999999999996447 ) ) ;
#53702 = CARTESIAN_POINT ( 'NONE',  ( 12.48750000000000249, -2.886751345948129988, 4.999999999999997335 ) ) ;
#53703 = CARTESIAN_POINT ( 'NONE',  ( 29.10937500061451999, 2.746126346562645981, -4.756430356249997438 ) ) ;
#53704 = ORIENTED_EDGE ( 'NONE', *, *, #61290, .T. ) ;
#53705 = CARTESIAN_POINT ( 'NONE',  ( -4.243569643749999898, 15.26562500061451644, 27.54997392385601529 ) ) ;
#53706 = CARTESIAN_POINT ( 'NONE',  ( 27.14062500061451644, -3.027376345333614438, 5.243569643749998122 ) ) ;
#53707 = CYLINDRICAL_SURFACE ( 'NONE', #30124, 4.000000000000000000 ) ;
#53708 = CARTESIAN_POINT ( 'NONE',  ( 3.756430356249998770, 18.45312499938548001, 32.16877607737302469 ) ) ;
#53709 = CARTESIAN_POINT ( 'NONE',  ( 23.55937500061451573, 0.000000000000000000, 5.243569643749999010 ) ) ;
#53710 = CARTESIAN_POINT ( 'NONE',  ( 19.26562500061451644, 3.027376345333613106, -5.243569643749998122 ) ) ;
#53711 = EDGE_CURVE ( 'NONE', #58137, #58126, #28532, .T. ) ;
#53712 = CARTESIAN_POINT ( 'NONE',  ( -3.000416591977282496E-16, 14.29062500061459140, -34.90005215228797653 ) ) ;
#53713 = CARTESIAN_POINT ( 'NONE',  ( 23.10000000122903074, -2.886751345948125991, -5.000000000000000000 ) ) ;
#53714 = CARTESIAN_POINT ( 'NONE',  ( 5.203125000614518214, -4.541064518000417216, -2.621784821875001281 ) ) ;
#53715 = CARTESIAN_POINT ( 'NONE',  ( 26.63437500061451857, 4.119189519843966529, 2.378215178124999607 ) ) ;
#53716 = CARTESIAN_POINT ( 'NONE',  ( 22.45312500061451644, 4.541064518000418104, -2.621784821874998173 ) ) ;
#53717 = CARTESIAN_POINT ( 'NONE',  ( 11.37187500061451750, 2.746126346562643317, 4.756430356249998326 ) ) ;
#53718 = CARTESIAN_POINT ( 'NONE',  ( -3.756430356250001434, 15.60312499938548392, 32.16877607737301048 ) ) ;
#53719 = CARTESIAN_POINT ( 'NONE',  ( 17.59687500061451715, 6.054752690667223547, 3.707466751127219781E-16 ) ) ;
#53720 = CARTESIAN_POINT ( 'NONE',  ( 17.07187500061451502, 3.027376345333613106, -5.243569643749998122 ) ) ;
#53721 = CARTESIAN_POINT ( 'NONE',  ( 23.93437500061451573, 4.541064518000418104, 2.621784821874999949 ) ) ;
#53722 = CARTESIAN_POINT ( 'NONE',  ( 2.121784821874999061, 14.75937500061451679, 26.32496088578401583 ) ) ;
#53723 = CARTESIAN_POINT ( 'NONE',  ( 5.015625000614518214, 3.027376345333611329, 5.243569643749999010 ) ) ;
#53724 = CARTESIAN_POINT ( 'NONE',  ( 16.50000000122903288, 5.773502691896255534, 3.535250795749688401E-16 ) ) ;
#53725 = CARTESIAN_POINT ( 'NONE',  ( 28.75312500061451715, 4.541064518000418104, -2.621784821874998173 ) ) ;
#53726 = CARTESIAN_POINT ( 'NONE',  ( -2.000000000000001776, 15.05000000000000071, 33.46410161513775705 ) ) ;
#53727 = CARTESIAN_POINT ( 'NONE',  ( 4.134375000614517681, 4.541064518000418104, 2.621784821874999949 ) ) ;
#53728 = CARTESIAN_POINT ( 'NONE',  ( 3.665625000614517681, 3.027376345333611329, 5.243569643749999010 ) ) ;
#53729 = CARTESIAN_POINT ( 'NONE',  ( 7.509375000614517681, -4.541064518000417216, -2.621784821875001281 ) ) ;
#53730 =( LENGTH_UNIT ( ) NAMED_UNIT ( * ) SI_UNIT ( .MILLI., .METRE. ) );
#53731 = CARTESIAN_POINT ( 'NONE',  ( 14.73750000122903359, 4.330127018922191873, 2.499999999999999556 ) ) ;
#53732 = CARTESIAN_POINT ( 'NONE',  ( 29.54062500061451502, -3.027376345333610441, -5.243569643749999898 ) ) ;
#53733 = CARTESIAN_POINT ( 'NONE',  ( 12.90000000122903145, 5.773502691896255534, 3.535250795749688894E-16 ) ) ;
#53734 = CARTESIAN_POINT ( 'NONE',  ( 6.253125000614517148, 4.541064518000418104, -2.621784821874998173 ) ) ;
#53735 = CARTESIAN_POINT ( 'NONE',  ( -4.000000000000000000, 13.11874999877096570, 30.00000000000000000 ) ) ;
#53736 = CARTESIAN_POINT ( 'NONE',  ( 20.08125000122903359, 4.330127018922191873, 2.499999999999999556 ) ) ;
#53737 = CARTESIAN_POINT ( 'NONE',  ( 14.78437500061451715, 6.421520780324663323E-16, -5.243569643749999010 ) ) ;
#53738 = CARTESIAN_POINT ( 'NONE',  ( 7.612500000000000711, -5.773502691896255534, -1.060575238724906372E-15 ) ) ;
#53739 = EDGE_LOOP ( 'NONE', ( #59586, #67529, #17972, #35081 ) ) ;
#53740 = CARTESIAN_POINT ( 'NONE',  ( 23.05312500061451431, 0.000000000000000000, 5.243569643749999010 ) ) ;
#53741 = CARTESIAN_POINT ( 'NONE',  ( 7.003125000614518036, -4.541064518000417216, -2.621784821875001281 ) ) ;
#53742 = CARTESIAN_POINT ( 'NONE',  ( 24.68437500061451573, 6.421520780324663323E-16, -5.243569643749999010 ) ) ;
#53743 = CARTESIAN_POINT ( 'NONE',  ( 6.440625000614517148, -3.027376345333614438, 5.243569643749998122 ) ) ;
#53744 = CARTESIAN_POINT ( 'NONE',  ( 8.212500001229035007, -4.330127018922190985, -2.500000000000001332 ) ) ;
#53745 = CARTESIAN_POINT ( 'NONE',  ( 22.82812500061451644, 6.421520780324663323E-16, -5.243569643749999010 ) ) ;
#53746 = CARTESIAN_POINT ( 'NONE',  ( -2.121784821874996840, 11.77812500061451750, -26.32496088578401583 ) ) ;
#53747 = CARTESIAN_POINT ( 'NONE',  ( 11.51250000122903216, 4.330127018922192761, -2.499999999999997780 ) ) ;
#53748 = CARTESIAN_POINT ( 'NONE',  ( 20.57812500061451644, 6.421520780324663323E-16, -5.243569643749999010 ) ) ;
#53749 = CARTESIAN_POINT ( 'NONE',  ( 17.76562500061451644, -6.054752690667223547, -1.112240025338166033E-15 ) ) ;
#53750 = CARTESIAN_POINT ( 'NONE',  ( 27.49687500061451217, 5.492252693125287522, 3.363034840372157021E-16 ) ) ;
#53751 = CARTESIAN_POINT ( 'NONE',  ( 17.39999999999999858, 0.000000000000000000, 4.999999999999998224 ) ) ;
#53752 = CARTESIAN_POINT ( 'NONE',  ( 14.77500000122903501, 2.886751345948126879, 4.999999999999999112 ) ) ;
#53753 = AXIS2_PLACEMENT_3D ( 'NONE', #28185, #17076, #39637 ) ;
#53754 = CARTESIAN_POINT ( 'NONE',  ( 9.440625000614517148, 6.054752690667223547, 3.707466751127219781E-16 ) ) ;
#53755 = CARTESIAN_POINT ( 'NONE',  ( 13.90312500061451750, 4.541064518000418104, -2.621784821874998173 ) ) ;
#53756 = VECTOR ( 'NONE', #12784, 1000.000000000000000 ) ;
#53757 = CARTESIAN_POINT ( 'NONE',  ( 23.96250000122903145, -4.330127018922190985, -2.500000000000001332 ) ) ;
#53758 = VECTOR ( 'NONE', #55520, 1000.000000000000000 ) ;
#53759 = CARTESIAN_POINT ( 'NONE',  ( 21.12187500061451573, 3.027376345333613106, -5.243569643749998122 ) ) ;
#53760 = CARTESIAN_POINT ( 'NONE',  ( 20.82187500061451857, 3.027376345333611329, 5.243569643749999010 ) ) ;
#53761 = CARTESIAN_POINT ( 'NONE',  ( 3.564913708944925208, 3.505916797073983293, -3.899182909318817725 ) ) ;
#53762 = CARTESIAN_POINT ( 'NONE',  ( 7.162500001229032520, 0.000000000000000000, 4.999999999999998224 ) ) ;
#53763 = CARTESIAN_POINT ( 'NONE',  ( 7.546875000614517326, -3.027376345333610441, -5.243569643749999898 ) ) ;
#53764 = CARTESIAN_POINT ( 'NONE',  ( 23.29687500061451644, -3.027376345333610441, -5.243569643749999898 ) ) ;
#53765 = CARTESIAN_POINT ( 'NONE',  ( 4.683223236373093457, -1.751405183929441556, 4.942428804804532838 ) ) ;
#53766 = CARTESIAN_POINT ( 'NONE',  ( 19.04062500061451146, -3.027376345333614438, 5.243569643749998122 ) ) ;
#53767 = CARTESIAN_POINT ( 'NONE',  ( 25.24687500061451573, 6.054752690667223547, 3.707466751127219781E-16 ) ) ;
#53768 = CARTESIAN_POINT ( 'NONE',  ( -3.756430356250000102, 20.62812499938548072, 30.00000000000000000 ) ) ;
#53769 = CARTESIAN_POINT ( 'NONE',  ( 23.13749999999999929, 5.773502691896255534, 3.535250795749688401E-16 ) ) ;
#53770 = CARTESIAN_POINT ( 'NONE',  ( 1.071796769724491893, 15.63259618943233598, 33.99999999999999289 ) ) ;
#53771 = CARTESIAN_POINT ( 'NONE',  ( 4.471875000614518925, 3.027376345333613106, -5.243569643749998122 ) ) ;
#53772 = CARTESIAN_POINT ( 'NONE',  ( 18.32812500061451644, 6.421520780324663323E-16, -5.243569643749999010 ) ) ;
#53773 = ORIENTED_EDGE ( 'NONE', *, *, #16481, .F. ) ;
#53774 = DIRECTION ( 'NONE',  ( 0.000000000000000000, 0.000000000000000000, 1.000000000000000000 ) ) ;
#53775 = CARTESIAN_POINT ( 'NONE',  ( 24.40312500061451573, 0.000000000000000000, 5.243569643749999010 ) ) ;
#53776 = CARTESIAN_POINT ( 'NONE',  ( 4.342984975361706468, -2.477595912125914790, -4.621313785610477787 ) ) ;
#53777 = CARTESIAN_POINT ( 'NONE',  ( 28.01249999999999574, 2.886751345948142866, -4.999999999999973355 ) ) ;
#53778 = CARTESIAN_POINT ( 'NONE',  ( 14.28750000000000142, -2.886751345948129988, 4.999999999999997335 ) ) ;
#53779 = CARTESIAN_POINT ( 'NONE',  ( 24.48750000122903359, 6.123233995736764310E-16, -4.999999999999998224 ) ) ;
#53780 = CARTESIAN_POINT ( 'NONE',  ( 18.25312500061451715, -4.541064518000417216, -2.621784821875001281 ) ) ;
#53781 = ORIENTED_EDGE ( 'NONE', *, *, #68789, .T. ) ;
#53782 = CARTESIAN_POINT ( 'NONE',  ( 22.42500000000000071, -4.330127018922194537, 2.499999999999995559 ) ) ;
#53783 = CARTESIAN_POINT ( 'NONE',  ( 24.64687500061451431, -3.027376345333610441, -5.243569643749999898 ) ) ;
#53784 = VERTEX_POINT ( 'NONE', #17322 ) ;
#53785 = CYLINDRICAL_SURFACE ( 'NONE', #28910, 5.000000000000000000 ) ;
#53786 = CARTESIAN_POINT ( 'NONE',  ( 12.36562500061451608, -6.054752690667223547, -1.112240025338166033E-15 ) ) ;
#53787 = CARTESIAN_POINT ( 'NONE',  ( 4.528125000614516615, 4.541064518000418104, 2.621784821874999949 ) ) ;
#53788 = CARTESIAN_POINT ( 'NONE',  ( 16.65937500061451715, 2.746126346562643317, 4.756430356249998326 ) ) ;
#53789 = CARTESIAN_POINT ( 'NONE',  ( 27.32812500061451644, 6.421520780324663323E-16, -5.243569643749999010 ) ) ;
#53790 = CARTESIAN_POINT ( 'NONE',  ( 13.35000000122903430, 5.773502691896255534, 3.535250795749688894E-16 ) ) ;
#53791 = AXIS2_PLACEMENT_3D ( 'NONE', #36493, #70481, #69751 ) ;
#53792 = CARTESIAN_POINT ( 'NONE',  ( 19.76250000000000639, -5.773502691896255534, -1.060575238724906372E-15 ) ) ;
#53793 = CARTESIAN_POINT ( 'NONE',  ( 25.80000000000000071, 4.330127018922192761, -2.499999999999997780 ) ) ;
#53794 = CARTESIAN_POINT ( 'NONE',  ( 3.271875000614519635, 3.027376345333611329, 5.243569643749999010 ) ) ;
#53795 = CARTESIAN_POINT ( 'NONE',  ( 5.746875000614517504, -3.027376345333610441, -5.243569643749999898 ) ) ;
#53796 = CARTESIAN_POINT ( 'NONE',  ( 16.65937500061452070, 4.541064518000418104, -2.621784821874998173 ) ) ;
#53797 = CARTESIAN_POINT ( 'NONE',  ( 45.00000000000000000, 0.000000000000000000, 0.000000000000000000 ) ) ;
#53798 = VERTEX_POINT ( 'NONE', #22505 ) ;
#53799 = CARTESIAN_POINT ( 'NONE',  ( 29.16562500061451502, 3.027376345333613106, -5.243569643749998122 ) ) ;
#53800 = CARTESIAN_POINT ( 'NONE',  ( 26.59687500061451360, 6.054752690667223547, 3.707466751127219781E-16 ) ) ;
#53801 = CARTESIAN_POINT ( 'NONE',  ( 16.96875000122903288, 2.886751345948126879, 4.999999999999998224 ) ) ;
#53802 = CARTESIAN_POINT ( 'NONE',  ( 15.07499999999999929, 4.330127018922191873, 2.499999999999999556 ) ) ;
#53803 = CARTESIAN_POINT ( 'NONE',  ( 14.12812500061451715, -4.541064518000419881, 2.621784821874995952 ) ) ;
#53804 = CARTESIAN_POINT ( 'NONE',  ( -1.071796769724490339, 19.38259618943233775, 26.00000000000000000 ) ) ;
#53805 = DIRECTION ( 'NONE',  ( -0.000000000000000000, -1.000000000000000000, -0.000000000000000000 ) ) ;
#53806 = LINE ( 'NONE', #69700, #11538 ) ;
#53807 = CARTESIAN_POINT ( 'NONE',  ( 19.08750000122903145, 6.123233995736764310E-16, -4.999999999999998224 ) ) ;
#53808 = DIRECTION ( 'NONE',  ( -1.000000000000000000, 0.000000000000000000, 0.000000000000000000 ) ) ;
#53809 = CARTESIAN_POINT ( 'NONE',  ( 17.93437500061451928, 5.824947211148865298E-16, -4.756430356249998326 ) ) ;
#53810 = CARTESIAN_POINT ( 'NONE',  ( 7.640625000614517326, 6.054752690667223547, 3.707466751127219781E-16 ) ) ;
#53811 = CARTESIAN_POINT ( 'NONE',  ( 23.10937500061451644, 0.000000000000000000, 5.243569643749999010 ) ) ;
#53812 = CARTESIAN_POINT ( 'NONE',  ( -4.243569643749999898, 16.70937500061451786, 30.00000000000000000 ) ) ;
#53813 = EDGE_CURVE ( 'NONE', #67359, #63939, #38469, .T. ) ;
#53814 = CARTESIAN_POINT ( 'NONE',  ( 25.09687500061451715, -3.027376345333610441, -5.243569643749999898 ) ) ;
#53815 = CARTESIAN_POINT ( 'NONE',  ( 4.687500000000000000, 5.773502691896255534, 3.535250795749688894E-16 ) ) ;
#53816 = CARTESIAN_POINT ( 'NONE',  ( 4.000000000000000000, 10.40000000122903501, 32.30940107675849049 ) ) ;
#53817 = CARTESIAN_POINT ( 'NONE',  ( 11.20312500061451644, 4.541064518000418104, -2.621784821874998173 ) ) ;
#53818 = CARTESIAN_POINT ( 'NONE',  ( 3.637500001229036162, -4.330127018922194537, 2.499999999999995559 ) ) ;
#53819 = CARTESIAN_POINT ( 'NONE',  ( 8.371875000614515727, -6.054752690667223547, -1.112240025338166033E-15 ) ) ;
#53820 = CYLINDRICAL_SURFACE ( 'NONE', #21839, 1.500000000000000444 ) ;
#53821 = ORIENTED_EDGE ( 'NONE', *, *, #62622, .F. ) ;
#53822 = CARTESIAN_POINT ( 'NONE',  ( 10.22812500061451679, 6.421520780324663323E-16, -5.243569643749999010 ) ) ;
#53823 = CARTESIAN_POINT ( 'NONE',  ( 14.48437500061451821, 4.541064518000418104, 2.621784821874999949 ) ) ;
#53824 = DIRECTION ( 'NONE',  ( 0.000000000000000000, 6.195440985631455317E-17, 1.000000000000000000 ) ) ;
#53825 = CARTESIAN_POINT ( 'NONE',  ( 22.65000000122903856, -2.886751345948125991, -5.000000000000000000 ) ) ;
#53826 = CARTESIAN_POINT ( 'NONE',  ( 10.28437500061451715, 6.421520780324663323E-16, -5.243569643749999010 ) ) ;
#53827 = CARTESIAN_POINT ( 'NONE',  ( 11.87812500061451537, -4.541064518000419881, 2.621784821874995952 ) ) ;
#53828 = CARTESIAN_POINT ( 'NONE',  ( 27.16875000122903216, 2.886751345948129099, -4.999999999999998224 ) ) ;
#53829 = CARTESIAN_POINT ( 'NONE',  ( 20.67187500061451289, 3.027376345333613106, -5.243569643749998122 ) ) ;
#53830 = CARTESIAN_POINT ( 'NONE',  ( 14.24999999999999822, 0.000000000000000000, 4.999999999999998224 ) ) ;
#53831 =( BOUNDED_CURVE ( )  B_SPLINE_CURVE ( 2, ( #6809, #41161, #24146, #1640, #63670, #41872, #13794 ),
 .UNSPECIFIED., .F., .F. ) 
 B_SPLINE_CURVE_WITH_KNOTS ( ( 3, 2, 2, 3 ),
 ( 0.2333333333333333648, 0.2361111111111111327, 0.2388888888888889284, 0.2416666666666666963 ),
 .UNSPECIFIED. ) 
 CURVE ( )  GEOMETRIC_REPRESENTATION_ITEM ( )  RATIONAL_B_SPLINE_CURVE ( ( 0.9999999999999986677, 0.8660254037844400399, 1.000000000000000000, 0.8660254037844387076, 1.000000000000000000, 0.8660254037844373753, 1.000000000000001332 ) ) 
 REPRESENTATION_ITEM ( '' )  );
#53832 = CARTESIAN_POINT ( 'NONE',  ( -5.810221930991193690E-16, 12.68750000000000000, 26.00000000000000355 ) ) ;
#53833 = CARTESIAN_POINT ( 'NONE',  ( -4.243569643749998122, 14.04687500061451999, -27.54997392385601174 ) ) ;
#53834 = CARTESIAN_POINT ( 'NONE',  ( 16.65937500061452070, 4.541064518000418104, -2.621784821874998173 ) ) ;
#53835 = CARTESIAN_POINT ( 'NONE',  ( 16.05000000122903359, 5.773502691896255534, 3.535250795749688894E-16 ) ) ;
#53836 = CARTESIAN_POINT ( 'NONE',  ( 12.30937500061451573, 0.000000000000000000, 5.243569643749999010 ) ) ;
#53837 = CARTESIAN_POINT ( 'NONE',  ( -2.121784821874996840, 18.52812500061451928, -26.32496088578401583 ) ) ;
#53838 = CARTESIAN_POINT ( 'NONE',  ( 16.38750000122903216, 6.123233995736764310E-16, -4.999999999999998224 ) ) ;
#53839 = CARTESIAN_POINT ( 'NONE',  ( 11.54062500061451857, -3.027376345333610441, -5.243569643749999898 ) ) ;
#53840 = ORIENTED_EDGE ( 'NONE', *, *, #14279, .F. ) ;
#53841 = CARTESIAN_POINT ( 'NONE',  ( 14.88750000000000107, -2.886751345948125991, -5.000000000000000000 ) ) ;
#53842 = CARTESIAN_POINT ( 'NONE',  ( 4.711411573247316298, 1.674097066322985938, -4.711411573247316298 ) ) ;
#53843 = CARTESIAN_POINT ( 'NONE',  ( 11.14687500061451608, -3.027376345333610441, -5.243569643749999898 ) ) ;
#53844 = CARTESIAN_POINT ( 'NONE',  ( 3.049098432412538973, 3.962700941209165606, -3.321219890071966496 ) ) ;
#53845 = CARTESIAN_POINT ( 'NONE',  ( 12.15000000122903501, -2.886751345948129988, 4.999999999999997335 ) ) ;
#53846 = CARTESIAN_POINT ( 'NONE',  ( 21.00000000122903288, 5.773502691896255534, 3.535250795749688894E-16 ) ) ;
#53847 = CARTESIAN_POINT ( 'NONE',  ( 17.35312500061451502, -4.541064518000417216, -2.621784821875001281 ) ) ;
#53848 = CARTESIAN_POINT ( 'NONE',  ( 19.67812500061451786, 6.421520780324663323E-16, -5.243569643749999010 ) ) ;
#53849 = CARTESIAN_POINT ( 'NONE',  ( 26.81250000122903288, 4.330127018922192761, -2.499999999999997780 ) ) ;
#53850 = EDGE_CURVE ( 'NONE', #27675, #32725, #165, .T. ) ;
#53851 =( BOUNDED_CURVE ( )  B_SPLINE_CURVE ( 2, ( #3603, #43490, #42392, #26125, #71189, #66014, #14304 ),
 .UNSPECIFIED., .F., .F. ) 
 B_SPLINE_CURVE_WITH_KNOTS ( ( 3, 2, 2, 3 ),
 ( 0.9083333333333334370, 0.9111111111111112049, 0.9138888888888888618, 0.9161926342374220322 ),
 .UNSPECIFIED. ) 
 CURVE ( )  GEOMETRIC_REPRESENTATION_ITEM ( )  RATIONAL_B_SPLINE_CURVE ( ( 0.9999999999999946709, 0.8660254037844440367, 1.000000000000000000, 0.8660254037844387076, 1.000000000000000000, 0.8888883929728443878, 0.9620772364026252133 ) ) 
 REPRESENTATION_ITEM ( '' )  );
#53852 = CARTESIAN_POINT ( 'NONE',  ( 4.490625000614516971, 6.054752690667223547, 3.707466751127219781E-16 ) ) ;
#53853 = CARTESIAN_POINT ( 'NONE',  ( 24.75000000000000000, -4.330127018922190985, -2.500000000000001332 ) ) ;
#53854 = CARTESIAN_POINT ( 'NONE',  ( 17.56875000122903074, -5.773502691896255534, -1.060575238724906372E-15 ) ) ;
#53855 = AXIS2_PLACEMENT_3D ( 'NONE', #53201, #2597, #25117 ) ;
#53856 = CARTESIAN_POINT ( 'NONE',  ( 28.27499999999999858, -4.330127018922194537, 2.499999999999995559 ) ) ;
#53857 = CARTESIAN_POINT ( 'NONE',  ( 27.64687500061452141, -3.027376345333614438, 5.243569643749998122 ) ) ;
#53858 = CARTESIAN_POINT ( 'NONE',  ( -3.999999999999999112, 15.94999999999999929, 30.00000000000000000 ) ) ;
#53859 = CARTESIAN_POINT ( 'NONE',  ( -2.121784821874996840, 13.18437500061451750, -26.32496088578401583 ) ) ;
#53860 = CARTESIAN_POINT ( 'NONE',  ( 4.275000001229035895, 2.886751345948129099, -4.999999999999998224 ) ) ;
#53861 = CARTESIAN_POINT ( 'NONE',  ( 3.637500000000001954, -2.886751345948125991, -5.000000000000000000 ) ) ;
#53862 = CARTESIAN_POINT ( 'NONE',  ( 16.42500000000000071, 4.330127018922191873, 2.499999999999999556 ) ) ;
#53863 = CARTESIAN_POINT ( 'NONE',  ( 8.371875000614515727, -6.054752690667223547, -1.112240025338166033E-15 ) ) ;
#53864 = CARTESIAN_POINT ( 'NONE',  ( 25.07812500061451644, 6.421520780324663323E-16, -5.243569643749999010 ) ) ;
#53865 =( BOUNDED_CURVE ( )  B_SPLINE_CURVE ( 2, ( #39394, #6492, #51199, #67831, #17204, #56727, #50116, #68197, #72645 ),
 .UNSPECIFIED., .F., .F. ) 
 B_SPLINE_CURVE_WITH_KNOTS ( ( 3, 2, 2, 2, 3 ),
 ( 0.7717391304347825942, 0.7753623188405797118, 0.7826086956521739468, 0.7898550724637680709, 0.7934782608695651884 ),
 .UNSPECIFIED. ) 
 CURVE ( )  GEOMETRIC_REPRESENTATION_ITEM ( )  RATIONAL_B_SPLINE_CURVE ( ( 0.9330127018922194093, 0.9330127018922194093, 1.000000000000000000, 0.8660254037844387076, 1.000000000000000000, 0.8660254037844387076, 1.000000000000000000, 0.9330127018922194093, 0.9330127018922194093 ) ) 
 REPRESENTATION_ITEM ( '' )  );
#53866 = CARTESIAN_POINT ( 'NONE',  ( 0.000000000000000000, 20.00000000000000000, 30.00000000000000000 ) ) ;
#53867 = FACE_OUTER_BOUND ( 'NONE', #10378, .T. ) ;
#53868 = CARTESIAN_POINT ( 'NONE',  ( 6.496875000614517504, -3.027376345333614438, 5.243569643749998122 ) ) ;
#53869 = CARTESIAN_POINT ( 'NONE',  ( 8.034375000614518925, 6.421520780324663323E-16, -5.243569643749999010 ) ) ;
#53870 = CARTESIAN_POINT ( 'NONE',  ( 4.312500000000000000, 2.886751345948126879, 4.999999999999999112 ) ) ;
#53871 = CARTESIAN_POINT ( 'NONE',  ( -3.000416591977282496E-16, 13.39062500061459460, 25.09994784771203058 ) ) ;
#53872 = CARTESIAN_POINT ( 'NONE',  ( -3.999999999999999112, 17.71249999999999858, -32.30940107675850470 ) ) ;
#53873 = CARTESIAN_POINT ( 'NONE',  ( 4.162499999999999645, 2.886751345948129099, -4.999999999999998224 ) ) ;
#53874 = CARTESIAN_POINT ( 'NONE',  ( 16.28437500061451715, -2.746126346562646425, 4.756430356249996549 ) ) ;
#53875 = ORIENTED_EDGE ( 'NONE', *, *, #49176, .F. ) ;
#53876 = CARTESIAN_POINT ( 'NONE',  ( 19.71562500061451928, 3.027376345333613106, -5.243569643749998122 ) ) ;
#53877 = CARTESIAN_POINT ( 'NONE',  ( 10.22812500061451679, 6.421520780324663323E-16, -5.243569643749999010 ) ) ;
#53878 = CARTESIAN_POINT ( 'NONE',  ( 23.78437500061451360, 5.492252693125287522, 3.363034840372157021E-16 ) ) ;
#53879 = CARTESIAN_POINT ( 'NONE',  ( 6.309375000614517504, 4.541064518000418104, -2.621784821874998173 ) ) ;
#53880 = CARTESIAN_POINT ( 'NONE',  ( 26.32499999999999929, 4.330127018922191873, 2.499999999999999556 ) ) ;
#53881 = CARTESIAN_POINT ( 'NONE',  ( 19.95000000122903572, -2.886751345948125991, -5.000000000000000000 ) ) ;
#53882 = CARTESIAN_POINT ( 'NONE',  ( 28.11562500061451431, -6.054752690667223547, -1.112240025338166033E-15 ) ) ;
#53883 = CARTESIAN_POINT ( 'NONE',  ( 15.99375000122903145, 5.773502691896255534, 3.535250795749688401E-16 ) ) ;
#53884 = CARTESIAN_POINT ( 'NONE',  ( 8.371875000614515727, -6.054752690667223547, -1.112240025338166033E-15 ) ) ;
#53885 = CARTESIAN_POINT ( 'NONE',  ( 14.70937500061451786, -4.541064518000417216, -2.621784821875001281 ) ) ;
#53886 = CARTESIAN_POINT ( 'NONE',  ( 25.99687500061451928, -3.027376345333610441, -5.243569643749999898 ) ) ;
#53887 = AXIS2_PLACEMENT_3D ( 'NONE', #46845, #57552, #24297 ) ;
#53888 = LINE ( 'NONE', #30612, #24153 ) ;
#53889 = CARTESIAN_POINT ( 'NONE',  ( 12.75000000000000178, 4.330127018922192761, -2.499999999999997780 ) ) ;
#53890 = CARTESIAN_POINT ( 'NONE',  ( 20.18437500061451573, 6.421520780324663323E-16, -5.243569643749999010 ) ) ;
#53891 = CARTESIAN_POINT ( 'NONE',  ( 12.53437500061451537, 6.421520780324663323E-16, -5.243569643749999010 ) ) ;
#53892 = CARTESIAN_POINT ( 'NONE',  ( 3.756430356250000546, 13.57812499938548711, 27.83122392262697886 ) ) ;
#53893 = CARTESIAN_POINT ( 'NONE',  ( 24.52499999999999858, 4.330127018922191873, 2.499999999999999556 ) ) ;
#53894 = CARTESIAN_POINT ( 'NONE',  ( -1.999999999999999112, 14.00000000000000000, 26.53589838486224650 ) ) ;
#53895 = CARTESIAN_POINT ( 'NONE',  ( 4.243569643749999898, 11.49687500061451928, -27.54997392385601529 ) ) ;
#53896 = CARTESIAN_POINT ( 'NONE',  ( 25.32187500061451857, 2.746126346562643317, 4.756430356249998326 ) ) ;
#53897 = CARTESIAN_POINT ( 'NONE',  ( 15.62812500061451537, 6.421520780324663323E-16, -5.243569643749999010 ) ) ;
#53898 = CARTESIAN_POINT ( 'NONE',  ( 3.787500000000002753, 5.773502691896255534, 3.535250795749688894E-16 ) ) ;
#53899 = LINE ( 'NONE', #65700, #32500 ) ;
#53900 = CARTESIAN_POINT ( 'NONE',  ( 0.000000000000000000, 20.00000000000000000, 30.00000000000000000 ) ) ;
#53901 = CARTESIAN_POINT ( 'NONE',  ( 11.84999999999999964, 4.330127018922192761, -2.499999999999997780 ) ) ;
#53902 = CARTESIAN_POINT ( 'NONE',  ( 3.999999999999999112, 17.18750000122903288, 30.00000000000000000 ) ) ;
#53903 = CARTESIAN_POINT ( 'NONE',  ( 11.85000000122903430, -2.886751345948125991, -5.000000000000000000 ) ) ;
#53904 = CARTESIAN_POINT ( 'NONE',  ( 22.32187500061451502, -6.054752690667223547, -1.112240025338166033E-15 ) ) ;
#53905 = CARTESIAN_POINT ( 'NONE',  ( 15.45937500061451608, 0.000000000000000000, 5.243569643749999010 ) ) ;
#53906 = AXIS2_PLACEMENT_3D ( 'NONE', #71120, #59658, #65205 ) ;
#53907 = EDGE_LOOP ( 'NONE', ( #23434, #67300, #49700, #7395 ) ) ;
#53908 = CARTESIAN_POINT ( 'NONE',  ( 17.87812500061451715, 6.421520780324663323E-16, -5.243569643749999010 ) ) ;
#53909 = CARTESIAN_POINT ( 'NONE',  ( 3.215625000614518836, 3.027376345333611329, 5.243569643749999010 ) ) ;
#53910 = CARTESIAN_POINT ( 'NONE',  ( 18.60937500061451644, 0.000000000000000000, 5.243569643749999010 ) ) ;
#53911 = CARTESIAN_POINT ( 'NONE',  ( 29.74687500061451217, 6.054752690667223547, 3.707466751127219781E-16 ) ) ;
#53912 = CARTESIAN_POINT ( 'NONE',  ( 5.165625000614518569, -6.054752690667223547, -1.112240025338166033E-15 ) ) ;
#53913 = CARTESIAN_POINT ( 'NONE',  ( 19.26562500061451644, 3.027376345333613106, -5.243569643749998122 ) ) ;
#53914 = CARTESIAN_POINT ( 'NONE',  ( -2.121784821874996840, 12.22812500061451857, 33.67503911421598417 ) ) ;
#53915 = CARTESIAN_POINT ( 'NONE',  ( 15.45000000122903216, -2.886751345948125991, -5.000000000000000000 ) ) ;
#53916 = CARTESIAN_POINT ( 'NONE',  ( 11.59687500061451892, -2.746126346562641984, -4.756430356249999214 ) ) ;
#53917 = CARTESIAN_POINT ( 'NONE',  ( 5.990625000614517859, -3.027376345333614438, 5.243569643749998122 ) ) ;
#53918 = CARTESIAN_POINT ( 'NONE',  ( 26.09062500061451573, 6.054752690667223547, 3.707466751127219781E-16 ) ) ;
#53919 = CARTESIAN_POINT ( 'NONE',  ( 23.25937500061451857, -4.541064518000417216, -2.621784821875001281 ) ) ;
#53920 = CARTESIAN_POINT ( 'NONE',  ( 14.31562500061451537, 3.027376345333613106, -5.243569643749998122 ) ) ;
#53921 = CARTESIAN_POINT ( 'NONE',  ( 25.91250000122903074, 4.330127018922192761, -2.499999999999997780 ) ) ;
#53922 = CARTESIAN_POINT ( 'NONE',  ( 22.22812500061451502, -4.541064518000419881, 2.621784821874995952 ) ) ;
#53923 = CARTESIAN_POINT ( 'NONE',  ( 19.13437500061451857, -4.541064518000419881, 2.621784821874995952 ) ) ;
#53924 = CARTESIAN_POINT ( 'NONE',  ( 15.51562500061451644, -6.054752690667223547, -1.112240025338166033E-15 ) ) ;
#53925 = CARTESIAN_POINT ( 'NONE',  ( -4.243569643749997233, 14.94687500061451679, 32.45002607614398471 ) ) ;
#53926 = CARTESIAN_POINT ( 'NONE',  ( 20.61562500061451431, 3.027376345333613106, -5.243569643749998122 ) ) ;
#53927 = CARTESIAN_POINT ( 'NONE',  ( 29.05312500061451431, -4.541064518000417216, -2.621784821875001281 ) ) ;
#53928 = ORIENTED_EDGE ( 'NONE', *, *, #71265, .F. ) ;
#53929 = ORIENTED_EDGE ( 'NONE', *, *, #41327, .F. ) ;
#53930 = CARTESIAN_POINT ( 'NONE',  ( 22.91249999999999432, -5.773502691896255534, -1.060575238724906372E-15 ) ) ;
#53931 = CARTESIAN_POINT ( 'NONE',  ( -3.999999999999997335, 10.13750000000000284, -27.69059892324149175 ) ) ;
#53932 = CARTESIAN_POINT ( 'NONE',  ( 2.733878782416514941, -4.186395442746991158, 2.733878782416514941 ) ) ;
#53933 = CARTESIAN_POINT ( 'NONE',  ( 27.59062500061451573, -3.027376345333614438, 5.243569643749998122 ) ) ;
#53934 = CARTESIAN_POINT ( 'NONE',  ( 7.265625000614516438, 3.027376345333611329, 5.243569643749999010 ) ) ;
#53935 = CARTESIAN_POINT ( 'NONE',  ( 20.25000000122903288, -2.886751345948129988, 4.999999999999997335 ) ) ;
#53936 = CARTESIAN_POINT ( 'NONE',  ( 25.60312500061451502, 4.541064518000418104, -2.621784821874998173 ) ) ;
#53937 = CARTESIAN_POINT ( 'NONE',  ( 24.07499999999999929, 4.330127018922191873, 2.499999999999999556 ) ) ;
#53938 = CARTESIAN_POINT ( 'NONE',  ( 28.45312500061451289, 0.000000000000000000, 5.243569643749999010 ) ) ;
#53939 = CARTESIAN_POINT ( 'NONE',  ( 8.203125000614518214, 0.000000000000000000, 5.243569643749999010 ) ) ;
#53940 = ORIENTED_EDGE ( 'NONE', *, *, #44720, .F. ) ;
#53941 = EDGE_CURVE ( 'NONE', #41163, #49458, #21773, .T. ) ;
#53942 = CARTESIAN_POINT ( 'NONE',  ( 22.86562500061451431, 3.027376345333613106, -5.243569643749998122 ) ) ;
#53943 = CARTESIAN_POINT ( 'NONE',  ( 6.065625000614516260, -6.054752690667223547, -1.112240025338166033E-15 ) ) ;
#53944 = CARTESIAN_POINT ( 'NONE',  ( 14.85937500061451644, 4.119189519843966529, -2.378215178124998275 ) ) ;
#53945 = CARTESIAN_POINT ( 'NONE',  ( 4.153125000614515727, 0.000000000000000000, 5.243569643749999010 ) ) ;
#53946 = CARTESIAN_POINT ( 'NONE',  ( -3.999999999999999556, 14.67500000122903536, -32.30940107675850470 ) ) ;
#53947 = CARTESIAN_POINT ( 'NONE',  ( -5.810221930991193690E-16, 10.10000000122903430, 26.00000000000000355 ) ) ;
#53948 = VECTOR ( 'NONE', #9932, 1000.000000000000000 ) ;
#53949 = CARTESIAN_POINT ( 'NONE',  ( 10.23750000000000071, -2.886751345948129988, 4.999999999999997335 ) ) ;
#53950 = CARTESIAN_POINT ( 'NONE',  ( 10.32187500061451679, 3.027376345333613106, -5.243569643749998122 ) ) ;
#53951 = CARTESIAN_POINT ( 'NONE',  ( 8.925000001229033586, 2.886751345948126879, 4.999999999999999112 ) ) ;
#53952 = CARTESIAN_POINT ( 'NONE',  ( 14.89687500061451786, 6.054752690667223547, 3.707466751127219781E-16 ) ) ;
#53953 = CARTESIAN_POINT ( 'NONE',  ( 14.77500000000000036, -4.330127018922194537, 2.499999999999995559 ) ) ;
#53954 = CARTESIAN_POINT ( 'NONE',  ( 6.609375000614519102, -4.541064518000417216, -2.621784821875001281 ) ) ;
#53955 = CARTESIAN_POINT ( 'NONE',  ( -4.243569643749999898, 9.903125000614517504, -30.00000000000000000 ) ) ;
#53956 = CARTESIAN_POINT ( 'NONE',  ( 45.00000000000000000, 0.000000000000000000, 0.000000000000000000 ) ) ;
#53957 = CARTESIAN_POINT ( 'NONE',  ( 12.38437500061451857, -4.541064518000419881, 2.621784821874995952 ) ) ;
#53958 = LINE ( 'NONE', #60569, #20568 ) ;
#53959 = CARTESIAN_POINT ( 'NONE',  ( 21.85312500061451502, -4.541064518000417216, -2.621784821875001281 ) ) ;
#53960 = CARTESIAN_POINT ( 'NONE',  ( -2.121784821874996840, 10.93437500061451928, 33.67503911421598417 ) ) ;
#53961 = CARTESIAN_POINT ( 'NONE',  ( -4.243569643749999898, 18.90312500061459033, 30.00000000000000000 ) ) ;
#53962 = CARTESIAN_POINT ( 'NONE',  ( 25.99687500061451928, -3.027376345333610441, -5.243569643749999898 ) ) ;
#53963 = FACE_OUTER_BOUND ( 'NONE', #66225, .T. ) ;
#53964 = CARTESIAN_POINT ( 'NONE',  ( 5.615625000614517859, -6.054752690667223547, -1.112240025338166033E-15 ) ) ;
#53965 = CARTESIAN_POINT ( 'NONE',  ( 22.50937500061451502, 2.746126346562643317, 4.756430356249998326 ) ) ;
#53966 = CARTESIAN_POINT ( 'NONE',  ( 17.63437500061451502, 4.541064518000418104, 2.621784821874999949 ) ) ;
#53967 = CARTESIAN_POINT ( 'NONE',  ( 7.696875000614517681, 0.000000000000000000, 4.756430356249998326 ) ) ;
#53968 = CARTESIAN_POINT ( 'NONE',  ( 26.47500000122903074, 2.886751345948126879, 4.999999999999999112 ) ) ;
#53969 = CARTESIAN_POINT ( 'NONE',  ( 5.334375000614517859, 6.421520780324663323E-16, -5.243569643749999010 ) ) ;
#53970 = CARTESIAN_POINT ( 'NONE',  ( 16.17187500061451644, 3.027376345333613106, -5.243569643749998122 ) ) ;
#53971 = CARTESIAN_POINT ( 'NONE',  ( 4.829389079492484527, -1.295504259766551813, -5.081142917896463551 ) ) ;
#53972 = CARTESIAN_POINT ( 'NONE',  ( 24.37500000000000000, 6.123233995736764310E-16, -4.999999999999998224 ) ) ;
#53973 = CARTESIAN_POINT ( 'NONE',  ( 4.350000001229033408, 5.773502691896255534, 3.535250795749688894E-16 ) ) ;
#53974 = CARTESIAN_POINT ( 'NONE',  ( 26.22187500061451715, 3.027376345333611329, 5.243569643749999010 ) ) ;
#53975 = CARTESIAN_POINT ( 'NONE',  ( 3.756430356250000102, 14.55312499938548321, 30.00000000000000000 ) ) ;
#53976 = CARTESIAN_POINT ( 'NONE',  ( 5.587500001229033231, 6.123233995736764310E-16, -4.999999999999998224 ) ) ;
#53977 = CARTESIAN_POINT ( 'NONE',  ( 7.612500000000000711, -5.773502691896255534, -1.060575238724906372E-15 ) ) ;
#53978 = CARTESIAN_POINT ( 'NONE',  ( 9.496875000614517504, 0.000000000000000000, 4.756430356249998326 ) ) ;
#53979 = CARTESIAN_POINT ( 'NONE',  ( 22.56562500061451715, 3.027376345333611329, 5.243569643749999010 ) ) ;
#53980 = CARTESIAN_POINT ( 'NONE',  ( 10.68750000000000000, -2.886751345948129988, 4.999999999999997335 ) ) ;
#53981 = CARTESIAN_POINT ( 'NONE',  ( 3.928125000614516527, 6.421520780324663323E-16, -5.243569643749999010 ) ) ;
#53982 = CARTESIAN_POINT ( 'NONE',  ( 19.72499999999999787, -4.330127018922194537, 2.499999999999995559 ) ) ;
#53983 = EDGE_CURVE ( 'NONE', #9370, #63581, #39146, .T. ) ;
#53984 = CARTESIAN_POINT ( 'NONE',  ( 18.77812500061451573, 6.421520780324663323E-16, -5.243569643749999010 ) ) ;
#53985 = CARTESIAN_POINT ( 'NONE',  ( 4.738577610423850395, 3.409353767520035383, -4.094826053678926492 ) ) ;
#53986 = CARTESIAN_POINT ( 'NONE',  ( 23.25000000122903288, 5.773502691896255534, 3.535250795749688894E-16 ) ) ;
#53987 = CARTESIAN_POINT ( 'NONE',  ( 3.756430356250000546, 19.42812499938548143, 27.83122392262697886 ) ) ;
#53988 = CARTESIAN_POINT ( 'NONE',  ( 3.600000000000002309, -4.330127018922190985, -2.500000000000001332 ) ) ;
#53989 = EDGE_CURVE ( 'NONE', #60188, #4158, #46026, .T. ) ;
#53990 = ORIENTED_EDGE ( 'NONE', *, *, #68150, .T. ) ;
#53991 = CARTESIAN_POINT ( 'NONE',  ( 19.26562500061451644, 3.027376345333613106, -5.243569643749998122 ) ) ;
#53992 = CARTESIAN_POINT ( 'NONE',  ( 26.99062500061451431, 6.054752690667223547, 3.707466751127219781E-16 ) ) ;
#53993 = CARTESIAN_POINT ( 'NONE',  ( 23.89687500061451786, 6.054752690667223547, 3.707466751127219781E-16 ) ) ;
#53994 = CARTESIAN_POINT ( 'NONE',  ( 8.324999999999999289, 4.330127018922191873, 2.499999999999999556 ) ) ;
#53995 = CARTESIAN_POINT ( 'NONE',  ( 13.04062500061451502, 6.054752690667223547, 3.707466751127219781E-16 ) ) ;
#53996 = CARTESIAN_POINT ( 'NONE',  ( 27.47812500061451502, 4.541064518000418104, 2.621784821874999949 ) ) ;
#53997 = CARTESIAN_POINT ( 'NONE',  ( 18.12187500061451573, 3.027376345333611329, 5.243569643749999010 ) ) ;
#53998 = CARTESIAN_POINT ( 'NONE',  ( 8.840625000614515727, -3.027376345333610441, -5.243569643749999898 ) ) ;
#53999 = CARTESIAN_POINT ( 'NONE',  ( -5.810221930991193690E-16, 18.65000000122903501, 26.00000000000000355 ) ) ;
#54000 = CARTESIAN_POINT ( 'NONE',  ( -3.000416591977282496E-16, 11.19687500061451679, 25.09994784771203058 ) ) ;
#54001 = AXIS2_PLACEMENT_3D ( 'NONE', #53066, #70057, #43084 ) ;
#54002 = CARTESIAN_POINT ( 'NONE',  ( 24.41250000122903430, -4.330127018922190985, -2.500000000000001332 ) ) ;
#54003 = CARTESIAN_POINT ( 'NONE',  ( 19.17187500061451644, -5.492252693125287522, -1.008910452111647106E-15 ) ) ;
#54004 = CARTESIAN_POINT ( 'NONE',  ( 14.24062500061451608, -3.027376345333610441, -5.243569643749999898 ) ) ;
#54005 = CARTESIAN_POINT ( 'NONE',  ( 9.646875000614516082, -3.027376345333614438, 5.243569643749998122 ) ) ;
#54006 = CARTESIAN_POINT ( 'NONE',  ( 9.346875000614517148, -3.027376345333610441, -5.243569643749999898 ) ) ;
#54007 = EDGE_CURVE ( 'NONE', #20756, #61022, #29864, .T. ) ;
#54008 = VERTEX_POINT ( 'NONE', #13960 ) ;
#54009 = CARTESIAN_POINT ( 'NONE',  ( 65.00000000000000000, 8.874999999999998224, -1.494782592887675232 ) ) ;
#54010 = CARTESIAN_POINT ( 'NONE',  ( 21.32812500061451644, -4.541064518000419881, 2.621784821874995952 ) ) ;
#54011 = CARTESIAN_POINT ( 'NONE',  ( 16.99687500061451573, -3.027376345333610441, -5.243569643749999898 ) ) ;
#54012 = CARTESIAN_POINT ( 'NONE',  ( 22.82812500061451644, 6.421520780324663323E-16, -5.243569643749999010 ) ) ;
#54013 = CARTESIAN_POINT ( 'NONE',  ( -1.999999999999997113, 11.07500000000000107, 33.46410161513775705 ) ) ;
#54014 = CARTESIAN_POINT ( 'NONE',  ( 27.59062500061451573, -3.027376345333614438, 5.243569643749998122 ) ) ;
#54015 = CARTESIAN_POINT ( 'NONE',  ( 8.287500001229034297, 6.123233995736764310E-16, -4.999999999999998224 ) ) ;
#54016 = ORIENTED_EDGE ( 'NONE', *, *, #2783, .T. ) ;
#54017 = CARTESIAN_POINT ( 'NONE',  ( 2.775000001229033675, -5.773502691896255534, -1.060575238724906372E-15 ) ) ;
#54018 = CARTESIAN_POINT ( 'NONE',  ( 2.000000000000001332, 17.00000000000000000, -26.53589838486224650 ) ) ;
#54019 = CARTESIAN_POINT ( 'NONE',  ( 24.45000000122903572, -2.886751345948125991, -5.000000000000000000 ) ) ;
#54020 = CARTESIAN_POINT ( 'NONE',  ( 1.878215178125000495, 14.17812499938548321, 26.74683588394047007 ) ) ;
#54021 = EDGE_CURVE ( 'NONE', #26767, #27538, #3522, .T. ) ;
#54022 = CARTESIAN_POINT ( 'NONE',  ( 5.934375000614517504, 4.541064518000418104, 2.621784821874999949 ) ) ;
#54023 = CARTESIAN_POINT ( 'NONE',  ( 23.47499999999999787, 6.123233995736764310E-16, -4.999999999999998224 ) ) ;
#54024 = CARTESIAN_POINT ( 'NONE',  ( 15.32812500061451644, 4.541064518000418104, 2.621784821874999949 ) ) ;
#54025 = CARTESIAN_POINT ( 'NONE',  ( 7.809375000614519280, 0.000000000000000000, 5.243569643749999010 ) ) ;
#54026 = CARTESIAN_POINT ( 'NONE',  ( 25.91250000122903074, 4.330127018922192761, -2.499999999999997780 ) ) ;
#54027 = CARTESIAN_POINT ( 'NONE',  ( 17.63437500061451502, 4.541064518000418104, 2.621784821874999949 ) ) ;
#54028 = CARTESIAN_POINT ( 'NONE',  ( 5.559375000614517504, 0.000000000000000000, 5.243569643749999010 ) ) ;
#54029 = CYLINDRICAL_SURFACE ( 'NONE', #22676, 4.999999999999998224 ) ;
#54030 = CARTESIAN_POINT ( 'NONE',  ( 4.490625000614516971, 6.054752690667223547, 3.707466751127219781E-16 ) ) ;
#54031 = CARTESIAN_POINT ( 'NONE',  ( 15.81562500061451537, 3.027376345333611329, 5.243569643749999010 ) ) ;
#54032 = ORIENTED_EDGE ( 'NONE', *, *, #47475, .F. ) ;
#54033 = CARTESIAN_POINT ( 'NONE',  ( 12.40312500061451573, -4.541064518000417216, -2.621784821875001281 ) ) ;
#54034 = CARTESIAN_POINT ( 'NONE',  ( 4.612500001229032698, -4.330127018922190985, -2.500000000000001332 ) ) ;
#54035 = CARTESIAN_POINT ( 'NONE',  ( 9.890625000614516438, 6.054752690667223547, 3.707466751127219781E-16 ) ) ;
#54036 = CARTESIAN_POINT ( 'NONE',  ( 20.10937500061451289, -4.119189519843965641, -2.378215178125001383 ) ) ;
#54037 = CARTESIAN_POINT ( 'NONE',  ( 10.46249999999999858, 2.886751345948129099, -4.999999999999998224 ) ) ;
#54038 = CARTESIAN_POINT ( 'NONE',  ( 3.637500001229036162, -4.330127018922194537, 2.499999999999995559 ) ) ;
#54039 = CARTESIAN_POINT ( 'NONE',  ( 18.00000000000000355, -4.330127018922190985, -2.500000000000001332 ) ) ;
#54040 = CARTESIAN_POINT ( 'NONE',  ( 17.93437500061451928, 6.421520780324663323E-16, -5.243569643749999010 ) ) ;
#54041 = CARTESIAN_POINT ( 'NONE',  ( 15.45000000122903216, -2.886751345948125991, -5.000000000000000000 ) ) ;
#54042 = CARTESIAN_POINT ( 'NONE',  ( 22.53750000000000142, -2.886751345948125991, -5.000000000000000000 ) ) ;
#54043 = CARTESIAN_POINT ( 'NONE',  ( -4.243569643749997233, 15.34062500061451750, -27.54997392385601174 ) ) ;
#54044 = CARTESIAN_POINT ( 'NONE',  ( 9.299999999999998934, 0.000000000000000000, 4.999999999999998224 ) ) ;
#54045 = CARTESIAN_POINT ( 'NONE',  ( -1.071796769724487453, 18.55759618943233491, 26.00000000000000000 ) ) ;
#54046 = CARTESIAN_POINT ( 'NONE',  ( 29.27812500061451573, 4.541064518000418104, 2.621784821874999949 ) ) ;
#54047 = AXIS2_PLACEMENT_3D ( 'NONE', #19670, #69930, #58101 ) ;
#54048 = CARTESIAN_POINT ( 'NONE',  ( -6.275039685470489619E-15, 18.31250000000000000, 33.99999999999999289 ) ) ;
#54049 = DIRECTION ( 'NONE',  ( 0.000000000000000000, 0.000000000000000000, 1.000000000000000000 ) ) ;
#54050 = CARTESIAN_POINT ( 'NONE',  ( 16.99687500061451573, -3.027376345333610441, -5.243569643749999898 ) ) ;
#54051 =( BOUNDED_CURVE ( )  B_SPLINE_CURVE ( 2, ( #4726, #59757, #43520, #37234, #31330, #49425, #26900 ),
 .UNSPECIFIED., .F., .F. ) 
 B_SPLINE_CURVE_WITH_KNOTS ( ( 3, 2, 2, 3 ),
 ( 0.3250000000000000111, 0.3277777777777777790, 0.3305555555555556024, 0.3333333333333333703 ),
 .UNSPECIFIED. ) 
 CURVE ( )  GEOMETRIC_REPRESENTATION_ITEM ( )  RATIONAL_B_SPLINE_CURVE ( ( 1.000000000000000000, 0.8660254037844387076, 1.000000000000000000, 0.8660254037844387076, 1.000000000000000000, 0.8660254037844360431, 1.000000000000002665 ) ) 
 REPRESENTATION_ITEM ( '' )  );
#54052 = CARTESIAN_POINT ( 'NONE',  ( 28.68749999999999645, -2.886751345948129988, 4.999999999999997335 ) ) ;
#54053 = CARTESIAN_POINT ( 'NONE',  ( 12.25312500061451537, 0.000000000000000000, 5.243569643749999010 ) ) ;
#54054 = CARTESIAN_POINT ( 'NONE',  ( 7.893750001229032698, 5.773502691896255534, 3.535250795749688894E-16 ) ) ;
#54055 = CARTESIAN_POINT ( 'NONE',  ( 23.59687500061451715, -3.027376345333614438, 5.243569643749998122 ) ) ;
#54056 = CARTESIAN_POINT ( 'NONE',  ( 16.88437500061451502, -2.746126346562641984, -4.756430356249999214 ) ) ;
#54057 = CARTESIAN_POINT ( 'NONE',  ( 7.340625000614518392, -3.027376345333614438, 5.243569643749998122 ) ) ;
#54058 = CARTESIAN_POINT ( 'NONE',  ( 12.87187500061451750, -6.054752690667223547, -1.112240025338166033E-15 ) ) ;
#54059 = VERTEX_POINT ( 'NONE', #58287 ) ;
#54060 = CARTESIAN_POINT ( 'NONE',  ( 24.72187500061451360, 3.027376345333613106, -5.243569643749998122 ) ) ;
#54061 = CARTESIAN_POINT ( 'NONE',  ( 28.04062500061451502, -3.027376345333614438, 5.243569643749998122 ) ) ;
#54062 = CARTESIAN_POINT ( 'NONE',  ( 8.587500000000002132, -2.886751345948125991, -5.000000000000000000 ) ) ;
#54063 = CARTESIAN_POINT ( 'NONE',  ( 17.40000000122903145, 5.773502691896255534, 3.535250795749688894E-16 ) ) ;
#54064 = CARTESIAN_POINT ( 'NONE',  ( 27.30000000122903359, 5.773502691896255534, 3.535250795749688401E-16 ) ) ;
#54065 = CARTESIAN_POINT ( 'NONE',  ( 8.596875000614515372, 0.000000000000000000, 4.756430356249998326 ) ) ;
#54066 = EDGE_LOOP ( 'NONE', ( #46477, #22922, #49609, #38241 ) ) ;
#54067 = CARTESIAN_POINT ( 'NONE',  ( 14.96250000000000036, 2.886751345948129099, -4.999999999999998224 ) ) ;
#54068 = CARTESIAN_POINT ( 'NONE',  ( 18.75000000000000000, 0.000000000000000000, 4.999999999999998224 ) ) ;
#54069 = CARTESIAN_POINT ( 'NONE',  ( 13.60312500061451679, 0.000000000000000000, 5.243569643749999010 ) ) ;
#54070 = VERTEX_POINT ( 'NONE', #6975 ) ;
#54071 = CARTESIAN_POINT ( 'NONE',  ( -1.071796769724492115, 16.81115380933863435, 34.00000000000000000 ) ) ;
#54072 = CARTESIAN_POINT ( 'NONE',  ( 9.001249775931846008E-16, 18.17187500061451999, -25.09994784771203058 ) ) ;
#54073 = CARTESIAN_POINT ( 'NONE',  ( 3.890625000614517326, -3.027376345333610441, -5.243569643749999898 ) ) ;
#54074 = CARTESIAN_POINT ( 'NONE',  ( -3.756430356250000990, 13.35312499938548392, 32.16877607737301048 ) ) ;
#54075 = CARTESIAN_POINT ( 'NONE',  ( 10.08749999999999858, 5.773502691896255534, 3.535250795749688894E-16 ) ) ;
#54076 = CARTESIAN_POINT ( 'NONE',  ( 27.57187500061451502, -4.119189519843968306, 2.378215178124996054 ) ) ;
#54077 = EDGE_LOOP ( 'NONE', ( #65501, #70890, #39860, #32254 ) ) ;
#54078 = CARTESIAN_POINT ( 'NONE',  ( -3.000416591977282496E-16, 15.19062500061451715, 25.09994784771203058 ) ) ;
#54079 = CARTESIAN_POINT ( 'NONE',  ( 26.16562500061451502, 3.027376345333611329, 5.243569643749999010 ) ) ;
#54080 = CARTESIAN_POINT ( 'NONE',  ( 25.70625000122903003, -4.330127018922190985, -2.500000000000001332 ) ) ;
#54081 = CARTESIAN_POINT ( 'NONE',  ( 3.756430356250000102, 20.29062499938548569, 30.00000000000000000 ) ) ;
#54082 = CARTESIAN_POINT ( 'NONE',  ( 24.30937500061451573, 4.541064518000418104, -2.621784821874998173 ) ) ;
#54083 = CARTESIAN_POINT ( 'NONE',  ( 18.25312500061451715, -4.541064518000417216, -2.621784821875001281 ) ) ;
#54084 = CARTESIAN_POINT ( 'NONE',  ( -4.243569643749999898, 13.05312500061459424, -30.00000000000000000 ) ) ;
#54085 = CARTESIAN_POINT ( 'NONE',  ( 24.22500000122903430, 2.886751345948126879, 4.999999999999999112 ) ) ;
#54086 = CARTESIAN_POINT ( 'NONE',  ( 3.853125000614517681, -4.541064518000417216, -2.621784821875001281 ) ) ;
#54087 = CARTESIAN_POINT ( 'NONE',  ( 27.30937500061451573, -4.119189519843965641, -2.378215178125001383 ) ) ;
#54088 = CARTESIAN_POINT ( 'NONE',  ( 21.77812500061451928, -4.541064518000419881, 2.621784821874995952 ) ) ;
#54089 = CARTESIAN_POINT ( 'NONE',  ( 9.271875000614516082, -5.492252693125287522, -1.008910452111647106E-15 ) ) ;
#54090 = CARTESIAN_POINT ( 'NONE',  ( 1.878215178124997609, 16.61562499938548143, 33.25316411605952993 ) ) ;
#54092 = ADVANCED_FACE ( 'NONE', ( #23592 ), #30595, .T. ) ;
#54091 = CARTESIAN_POINT ( 'NONE',  ( 16.50937500061451502, -4.541064518000417216, -2.621784821875001281 ) ) ;
#54093 = CARTESIAN_POINT ( 'NONE',  ( 17.55937500061451573, 4.541064518000418104, -2.621784821874998173 ) ) ;
#54094 = CARTESIAN_POINT ( 'NONE',  ( 25.65937500061451715, 4.541064518000418104, -2.621784821874998173 ) ) ;
#54095 = CARTESIAN_POINT ( 'NONE',  ( -2.121784821874996840, 13.63437500061451857, 33.67503911421598417 ) ) ;
#54096 = CARTESIAN_POINT ( 'NONE',  ( 5.278125000614516615, 6.421520780324663323E-16, -5.243569643749999010 ) ) ;
#54097 = CARTESIAN_POINT ( 'NONE',  ( 28.00312500061451715, 0.000000000000000000, 5.243569643749999010 ) ) ;
#54098 = CARTESIAN_POINT ( 'NONE',  ( 28.30312500061451431, 4.541064518000418104, -2.621784821874998173 ) ) ;
#54099 = CARTESIAN_POINT ( 'NONE',  ( 3.999999999999998668, 16.32500000122903216, -32.30940107675850470 ) ) ;
#54100 = CARTESIAN_POINT ( 'NONE',  ( 6.834375000614518747, 4.541064518000418104, 2.621784821874999949 ) ) ;
#54101 = CARTESIAN_POINT ( 'NONE',  ( 13.23750000122903359, 6.123233995736764310E-16, -4.999999999999998224 ) ) ;
#54102 = CARTESIAN_POINT ( 'NONE',  ( 8.812500001229034652, 4.330127018922192761, -2.499999999999997780 ) ) ;
#54103 = CARTESIAN_POINT ( 'NONE',  ( 3.890625000614517326, -3.027376345333610441, -5.243569643749999898 ) ) ;
#54104 = CARTESIAN_POINT ( 'NONE',  ( -4.000000000000000000, 17.16874999877096641, 30.00000000000000000 ) ) ;
#54105 = CARTESIAN_POINT ( 'NONE',  ( 19.85625000122902861, -4.330127018922190985, -2.500000000000001332 ) ) ;
#54106 = CARTESIAN_POINT ( 'NONE',  ( 13.39687500061451608, -3.027376345333610441, -5.243569643749999898 ) ) ;
#54107 = CARTESIAN_POINT ( 'NONE',  ( 23.69999999999999929, 0.000000000000000000, 4.999999999999998224 ) ) ;
#54108 = ORIENTED_EDGE ( 'NONE', *, *, #29492, .T. ) ;
#54109 = CARTESIAN_POINT ( 'NONE',  ( 22.86562500061451431, 3.027376345333613106, -5.243569643749998122 ) ) ;
#54110 = CARTESIAN_POINT ( 'NONE',  ( 7.528125000614515727, 6.421520780324663323E-16, -5.243569643749999010 ) ) ;
#54111 = CARTESIAN_POINT ( 'NONE',  ( 24.34687500061451715, 6.054752690667223547, 3.707466751127219781E-16 ) ) ;
#54112 = CARTESIAN_POINT ( 'NONE',  ( 7.978125000614517681, 6.421520780324663323E-16, -5.243569643749999010 ) ) ;
#54113 = CARTESIAN_POINT ( 'NONE',  ( 20.51249999999999929, 2.886751345948161074, 4.999999999999941380 ) ) ;
#54114 = CARTESIAN_POINT ( 'NONE',  ( 8.062500001229034652, 0.000000000000000000, 4.999999999999998224 ) ) ;
#54115 = CARTESIAN_POINT ( 'NONE',  ( 21.66562500061451502, 3.027376345333611329, 5.243569643749999010 ) ) ;
#54116 = ADVANCED_BREP_SHAPE_REPRESENTATION ( '', ( #21999, #23765 ), #19014 ) ;
#54117 = CARTESIAN_POINT ( 'NONE',  ( -3.000416591977282496E-16, 10.24062500061451608, -34.90005215228797653 ) ) ;
#54118 = CARTESIAN_POINT ( 'NONE',  ( 11.10000000122903252, 5.773502691896255534, 3.535250795749688894E-16 ) ) ;
#54119 = CARTESIAN_POINT ( 'NONE',  ( 19.79062500061451502, 6.054752690667223547, 3.707466751127219781E-16 ) ) ;
#54120 = CARTESIAN_POINT ( 'NONE',  ( 17.65312500061451573, 0.000000000000000000, 5.243569643749999010 ) ) ;
#54121 = CARTESIAN_POINT ( 'NONE',  ( 27.23437500061451644, -4.119189519843968306, 2.378215178124996054 ) ) ;
#54122 = CARTESIAN_POINT ( 'NONE',  ( 17.28750000000000142, 5.773502691896255534, 3.535250795749688894E-16 ) ) ;
#54123 = CARTESIAN_POINT ( 'NONE',  ( 11.62500000122903465, 2.886751345948126879, 4.999999999999999112 ) ) ;
#54124 = EDGE_CURVE ( 'NONE', #8958, #57550, #23950, .T. ) ;
#54125 = CARTESIAN_POINT ( 'NONE',  ( 7.790625000614518569, -3.027376345333614438, 5.243569643749998122 ) ) ;
#54126 = CARTESIAN_POINT ( 'NONE',  ( 13.79062500061451502, -3.027376345333610441, -5.243569643749999898 ) ) ;
#54127 = CARTESIAN_POINT ( 'NONE',  ( 22.35000000122903074, 5.773502691896255534, 3.535250795749688894E-16 ) ) ;
#54128 = CARTESIAN_POINT ( 'NONE',  ( 20.74687500061451573, 6.054752690667223547, 3.707466751127219781E-16 ) ) ;
#54129 = CARTESIAN_POINT ( 'NONE',  ( 9.637500001229033941, 6.123233995736764310E-16, -4.999999999999998224 ) ) ;
#54130 = EDGE_CURVE ( 'NONE', #65074, #44184, #45309, .T. ) ;
#54131 = CARTESIAN_POINT ( 'NONE',  ( 5.887500001229034829, -4.330127018922194537, 2.499999999999995559 ) ) ;
#54132 = CARTESIAN_POINT ( 'NONE',  ( 7.246875000614518392, 6.054752690667223547, 3.707466751127219781E-16 ) ) ;
#54133 = CARTESIAN_POINT ( 'NONE',  ( 22.92187500061451644, 3.027376345333613106, -5.243569643749998122 ) ) ;
#54134 = CARTESIAN_POINT ( 'NONE',  ( 4.564313923822768793, 2.041911324548167261, -4.640016024762649849 ) ) ;
#54135 = CARTESIAN_POINT ( 'NONE',  ( 19.97812500061451502, -4.541064518000419881, 2.621784821874995952 ) ) ;
#54136 = CARTESIAN_POINT ( 'NONE',  ( 23.44687500061451502, 6.054752690667223547, 3.707466751127219781E-16 ) ) ;
#54137 = CARTESIAN_POINT ( 'NONE',  ( -1.878215178124999163, 19.20312499938548356, 26.74683588394047007 ) ) ;
#54138 = CARTESIAN_POINT ( 'NONE',  ( 12.56250000122903465, 0.000000000000000000, 4.999999999999998224 ) ) ;
#54139 = CARTESIAN_POINT ( 'NONE',  ( 1.626862140677534273E-15, 13.47500000122903252, -26.00000000000000355 ) ) ;
#54140 = CARTESIAN_POINT ( 'NONE',  ( 4.809375000614516615, -4.541064518000417216, -2.621784821875001281 ) ) ;
#54141 = CARTESIAN_POINT ( 'NONE',  ( 17.12812500061451715, 4.541064518000418104, 2.621784821874999949 ) ) ;
#54142 = CARTESIAN_POINT ( 'NONE',  ( 12.75937500061451857, 0.000000000000000000, 5.243569643749999010 ) ) ;
#54143 = EDGE_LOOP ( 'NONE', ( #31299, #11129, #72606, #22351 ) ) ;
#54144 = CARTESIAN_POINT ( 'NONE',  ( 1.071796769724484344, 16.98259618943233562, -25.99999999999999645 ) ) ;
#54145 = CARTESIAN_POINT ( 'NONE',  ( 25.79062500061451502, -3.027376345333614438, 5.243569643749998122 ) ) ;
#54146 = CARTESIAN_POINT ( 'NONE',  ( 1.626862140677534273E-15, 10.77500000122903323, -26.00000000000000355 ) ) ;
#54147 = CARTESIAN_POINT ( 'NONE',  ( -3.999999999999999112, 11.52500000122903501, -32.30940107675850470 ) ) ;
#54148 = CARTESIAN_POINT ( 'NONE',  ( 14.47499999999999964, 6.123233995736764310E-16, -4.999999999999998224 ) ) ;
#54149 = CARTESIAN_POINT ( 'NONE',  ( 24.63750000122903216, 4.330127018922191873, 2.499999999999999556 ) ) ;
#54150 = CARTESIAN_POINT ( 'NONE',  ( 17.46562500061451217, 3.027376345333613106, -5.243569643749998122 ) ) ;
#54151 = VERTEX_POINT ( 'NONE', #54957 ) ;
#54152 = CARTESIAN_POINT ( 'NONE',  ( 23.21250000000000213, 2.886751345948126879, 4.999999999999999112 ) ) ;
#54153 = CARTESIAN_POINT ( 'NONE',  ( 22.84687500061451715, -3.027376345333610441, -5.243569643749999898 ) ) ;
#54154 = ORIENTED_EDGE ( 'NONE', *, *, #44687, .T. ) ;
#54155 = CARTESIAN_POINT ( 'NONE',  ( 10.30312500061451431, 4.541064518000418104, -2.621784821874998173 ) ) ;
#54156 = CARTESIAN_POINT ( 'NONE',  ( 3.253125000614518036, 0.000000000000000000, 5.243569643749999010 ) ) ;
#54157 = CARTESIAN_POINT ( 'NONE',  ( 16.47187500061451715, 5.824947211148865298E-16, -4.756430356249998326 ) ) ;
#54158 = CARTESIAN_POINT ( 'NONE',  ( 27.47812500061451502, 4.541064518000418104, 2.621784821874999949 ) ) ;
#54159 = CARTESIAN_POINT ( 'NONE',  ( 19.57500000000000284, 4.330127018922191873, 2.499999999999999556 ) ) ;
#54160 = CARTESIAN_POINT ( 'NONE',  ( 26.84999999999999787, 0.000000000000000000, 4.999999999999998224 ) ) ;
#54161 = CARTESIAN_POINT ( 'NONE',  ( 3.159375000614518036, 4.541064518000418104, -2.621784821874998173 ) ) ;
#54162 = CARTESIAN_POINT ( 'NONE',  ( 8.071875000614518569, 3.027376345333613106, -5.243569643749998122 ) ) ;
#54163 = CARTESIAN_POINT ( 'NONE',  ( 17.07187500061451502, 3.027376345333613106, -5.243569643749998122 ) ) ;
#54164 = EDGE_LOOP ( 'NONE', ( #19320, #19410, #52321, #64324 ) ) ;
#54165 = CARTESIAN_POINT ( 'NONE',  ( 27.10312500061451502, 0.000000000000000000, 5.243569643749999010 ) ) ;
#54166 = CARTESIAN_POINT ( 'NONE',  ( 28.50937500061451502, 0.000000000000000000, 5.243569643749999010 ) ) ;
#54167 = DIRECTION ( 'NONE',  ( -0.000000000000000000, -1.000000000000000000, -0.000000000000000000 ) ) ;
#54168 = CARTESIAN_POINT ( 'NONE',  ( 16.98750000000000426, -2.886751345948129988, 4.999999999999997335 ) ) ;
#54169 = CARTESIAN_POINT ( 'NONE',  ( 11.95312500061451644, -4.541064518000417216, -2.621784821875001281 ) ) ;
#54170 = CARTESIAN_POINT ( 'NONE',  ( 16.46249999999999858, 2.886751345948126879, 4.999999999999998224 ) ) ;
#54171 = CARTESIAN_POINT ( 'NONE',  ( 14.24999999999999822, 0.000000000000000000, 4.999999999999998224 ) ) ;
#54172 = CARTESIAN_POINT ( 'NONE',  ( 29.12812500061451715, 6.421520780324663323E-16, -5.243569643749999010 ) ) ;
#54173 = CARTESIAN_POINT ( 'NONE',  ( 17.21250000122903145, -4.330127018922190985, -2.500000000000001332 ) ) ;
#54174 = CARTESIAN_POINT ( 'NONE',  ( 8.400000000000000355, 0.000000000000000000, 4.999999999999998224 ) ) ;
#54175 = CARTESIAN_POINT ( 'NONE',  ( 16.88437500061451502, -4.119189519843968306, 2.378215178124996054 ) ) ;
#54176 = CARTESIAN_POINT ( 'NONE',  ( 5.090625000614516615, -3.027376345333614438, 5.243569643749998122 ) ) ;
#54177 = CARTESIAN_POINT ( 'NONE',  ( 22.73437500061451644, -4.541064518000419881, 2.621784821874995952 ) ) ;
#54178 = CARTESIAN_POINT ( 'NONE',  ( 2.121784821875001281, 17.30937500061451573, 33.67503911421598417 ) ) ;
#54179 = EDGE_CURVE ( 'NONE', #14728, #40395, #50767, .T. ) ;
#54180 = CARTESIAN_POINT ( 'NONE',  ( 25.17187500061451644, 3.027376345333613106, -5.243569643749998122 ) ) ;
#54181 = CARTESIAN_POINT ( 'NONE',  ( 4.875000000000000888, -4.330127018922194537, 2.499999999999995559 ) ) ;
#54182 = CARTESIAN_POINT ( 'NONE',  ( -2.000000000000000000, 11.03750000122903430, 26.53589838486224650 ) ) ;
#54183 = CARTESIAN_POINT ( 'NONE',  ( 12.51562500061451821, 3.027376345333613106, -5.243569643749998122 ) ) ;
#54184 = CARTESIAN_POINT ( 'NONE',  ( 4.462500001229035007, 0.000000000000000000, 4.999999999999998224 ) ) ;
#54185 = CARTESIAN_POINT ( 'NONE',  ( 9.384375000614518569, 6.421520780324663323E-16, -5.243569643749999010 ) ) ;
#54186 = CARTESIAN_POINT ( 'NONE',  ( 45.00000000000000000, 0.000000000000000000, 0.000000000000000000 ) ) ;
#54187 = CARTESIAN_POINT ( 'NONE',  ( 10.11562500061451608, -6.054752690667223547, -1.112240025338166033E-15 ) ) ;
#54188 = CARTESIAN_POINT ( 'NONE',  ( 14.29687500061451821, -3.027376345333610441, -5.243569643749999898 ) ) ;
#54189 =( LENGTH_UNIT ( ) NAMED_UNIT ( * ) SI_UNIT ( .MILLI., .METRE. ) );
#54190 = CARTESIAN_POINT ( 'NONE',  ( 22.27500000122903145, 2.886751345948129099, -4.999999999999998224 ) ) ;
#54191 = CARTESIAN_POINT ( 'NONE',  ( 11.44687500061451857, -3.027376345333614438, 5.243569643749998122 ) ) ;
#54192 = CARTESIAN_POINT ( 'NONE',  ( 12.70312500061451821, 0.000000000000000000, 5.243569643749999010 ) ) ;
#54193 = CARTESIAN_POINT ( 'NONE',  ( 29.30625000122903145, -4.330127018922190985, -2.500000000000001332 ) ) ;
#54194 = CARTESIAN_POINT ( 'NONE',  ( 22.43437500061451573, 6.421520780324663323E-16, -5.243569643749999010 ) ) ;
#54195 = CARTESIAN_POINT ( 'NONE',  ( 14.06249999999999645, 2.886751345948062486, -5.000000000000113687 ) ) ;
#54196 = CARTESIAN_POINT ( 'NONE',  ( -2.674018119152297590, 4.230323444454995752, 32.98541807432768280 ) ) ;
#54197 = CARTESIAN_POINT ( 'NONE',  ( 0.000000000000000000, 20.00000000000000000, -30.00000000000000000 ) ) ;
#54198 = CARTESIAN_POINT ( 'NONE',  ( 9.001249775931846008E-16, 15.02187500061451608, -25.09994784771203058 ) ) ;
#54199 = CARTESIAN_POINT ( 'NONE',  ( 15.97500000122903430, 2.886751345948129099, -4.999999999999998224 ) ) ;
#54200 = CARTESIAN_POINT ( 'NONE',  ( 10.77187500061451786, 3.027376345333613106, -5.243569643749998122 ) ) ;
#54201 = CARTESIAN_POINT ( 'NONE',  ( 9.001249775931846008E-16, 16.76562500061451999, -25.09994784771203058 ) ) ;
#54202 = CARTESIAN_POINT ( 'NONE',  ( 18.11250000122903359, -4.330127018922190985, -2.500000000000001332 ) ) ;
#54203 = CARTESIAN_POINT ( 'NONE',  ( 12.10312500061451857, 4.541064518000418104, -2.621784821874998173 ) ) ;
#54204 = VERTEX_POINT ( 'NONE', #15780 ) ;
#54205 = CARTESIAN_POINT ( 'NONE',  ( 15.82499999999999929, 6.123233995736764310E-16, -4.999999999999998224 ) ) ;
#54206 = FACE_OUTER_BOUND ( 'NONE', #69950, .T. ) ;
#54207 = CARTESIAN_POINT ( 'NONE',  ( 9.646875000614519635, -3.027376345333614438, 5.243569643749998122 ) ) ;
#54208 = DIRECTION ( 'NONE',  ( -1.000000000000000000, -0.000000000000000000, -0.000000000000000000 ) ) ;
#54209 = CARTESIAN_POINT ( 'NONE',  ( 12.63750000122903394, -4.330127018922194537, 2.499999999999995559 ) ) ;
#54210 = CARTESIAN_POINT ( 'NONE',  ( 20.25000000122903288, -2.886751345948129988, 4.999999999999997335 ) ) ;
#54211 = CARTESIAN_POINT ( 'NONE',  ( 18.29062500061451502, -3.027376345333610441, -5.243569643749999898 ) ) ;
#54212 =( BOUNDED_SURFACE ( )  B_SPLINE_SURFACE ( 1, 2, ( 
 ( #16085, #5015, #56349, #20893, #27549, #72974, #22356, #67445, #16442, #21257, #16807, #5739, #43447, #44181, #15713, #65969, #26820, #37890, #60409, #38251, #9818, #71884, #43810, #44552, #55259, #4655, #49718, #46347, #62958, #68521, #13073, #35612, #29710, #56697, #50804, #17882, #51888, #6097, #569, #12353, #68881, #34160, #34888, #57772, #45985, #67797, #28628, #7182, #28273, #18609, #63327, #57053, #207, #17171, #11645, #6821, #58132, #39731, #51166, #40090, #40442, #57417, #63683, #22712, #29355, #35251, #52248, #1651, #18238, #23075, #24159, #45265, #40811, #51531, #68165, #62248, #45632, #41174, #17528, #62604, #12000, #34523, #6459, #1286, #28994, #46712, #23796, #12715, #69247, #931, #23439, #65515, #9006, #35975, #30071, #70327, #31163, #58495, #52971, #64779, #48164, #13426, #14170, #37070, #25249, #47071, #7904, #59593, #7538, #71060, #3474, #64046, #14535, #69606, #41886, #70689, #24885, #25627, #31538, #2016, #20064, #53705, #36704, #54078, #65144, #64414, #59226, #69961, #58861, #8634, #30442, #42984, #3098, #2367, #19332, #47430, #13807, #8271, #19703, #42620, #47797, #25994, #41527, #48533, #36346, #14902, #30801, #20435, #53334, #2732, #37443, #42256, #52610, #24527, #18967, #3839, #383, #11825, #22890, #28450, #62069, #39913, #50627, #56168, #56523, #37803, #45086, #5563, #50985, #45448, #20806, #71429, #67621, #50273, #43361, #67981, #26360, #11096, #32267, #39181, #32, #5916, #28099, #11463, #65884, #62427, #54800, #68346, #15265, #17356, #61697, #33624, #34343, #4206, #56876, #17707, #6280, #48900, #28809, #51348, #751, #23260, #33985, #45810, #22538, #16987, #59963, #60323, #39545, #9371, #31903, #54440, #9733, #26734, #72797, #22180, #44734, #67268, #16627, #63515, #2198, #69074, #40267, #29180, #23623, #18794, #47616, #51713, #46170, #52073, #7367, #52436, #2555, #62788, #29898, #47256, #69790, #19156, #58319, #12544, #41710, #25073, #7730, #12902, #7008, #70147, #68709, #53157, #1116, #29538, #18069, #40630, #63149, #41358, #57604, #13625, #24350, #30264, #1843, #46898, #12181, #34708, #64234, #35078, #57238, #69437, #63868, #1479, #23985 ),
 ( #36168, #6651, #30625, #58686, #46532, #8096, #18433, #41000, #52797, #35435, #24713, #57959, #13258, #35796, #43184, #26183, #43548, #4029, #3294, #3660, #8824, #70884, #48723, #19896, #54993, #71246, #64971, #31361, #36897, #13992, #9559, #42810, #20625, #65703, #25822, #42449, #60149, #30991, #26554, #54266, #9193, #65333, #14362, #4399, #15090, #26928, #32458, #31728, #14722, #49453, #37993, #47992, #37626, #2918, #32092, #48359, #20258, #54623, #25449, #19525, #49094, #71623, #42084, #70521, #64606, #37265, #53902, #20996, #66070, #15448, #59787, #59051, #60514, #36531, #8456, #9920, #53524, #59417, #71987, #16905, #16188, #56446, #62347, #10292, #5480, #32822, #33183, #16546, #33538, #27287, #55722, #21726, #6198, #50904, #34260, #28726, #303, #33902, #27650, #11743, #72345, #56088, #21361, #56793, #15817, #39098, #72714, #43915, #38739, #38360, #50187, #66441, #60887, #55360, #4754, #61259, #66815, #61981, #67542, #49821, #22813, #10653, #44285, #28019, #39832, #5116, #73075, #22097, #44655, #67185, #61615, #11017, #39460, #50547, #22456, #45005, #11383, #5836, #28368, #45364, #67899, #17271, #7644, #68266, #46817, #29817, #17628, #8013, #46090, #51633, #7288, #36086, #57155, #63433, #6566, #40547, #69709, #69355, #12820, #18346, #58606, #51267, #52713, #29098, #669, #40921, #1755, #1034, #23540, #35354, #18712, #68626, #57878, #30182, #68989, #40188, #17988, #2119, #23177, #41632, #47176, #34624, #58239, #62709, #12466, #41277, #63063, #63788, #24631, #45731, #13178, #24268, #52352, #19075, #35717, #34996, #64151, #57525, #29456, #13538, #6926, #12103, #51993, #1394, #23903, #46451, #2836, #8740, #20174, #48639, #48275, #31649, #64521, #9480, #25365, #37913, #13914, #37546, #31273, #3209, #20537, #47909, #3946, #60430, #15009, #47538, #43093, #54544, #65621, #71164, #54182, #32009, #42728, #25738, #26101, #8375, #14638, #70799, #60068, #26469, #36453, #42001, #37179, #19813, #58967, #49008, #70067, #53816, #71539, #59329, #30548, #19440, #30904, #9111, #53075, #53446, #70438, #42366, #65249, #59704, #65990, #2470, #3578, #20914, #43466, #15371, #24994, #64888, #14276 ) ),
 .UNSPECIFIED., .F., .F., .F. ) 
 B_SPLINE_SURFACE_WITH_KNOTS ( ( 2, 2 ),
 ( 3, 2, 2, 2, 2, 2, 2, 2, 2, 2, 2, 2, 2, 2, 2, 2, 2, 2, 2, 2, 2, 2, 2, 2, 2, 2, 2, 2, 2, 2, 2, 2, 2, 2, 2, 2, 2, 2, 2, 2, 2, 2, 2, 2, 2, 2, 2, 2, 2, 2, 2, 2, 2, 2, 2, 2, 2, 2, 2, 2, 2, 2, 2, 2, 2, 2, 2, 2, 2, 2, 2, 2, 2, 2, 2, 2, 2, 2, 2, 2, 2, 2, 2, 2, 2, 2, 2, 2, 2, 2, 2, 2, 2, 2, 2, 2, 2, 2, 2, 2, 2, 2, 2, 2, 2, 2, 2, 2, 2, 2, 2, 2, 2, 2, 2, 2, 2, 2, 2, 2, 2, 2, 2, 2, 2, 2, 2, 2, 2, 2, 2, 2, 2, 2, 3 ),
 ( 0.000000000000000000, 1.000000000000000000 ),
 ( 0.000000000000000000, 0.007246376811594202987, 0.01449275362318840597, 0.02173913043478260809, 0.02898550724637681195, 0.03623188405797101580, 0.04347826086956521618, 0.05072463768115942351, 0.05797101449275362389, 0.06521739130434782428, 0.07246376811594203160, 0.07971014492753622505, 0.08695652173913043237, 0.09420289855072463969, 0.1014492753623188470, 0.1086956521739130405, 0.1159420289855072478, 0.1231884057971014551, 0.1304347826086956486, 0.1376811594202898559, 0.1449275362318840632, 0.1521739130434782705, 0.1594202898550724501, 0.1666666666666666574, 0.1739130434782608647, 0.1811594202898550721, 0.1884057971014492794, 0.1956521739130434867, 0.2028985507246376940, 0.2101449275362318736, 0.2173913043478260809, 0.2246376811594202882, 0.2318840579710144956, 0.2391304347826087029, 0.2463768115942029102, 0.2536231884057971175, 0.2608695652173912971, 0.2681159420289855322, 0.2753623188405797118, 0.2826086956521738913, 0.2898550724637681264, 0.2971014492753623060, 0.3043478260869565410, 0.3115942028985507206, 0.3188405797101449002, 0.3260869565217391353, 0.3333333333333333148, 0.3405797101449275499, 0.3478260869565217295, 0.3550724637681159646, 0.3623188405797101441, 0.3695652173913043237, 0.3768115942028985588, 0.3840579710144927383, 0.3913043478260869734, 0.3985507246376811530, 0.4057971014492753881, 0.4130434782608695676, 0.4202898550724637472, 0.4275362318840579823, 0.4347826086956521618, 0.4420289855072463969, 0.4492753623188405765, 0.4565217391304347561, 0.4637681159420289911, 0.4710144927536231707, 0.4782608695652174058, 0.4855072463768115854, 0.4927536231884058204, 0.5000000000000000000, 0.5072463768115942351, 0.5144927536231883591, 0.5217391304347825942, 0.5289855072463768293, 0.5362318840579710644, 0.5434782608695651884, 0.5507246376811594235, 0.5579710144927536586, 0.5652173913043477826, 0.5724637681159420177, 0.5797101449275362528, 0.5869565217391304879, 0.5942028985507246119, 0.6014492753623188470, 0.6086956521739130821, 0.6159420289855072062, 0.6231884057971014412, 0.6304347826086956763, 0.6376811594202898004, 0.6449275362318840354, 0.6521739130434782705, 0.6594202898550725056, 0.6666666666666666297, 0.6739130434782608647, 0.6811594202898550998, 0.6884057971014492239, 0.6956521739130434590, 0.7028985507246376940, 0.7101449275362319291, 0.7173913043478260532, 0.7246376811594202882, 0.7318840579710145233, 0.7391304347826086474, 0.7463768115942028825, 0.7536231884057971175, 0.7608695652173913526, 0.7681159420289854767, 0.7753623188405797118, 0.7826086956521739468, 0.7898550724637680709, 0.7971014492753623060, 0.8043478260869565410, 0.8115942028985507761, 0.8188405797101449002, 0.8260869565217391353, 0.8333333333333333703, 0.8405797101449274944, 0.8478260869565217295, 0.8550724637681159646, 0.8623188405797101996, 0.8695652173913043237, 0.8768115942028985588, 0.8840579710144927938, 0.8913043478260869179, 0.8985507246376811530, 0.9057971014492753881, 0.9130434782608695121, 0.9202898550724637472, 0.9275362318840579823, 0.9347826086956522174, 0.9420289855072463414, 0.9492753623188405765, 0.9565217391304348116, 0.9637681159420289356, 0.9662083003288912675 ),
 .UNSPECIFIED. ) 
 GEOMETRIC_REPRESENTATION_ITEM ( )  RATIONAL_B_SPLINE_SURFACE ( (
 ( 1.000000000000000000, 0.8660254037844387076, 1.000000000000000000, 0.8660254037844387076, 1.000000000000000000, 0.8660254037844387076, 1.000000000000000000, 0.8660254037844387076, 1.000000000000000000, 0.8660254037844387076, 1.000000000000000000, 0.8660254037844387076, 1.000000000000000000, 0.8660254037844387076, 1.000000000000000000, 0.8660254037844387076, 1.000000000000000000, 0.8660254037844387076, 1.000000000000000000, 0.8660254037844387076, 1.000000000000000000, 0.8660254037844387076, 1.000000000000000000, 0.8660254037844387076, 1.000000000000000000, 0.8660254037844387076, 1.000000000000000000, 0.8660254037844387076, 1.000000000000000000, 0.8660254037844387076, 1.000000000000000000, 0.8660254037844387076, 1.000000000000000000, 0.8660254037844387076, 1.000000000000000000, 0.8660254037844387076, 1.000000000000000000, 0.8660254037844387076, 1.000000000000000000, 0.8660254037844387076, 1.000000000000000000, 0.8660254037844387076, 1.000000000000000000, 0.8660254037844387076, 1.000000000000000000, 0.8660254037844387076, 1.000000000000000000, 0.8660254037844387076, 1.000000000000000000, 0.8660254037844387076, 1.000000000000000000, 0.8660254037844387076, 1.000000000000000000, 0.8660254037844387076, 1.000000000000000000, 0.8660254037844387076, 1.000000000000000000, 0.8660254037844387076, 1.000000000000000000, 0.8660254037844387076, 1.000000000000000000, 0.8660254037844387076, 1.000000000000000000, 0.8660254037844387076, 1.000000000000000000, 0.8660254037844387076, 1.000000000000000000, 0.8660254037844387076, 1.000000000000000000, 0.8660254037844387076, 1.000000000000000000, 0.8660254037844387076, 1.000000000000000000, 0.8660254037844387076, 1.000000000000000000, 0.8660254037844387076, 1.000000000000000000, 0.8660254037844387076, 1.000000000000000000, 0.8660254037844387076, 1.000000000000000000, 0.8660254037844387076, 1.000000000000000000, 0.8660254037844387076, 1.000000000000000000, 0.8660254037844387076, 1.000000000000000000, 0.8660254037844387076, 1.000000000000000000, 0.8660254037844387076, 1.000000000000000000, 0.8660254037844387076, 1.000000000000000000, 0.8660254037844387076, 1.000000000000000000, 0.8660254037844387076, 1.000000000000000000, 0.8660254037844387076, 1.000000000000000000, 0.8660254037844387076, 1.000000000000000000, 0.8660254037844387076, 1.000000000000000000, 0.8660254037844387076, 1.000000000000000000, 0.8660254037844387076, 1.000000000000000000, 0.8660254037844387076, 1.000000000000000000, 0.8660254037844387076, 1.000000000000000000, 0.8660254037844387076, 1.000000000000000000, 0.8660254037844387076, 1.000000000000000000, 0.8660254037844387076, 1.000000000000000000, 0.8660254037844387076, 1.000000000000000000, 0.8660254037844387076, 1.000000000000000000, 0.8660254037844387076, 1.000000000000000000, 0.8660254037844387076, 1.000000000000000000, 0.8660254037844387076, 1.000000000000000000, 0.8660254037844387076, 1.000000000000000000, 0.8660254037844387076, 1.000000000000000000, 0.8660254037844387076, 1.000000000000000000, 0.8660254037844387076, 1.000000000000000000, 0.8660254037844387076, 1.000000000000000000, 0.8660254037844387076, 1.000000000000000000, 0.8660254037844387076, 1.000000000000000000, 0.8660254037844387076, 1.000000000000000000, 0.8660254037844387076, 1.000000000000000000, 0.8660254037844387076, 1.000000000000000000, 0.8660254037844387076, 1.000000000000000000, 0.8660254037844387076, 1.000000000000000000, 0.8660254037844387076, 1.000000000000000000, 0.8660254037844387076, 1.000000000000000000, 0.8660254037844387076, 1.000000000000000000, 0.8660254037844387076, 1.000000000000000000, 0.8660254037844387076, 1.000000000000000000, 0.8660254037844387076, 1.000000000000000000, 0.8660254037844387076, 1.000000000000000000, 0.8660254037844387076, 1.000000000000000000, 0.8660254037844387076, 1.000000000000000000, 0.8660254037844387076, 1.000000000000000000, 0.8660254037844387076, 1.000000000000000000, 0.8660254037844387076, 1.000000000000000000, 0.8660254037844387076, 1.000000000000000000, 0.8660254037844387076, 1.000000000000000000, 0.8660254037844387076, 1.000000000000000000, 0.8660254037844387076, 1.000000000000000000, 0.8660254037844387076, 1.000000000000000000, 0.8660254037844387076, 1.000000000000000000, 0.8660254037844387076, 1.000000000000000000, 0.8660254037844387076, 1.000000000000000000, 0.8660254037844387076, 1.000000000000000000, 0.8660254037844387076, 1.000000000000000000, 0.8660254037844387076, 1.000000000000000000, 0.8660254037844387076, 1.000000000000000000, 0.8660254037844387076, 1.000000000000000000, 0.8660254037844387076, 1.000000000000000000, 0.8660254037844387076, 1.000000000000000000, 0.8660254037844387076, 1.000000000000000000, 0.8660254037844387076, 1.000000000000000000, 0.8660254037844387076, 1.000000000000000000, 0.8660254037844387076, 1.000000000000000000, 0.8660254037844387076, 1.000000000000000000, 0.8660254037844387076, 1.000000000000000000, 0.8660254037844387076, 1.000000000000000000, 0.8660254037844387076, 1.000000000000000000, 0.8660254037844387076, 1.000000000000000000, 0.8660254037844387076, 1.000000000000000000, 0.8660254037844387076, 1.000000000000000000, 0.8660254037844387076, 1.000000000000000000, 0.8660254037844387076, 1.000000000000000000, 0.8660254037844387076, 1.000000000000000000, 0.8660254037844387076, 1.000000000000000000, 0.8660254037844387076, 1.000000000000000000, 0.8660254037844387076, 1.000000000000000000, 0.8660254037844387076, 1.000000000000000000, 0.8660254037844387076, 1.000000000000000000, 0.8660254037844387076, 1.000000000000000000, 0.8660254037844387076, 1.000000000000000000, 0.8660254037844387076, 1.000000000000000000, 0.8660254037844387076, 1.000000000000000000, 0.8660254037844387076, 1.000000000000000000, 0.8660254037844387076, 1.000000000000000000, 0.8660254037844387076, 1.000000000000000000, 0.8660254037844387076, 1.000000000000000000, 0.8660254037844387076, 1.000000000000000000, 0.8660254037844387076, 1.000000000000000000, 0.8660254037844387076, 1.000000000000000000, 0.8660254037844387076, 1.000000000000000000, 0.9548846649268474263, 0.9401540970596797830),
 ( 1.000000000000000000, 0.8660254037844387076, 1.000000000000000000, 0.8660254037844387076, 1.000000000000000000, 0.8660254037844387076, 1.000000000000000000, 0.8660254037844387076, 1.000000000000000000, 0.8660254037844387076, 1.000000000000000000, 0.8660254037844387076, 1.000000000000000000, 0.8660254037844387076, 1.000000000000000000, 0.8660254037844387076, 1.000000000000000000, 0.8660254037844387076, 1.000000000000000000, 0.8660254037844387076, 1.000000000000000000, 0.8660254037844387076, 1.000000000000000000, 0.8660254037844387076, 1.000000000000000000, 0.8660254037844387076, 1.000000000000000000, 0.8660254037844387076, 1.000000000000000000, 0.8660254037844387076, 1.000000000000000000, 0.8660254037844387076, 1.000000000000000000, 0.8660254037844387076, 1.000000000000000000, 0.8660254037844387076, 1.000000000000000000, 0.8660254037844387076, 1.000000000000000000, 0.8660254037844387076, 1.000000000000000000, 0.8660254037844387076, 1.000000000000000000, 0.8660254037844387076, 1.000000000000000000, 0.8660254037844387076, 1.000000000000000000, 0.8660254037844387076, 1.000000000000000000, 0.8660254037844387076, 1.000000000000000000, 0.8660254037844387076, 1.000000000000000000, 0.8660254037844387076, 1.000000000000000000, 0.8660254037844387076, 1.000000000000000000, 0.8660254037844387076, 1.000000000000000000, 0.8660254037844387076, 1.000000000000000000, 0.8660254037844387076, 1.000000000000000000, 0.8660254037844387076, 1.000000000000000000, 0.8660254037844387076, 1.000000000000000000, 0.8660254037844387076, 1.000000000000000000, 0.8660254037844387076, 1.000000000000000000, 0.8660254037844387076, 1.000000000000000000, 0.8660254037844387076, 1.000000000000000000, 0.8660254037844387076, 1.000000000000000000, 0.8660254037844387076, 1.000000000000000000, 0.8660254037844387076, 1.000000000000000000, 0.8660254037844387076, 1.000000000000000000, 0.8660254037844387076, 1.000000000000000000, 0.8660254037844387076, 1.000000000000000000, 0.8660254037844387076, 1.000000000000000000, 0.8660254037844387076, 1.000000000000000000, 0.8660254037844387076, 1.000000000000000000, 0.8660254037844387076, 1.000000000000000000, 0.8660254037844387076, 1.000000000000000000, 0.8660254037844387076, 1.000000000000000000, 0.8660254037844387076, 1.000000000000000000, 0.8660254037844387076, 1.000000000000000000, 0.8660254037844387076, 1.000000000000000000, 0.8660254037844387076, 1.000000000000000000, 0.8660254037844387076, 1.000000000000000000, 0.8660254037844387076, 1.000000000000000000, 0.8660254037844387076, 1.000000000000000000, 0.8660254037844387076, 1.000000000000000000, 0.8660254037844387076, 1.000000000000000000, 0.8660254037844387076, 1.000000000000000000, 0.8660254037844387076, 1.000000000000000000, 0.8660254037844387076, 1.000000000000000000, 0.8660254037844387076, 1.000000000000000000, 0.8660254037844387076, 1.000000000000000000, 0.8660254037844387076, 1.000000000000000000, 0.8660254037844387076, 1.000000000000000000, 0.8660254037844387076, 1.000000000000000000, 0.8660254037844387076, 1.000000000000000000, 0.8660254037844387076, 1.000000000000000000, 0.8660254037844387076, 1.000000000000000000, 0.8660254037844387076, 1.000000000000000000, 0.8660254037844387076, 1.000000000000000000, 0.8660254037844387076, 1.000000000000000000, 0.8660254037844387076, 1.000000000000000000, 0.8660254037844387076, 1.000000000000000000, 0.8660254037844387076, 1.000000000000000000, 0.8660254037844387076, 1.000000000000000000, 0.8660254037844387076, 1.000000000000000000, 0.8660254037844387076, 1.000000000000000000, 0.8660254037844387076, 1.000000000000000000, 0.8660254037844387076, 1.000000000000000000, 0.8660254037844387076, 1.000000000000000000, 0.8660254037844387076, 1.000000000000000000, 0.8660254037844387076, 1.000000000000000000, 0.8660254037844387076, 1.000000000000000000, 0.8660254037844387076, 1.000000000000000000, 0.8660254037844387076, 1.000000000000000000, 0.8660254037844387076, 1.000000000000000000, 0.8660254037844387076, 1.000000000000000000, 0.8660254037844387076, 1.000000000000000000, 0.8660254037844387076, 1.000000000000000000, 0.8660254037844387076, 1.000000000000000000, 0.8660254037844387076, 1.000000000000000000, 0.8660254037844387076, 1.000000000000000000, 0.8660254037844387076, 1.000000000000000000, 0.8660254037844387076, 1.000000000000000000, 0.8660254037844387076, 1.000000000000000000, 0.8660254037844387076, 1.000000000000000000, 0.8660254037844387076, 1.000000000000000000, 0.8660254037844387076, 1.000000000000000000, 0.8660254037844387076, 1.000000000000000000, 0.8660254037844387076, 1.000000000000000000, 0.8660254037844387076, 1.000000000000000000, 0.8660254037844387076, 1.000000000000000000, 0.8660254037844387076, 1.000000000000000000, 0.8660254037844387076, 1.000000000000000000, 0.8660254037844387076, 1.000000000000000000, 0.8660254037844387076, 1.000000000000000000, 0.8660254037844387076, 1.000000000000000000, 0.8660254037844387076, 1.000000000000000000, 0.8660254037844387076, 1.000000000000000000, 0.8660254037844387076, 1.000000000000000000, 0.8660254037844387076, 1.000000000000000000, 0.8660254037844387076, 1.000000000000000000, 0.8660254037844387076, 1.000000000000000000, 0.8660254037844387076, 1.000000000000000000, 0.8660254037844387076, 1.000000000000000000, 0.8660254037844387076, 1.000000000000000000, 0.8660254037844387076, 1.000000000000000000, 0.8660254037844387076, 1.000000000000000000, 0.8660254037844387076, 1.000000000000000000, 0.8660254037844387076, 1.000000000000000000, 0.8660254037844387076, 1.000000000000000000, 0.8660254037844387076, 1.000000000000000000, 0.8660254037844387076, 1.000000000000000000, 0.8660254037844387076, 1.000000000000000000, 0.8660254037844387076, 1.000000000000000000, 0.8660254037844387076, 1.000000000000000000, 0.8660254037844387076, 1.000000000000000000, 0.8660254037844387076, 1.000000000000000000, 0.8660254037844387076, 1.000000000000000000, 0.8660254037844387076, 1.000000000000000000, 0.8660254037844387076, 1.000000000000000000, 0.8660254037844387076, 1.000000000000000000, 0.9548846649268474263, 0.9401540970596797830) ) ) 
 REPRESENTATION_ITEM ( '' )  SURFACE ( )  );
#54213 = CARTESIAN_POINT ( 'NONE',  ( 20.39062500061451644, -3.027376345333614438, 5.243569643749998122 ) ) ;
#54214 = CARTESIAN_POINT ( 'NONE',  ( 28.80000000122903003, -2.886751345948129988, 4.999999999999997335 ) ) ;
#54215 = CARTESIAN_POINT ( 'NONE',  ( 4.190625000614518925, -3.027376345333614438, 5.243569643749998122 ) ) ;
#54216 = CARTESIAN_POINT ( 'NONE',  ( 26.25000000000000000, 4.330127018922192761, -2.499999999999997780 ) ) ;
#54217 = CARTESIAN_POINT ( 'NONE',  ( 28.72500000000000142, -4.330127018922194537, 2.499999999999995559 ) ) ;
#54218 = CARTESIAN_POINT ( 'NONE',  ( 28.62187500061451573, -6.054752690667223547, -1.112240025338166033E-15 ) ) ;
#54219 = DIRECTION ( 'NONE',  ( 0.000000000000000000, 0.000000000000000000, 1.000000000000000000 ) ) ;
#54220 = EDGE_CURVE ( 'NONE', #26952, #66635, #53560, .T. ) ;
#54221 = CARTESIAN_POINT ( 'NONE',  ( 12.11250000122903181, 0.000000000000000000, 4.999999999999998224 ) ) ;
#54222 = CARTESIAN_POINT ( 'NONE',  ( 29.33437500061451431, 4.541064518000418104, 2.621784821874999949 ) ) ;
#54223 = DIRECTION ( 'NONE',  ( 0.000000000000000000, 0.000000000000000000, 1.000000000000000000 ) ) ;
#54224 = CARTESIAN_POINT ( 'NONE',  ( 6.984375000614516438, -4.541064518000419881, 2.621784821874995952 ) ) ;
#54225 = CARTESIAN_POINT ( 'NONE',  ( 26.69062500061451715, -3.027376345333614438, 5.243569643749998122 ) ) ;
#54226 = CARTESIAN_POINT ( 'NONE',  ( 2.655984681222220721E-16, 13.31562499938548783, 25.66244784525396483 ) ) ;
#54227 = CARTESIAN_POINT ( 'NONE',  ( 14.28749999999999964, -2.886751345948063374, 5.000000000000112799 ) ) ;
#54228 = CARTESIAN_POINT ( 'NONE',  ( 27.54375000122902506, -2.886751345948112224, -5.000000000000023981 ) ) ;
#54229 = CARTESIAN_POINT ( 'NONE',  ( 4.434375000614519280, 6.421520780324663323E-16, -5.243569643749999010 ) ) ;
#54230 = CARTESIAN_POINT ( 'NONE',  ( 9.496875000614517504, 6.054752690667223547, 3.707466751127219781E-16 ) ) ;
#54231 = CARTESIAN_POINT ( 'NONE',  ( 3.600000000000002309, -4.330127018922190985, -2.500000000000001332 ) ) ;
#54232 = CARTESIAN_POINT ( 'NONE',  ( -2.121784821874999949, 13.42812500061459602, 26.32496088578401938 ) ) ;
#54233 = CARTESIAN_POINT ( 'NONE',  ( 20.73750000000000071, -2.886751345948125991, -5.000000000000000000 ) ) ;
#54234 = CARTESIAN_POINT ( 'NONE',  ( -3.999999999999999112, 17.75000000000000355, -30.00000000000000000 ) ) ;
#54235 = CARTESIAN_POINT ( 'NONE',  ( 3.450000000000001510, 0.000000000000000000, 4.999999999999998224 ) ) ;
#54236 = CARTESIAN_POINT ( 'NONE',  ( 12.04687500061451821, 4.119189519843966529, -2.378215178124998275 ) ) ;
#54237 = EDGE_LOOP ( 'NONE', ( #44109, #38679, #15921, #45268 ) ) ;
#54238 = CARTESIAN_POINT ( 'NONE',  ( 21.32812500061451644, -4.541064518000419881, 2.621784821874995952 ) ) ;
#54239 = CARTESIAN_POINT ( 'NONE',  ( 10.19062500061451892, -3.027376345333610441, -5.243569643749999898 ) ) ;
#54240 = CARTESIAN_POINT ( 'NONE',  ( 22.88437500061451502, 5.492252693125287522, 3.363034840372157021E-16 ) ) ;
#54241 = CARTESIAN_POINT ( 'NONE',  ( 7.809375000614519280, 0.000000000000000000, 5.243569643749999010 ) ) ;
#54242 = CARTESIAN_POINT ( 'NONE',  ( 22.98749999999999716, -2.886751345948125991, -5.000000000000000000 ) ) ;
#54243 = CARTESIAN_POINT ( 'NONE',  ( 18.97500000122903074, -5.773502691896255534, -1.060575238724906372E-15 ) ) ;
#54244 = CARTESIAN_POINT ( 'NONE',  ( 27.10312500061451502, 0.000000000000000000, 5.243569643749999010 ) ) ;
#54245 = CARTESIAN_POINT ( 'NONE',  ( 1.626862140677534273E-15, 10.77500000122903323, 34.00000000000000000 ) ) ;
#54246 = CARTESIAN_POINT ( 'NONE',  ( 8.296875000614516438, -3.027376345333614438, 5.243569643749998122 ) ) ;
#54247 = CARTESIAN_POINT ( 'NONE',  ( 15.23437500061451644, 6.421520780324663323E-16, -5.243569643749999010 ) ) ;
#54248 = CARTESIAN_POINT ( 'NONE',  ( 24.19687500061451857, -3.027376345333610441, -5.243569643749999898 ) ) ;
#54249 = CARTESIAN_POINT ( 'NONE',  ( 3.999999999999998668, 18.12500000122903288, -32.30940107675850470 ) ) ;
#54250 = CARTESIAN_POINT ( 'NONE',  ( 14.17500000000000071, 4.330127018922191873, 2.499999999999999556 ) ) ;
#54251 = CARTESIAN_POINT ( 'NONE',  ( 16.77187500061451786, 3.027376345333611329, 5.243569643749999010 ) ) ;
#54252 =( BOUNDED_CURVE ( )  B_SPLINE_CURVE ( 2, ( #66228, #3457, #60305, #9716, #32249, #25976, #54782 ),
 .UNSPECIFIED., .F., .F. ) 
 B_SPLINE_CURVE_WITH_KNOTS ( ( 3, 2, 2, 3 ),
 ( 0.1916666666666666519, 0.1944444444444444198, 0.1972222222222221599, 0.1999999999999999556 ),
 .UNSPECIFIED. ) 
 CURVE ( )  GEOMETRIC_REPRESENTATION_ITEM ( )  RATIONAL_B_SPLINE_CURVE ( ( 1.000000000000001332, 0.8660254037844373753, 1.000000000000000000, 0.8660254037844387076, 1.000000000000000000, 0.8660254037844413721, 0.9999999999999973355 ) ) 
 REPRESENTATION_ITEM ( '' )  );
#54253 = CARTESIAN_POINT ( 'NONE',  ( 10.13437500061451679, -4.541064518000419881, 2.621784821874995952 ) ) ;
#54254 = CARTESIAN_POINT ( 'NONE',  ( 1.878215178124997609, 20.32812499938548356, 33.25316411605952993 ) ) ;
#54255 = CARTESIAN_POINT ( 'NONE',  ( 24.03750000000000142, 5.773502691896255534, 3.535250795749688894E-16 ) ) ;
#54256 = CARTESIAN_POINT ( 'NONE',  ( -3.999999999999999556, 14.48750000000000071, 27.69059892324149175 ) ) ;
#54257 = CARTESIAN_POINT ( 'NONE',  ( -4.243569643749999898, 9.921875000614519990, -32.45002607614398471 ) ) ;
#54258 = CARTESIAN_POINT ( 'NONE',  ( 24.94687500061451502, -2.746126346562646425, 4.756430356249996549 ) ) ;
#54259 = CARTESIAN_POINT ( 'NONE',  ( 13.52812500061451750, 4.541064518000418104, 2.621784821874999949 ) ) ;
#54260 = CARTESIAN_POINT ( 'NONE',  ( 29.40937500061451715, 0.000000000000000000, 5.243569643749999010 ) ) ;
#54261 = CARTESIAN_POINT ( 'NONE',  ( 13.21875000122903288, 2.886751345948129099, -4.999999999999997335 ) ) ;
#54262 = FACE_OUTER_BOUND ( 'NONE', #28989, .T. ) ;
#54263 =( BOUNDED_CURVE ( )  B_SPLINE_CURVE ( 2, ( #6047, #881, #57366, #51836, #23745, #28581, #4823 ),
 .UNSPECIFIED., .F., .F. ) 
 B_SPLINE_CURVE_WITH_KNOTS ( ( 3, 2, 2, 3 ),
 ( 0.5416666666666666297, 0.5444444444444443976, 0.5472222222222222765, 0.5500000000000000444 ),
 .UNSPECIFIED. ) 
 CURVE ( )  GEOMETRIC_REPRESENTATION_ITEM ( )  RATIONAL_B_SPLINE_CURVE ( ( 1.000000000000000000, 0.8660254037844387076, 1.000000000000000000, 0.8660254037844387076, 1.000000000000000000, 0.8660254037844387076, 1.000000000000000000 ) ) 
 REPRESENTATION_ITEM ( '' )  );
#54264 = CARTESIAN_POINT ( 'NONE',  ( 13.01249999999999929, -5.773502691896255534, -1.060575238724906372E-15 ) ) ;
#54265 = EDGE_CURVE ( 'NONE', #68363, #67338, #26155, .T. ) ;
#54266 = CARTESIAN_POINT ( 'NONE',  ( -2.828200636599751609E-16, 18.20000000122903216, 25.38119784648299770 ) ) ;
#54267 = CARTESIAN_POINT ( 'NONE',  ( 11.17500000122903536, 2.886751345948126879, 4.999999999999999112 ) ) ;
#54268 = CARTESIAN_POINT ( 'NONE',  ( 23.07187500061451857, 3.027376345333611329, 5.243569643749999010 ) ) ;
#54269 = CARTESIAN_POINT ( 'NONE',  ( 16.54687500061451644, -3.027376345333610441, -5.243569643749999898 ) ) ;
#54270 = CARTESIAN_POINT ( 'NONE',  ( 25.18125000122903145, -4.330127018922194537, 2.499999999999995559 ) ) ;
#54271 = ORIENTED_EDGE ( 'NONE', *, *, #6454, .F. ) ;
#54272 = CARTESIAN_POINT ( 'NONE',  ( 17.20312500061451644, 0.000000000000000000, 5.243569643749999010 ) ) ;
#54273 = CARTESIAN_POINT ( 'NONE',  ( 28.76250000122903216, 0.000000000000000000, 4.999999999999998224 ) ) ;
#54274 = CARTESIAN_POINT ( 'NONE',  ( 17.93437500061451928, 6.421520780324663323E-16, -5.243569643749999010 ) ) ;
#54275 = CARTESIAN_POINT ( 'NONE',  ( 28.47187500061451715, 3.027376345333611329, 5.243569643749999010 ) ) ;
#54276 = CARTESIAN_POINT ( 'NONE',  ( 4.340625000614515727, -3.027376345333610441, -5.243569643749999898 ) ) ;
#54277 = CARTESIAN_POINT ( 'NONE',  ( 18.77812500061451573, 6.421520780324663323E-16, -5.243569643749999010 ) ) ;
#54278 = CARTESIAN_POINT ( 'NONE',  ( 28.28437500061451715, 6.421520780324663323E-16, -5.243569643749999010 ) ) ;
#54279 = CARTESIAN_POINT ( 'NONE',  ( 4.243569643749999898, 12.37812500061451715, 30.00000000000000000 ) ) ;
#54280 = CARTESIAN_POINT ( 'NONE',  ( 16.72500000122903430, -5.773502691896255534, -1.060575238724906372E-15 ) ) ;
#54281 = CARTESIAN_POINT ( 'NONE',  ( 8.746875000614515727, -2.746126346562646425, 4.756430356249996549 ) ) ;
#54282 = CARTESIAN_POINT ( 'NONE',  ( 7.790625000614516793, -3.027376345333614438, 5.243569643749998122 ) ) ;
#54283 = CARTESIAN_POINT ( 'NONE',  ( 26.87812500061451360, 6.421520780324663323E-16, -5.243569643749999010 ) ) ;
#54284 = CARTESIAN_POINT ( 'NONE',  ( 0.000000000000000000, 0.000000000000000000, 50.00000000000000000 ) ) ;
#54285 = CARTESIAN_POINT ( 'NONE',  ( 24.04687500061451644, -3.027376345333614438, 5.243569643749998122 ) ) ;
#54286 = CARTESIAN_POINT ( 'NONE',  ( 12.77812500061451750, -4.541064518000419881, 2.621784821874995952 ) ) ;
#54287 = CARTESIAN_POINT ( 'NONE',  ( 22.68750000122903288, 6.123233995736764310E-16, -4.999999999999998224 ) ) ;
#54288 =( BOUNDED_CURVE ( )  B_SPLINE_CURVE ( 2, ( #17878, #927, #28269, #6455, #23435, #62954, #12349, #34884, #29706 ),
 .UNSPECIFIED., .F., .F. ) 
 B_SPLINE_CURVE_WITH_KNOTS ( ( 3, 2, 2, 2, 3 ),
 ( 0.2500000000000000000, 0.2536231884057971175, 0.2608695652173912971, 0.2681159420289855322, 0.2717391304347826497 ),
 .UNSPECIFIED. ) 
 CURVE ( )  GEOMETRIC_REPRESENTATION_ITEM ( )  RATIONAL_B_SPLINE_CURVE ( ( 0.9330127018922194093, 0.9330127018922190762, 1.000000000000000000, 0.8660254037844387076, 1.000000000000000000, 0.8660254037844387076, 1.000000000000000000, 0.9330127018922188542, 0.9330127018922194093 ) ) 
 REPRESENTATION_ITEM ( '' )  );
#54289 = CARTESIAN_POINT ( 'NONE',  ( 22.41562500061451502, 3.027376345333613106, -5.243569643749998122 ) ) ;
#54290 = CARTESIAN_POINT ( 'NONE',  ( 18.42187500061451644, 3.027376345333613106, -5.243569643749998122 ) ) ;
#54291 = CARTESIAN_POINT ( 'NONE',  ( 12.32812500061451821, -4.541064518000419881, 2.621784821874995952 ) ) ;
#54292 = CARTESIAN_POINT ( 'NONE',  ( -3.000416591977282496E-16, 15.69687500061451857, 25.09994784771203058 ) ) ;
#54293 = CARTESIAN_POINT ( 'NONE',  ( 18.89062500061451644, 6.054752690667223547, 3.707466751127219781E-16 ) ) ;
#54294 = CARTESIAN_POINT ( 'NONE',  ( -1.626862140677534273E-15, 17.78749999999999787, 34.00000000000000000 ) ) ;
#54295 = ORIENTED_EDGE ( 'NONE', *, *, #38095, .F. ) ;
#54296 = ORIENTED_EDGE ( 'NONE', *, *, #24479, .F. ) ;
#54297 = CARTESIAN_POINT ( 'NONE',  ( 22.72499999999999787, 4.330127018922191873, 2.499999999999999556 ) ) ;
#54298 = CARTESIAN_POINT ( 'NONE',  ( -1.389182184750238802, 10.01354716596406824, -33.81675744519802151 ) ) ;
#54299 = FACE_OUTER_BOUND ( 'NONE', #49206, .T. ) ;
#54300 = CARTESIAN_POINT ( 'NONE',  ( 26.42812500061451431, 6.421520780324663323E-16, -5.243569643749999010 ) ) ;
#54301 = CARTESIAN_POINT ( 'NONE',  ( 4.978125000614518569, 4.541064518000418104, 2.621784821874999949 ) ) ;
#54302 = CARTESIAN_POINT ( 'NONE',  ( 18.86250000122903359, 0.000000000000000000, 4.999999999999998224 ) ) ;
#54303 = CARTESIAN_POINT ( 'NONE',  ( 25.07812500061451644, 6.421520780324663323E-16, -5.243569643749999010 ) ) ;
#54304 = CARTESIAN_POINT ( 'NONE',  ( 23.25000000000000000, 0.000000000000000000, 4.999999999999998224 ) ) ;
#54305 = CARTESIAN_POINT ( 'NONE',  ( 27.59062500061451573, -3.027376345333614438, 5.243569643749998122 ) ) ;
#54306 = CARTESIAN_POINT ( 'NONE',  ( 7.903125000614515727, -4.541064518000417216, -2.621784821875001281 ) ) ;
#54307 = ORIENTED_EDGE ( 'NONE', *, *, #29408, .F. ) ;
#54308 = CARTESIAN_POINT ( 'NONE',  ( 24.40312500061451573, 0.000000000000000000, 5.243569643749999010 ) ) ;
#54309 = CARTESIAN_POINT ( 'NONE',  ( 6.103125000614515905, -4.541064518000417216, -2.621784821875001281 ) ) ;
#54310 = UNCERTAINTY_MEASURE_WITH_UNIT (LENGTH_MEASURE( 1.000000000000000082E-05 ), #71243, 'distance_accuracy_value', 'NONE');
#54311 = CARTESIAN_POINT ( 'NONE',  ( 14.93437500061451750, 4.119189519843966529, 2.378215178124999607 ) ) ;
#54312 = CARTESIAN_POINT ( 'NONE',  ( 2.953125000614516438, -4.541064518000417216, -2.621784821875001281 ) ) ;
#54313 = AXIS2_PLACEMENT_3D ( 'NONE', #3991, #42414, #47957 ) ;
#54314 = CARTESIAN_POINT ( 'NONE',  ( -2.828200636599751609E-16, 13.70000000122903572, -34.61880215351700230 ) ) ;
#54315 = CARTESIAN_POINT ( 'NONE',  ( 1.626862140677534273E-15, 10.66249999999999964, -26.00000000000000355 ) ) ;
#54316 = CARTESIAN_POINT ( 'NONE',  ( 10.16249999999999964, 2.886751345948126879, 4.999999999999999112 ) ) ;
#54317 = CARTESIAN_POINT ( 'NONE',  ( 12.27187500061451786, 3.027376345333611329, 5.243569643749999010 ) ) ;
#54318 = CARTESIAN_POINT ( 'NONE',  ( 5.887500001229034829, -4.330127018922194537, 2.499999999999995559 ) ) ;
#54319 = CARTESIAN_POINT ( 'NONE',  ( 13.73437500061451821, -4.541064518000419881, 2.621784821874995952 ) ) ;
#54320 = CARTESIAN_POINT ( 'NONE',  ( 16.05000000000000071, 0.000000000000000000, 4.999999999999998224 ) ) ;
#54321 = CARTESIAN_POINT ( 'NONE',  ( 5.521875000614517859, 3.027376345333611329, 5.243569643749999010 ) ) ;
#54322 = CARTESIAN_POINT ( 'NONE',  ( 1.071796769724493892, 18.51740381056766793, 26.00000000000000711 ) ) ;
#54323 = CARTESIAN_POINT ( 'NONE',  ( 24.82499999999999929, 6.123233995736764310E-16, -4.999999999999998224 ) ) ;
#54324 = CARTESIAN_POINT ( 'NONE',  ( 11.59687500061451892, -3.027376345333610441, -5.243569643749999898 ) ) ;
#54325 = DIRECTION ( 'NONE',  ( -1.000000000000000000, -0.000000000000000000, -0.000000000000000000 ) ) ;
#54326 = CARTESIAN_POINT ( 'NONE',  ( 21.25312500061451715, 0.000000000000000000, 5.243569643749999010 ) ) ;
#54327 = CARTESIAN_POINT ( 'NONE',  ( 2.121784821874999061, 10.70937500061451964, 26.32496088578401583 ) ) ;
#54328 = CARTESIAN_POINT ( 'NONE',  ( 24.94687500061451502, -3.027376345333614438, 5.243569643749998122 ) ) ;
#54329 = CARTESIAN_POINT ( 'NONE',  ( 29.55000000000000071, 0.000000000000000000, 4.999999999999998224 ) ) ;
#54330 = CARTESIAN_POINT ( 'NONE',  ( 3.778125000614519280, -4.541064518000419881, 2.621784821874995952 ) ) ;
#54331 = ADVANCED_FACE ( 'NONE', ( #20958 ), #31692, .T. ) ;
#54332 = CARTESIAN_POINT ( 'NONE',  ( 23.25937500061451502, 2.746126346562645981, -4.756430356249997438 ) ) ;
#54333 = CARTESIAN_POINT ( 'NONE',  ( 14.33437500061451786, 6.421520780324663323E-16, -5.243569643749999010 ) ) ;
#54334 = CARTESIAN_POINT ( 'NONE',  ( 26.81250000122903288, 4.330127018922192761, -2.499999999999997780 ) ) ;
#54335 = CARTESIAN_POINT ( 'NONE',  ( 4.921875000614518214, 3.027376345333613106, -5.243569643749998122 ) ) ;
#54336 = CARTESIAN_POINT ( 'NONE',  ( 16.99687500061451573, -3.027376345333610441, -5.243569643749999898 ) ) ;
#54337 = CARTESIAN_POINT ( 'NONE',  ( 14.92500000000000071, 6.123233995736764310E-16, -4.999999999999998224 ) ) ;
#54338 = CARTESIAN_POINT ( 'NONE',  ( 25.12499999999999645, -4.330127018922194537, 2.499999999999995559 ) ) ;
#54339 = CARTESIAN_POINT ( 'NONE',  ( 3.862500001229035362, 4.330127018922192761, -2.499999999999997780 ) ) ;
#54340 = CARTESIAN_POINT ( 'NONE',  ( 26.03437500061451715, 6.421520780324663323E-16, -5.243569643749999010 ) ) ;
#54341 = CARTESIAN_POINT ( 'NONE',  ( -1.878215178124999163, 14.25312499938548250, 26.74683588394047007 ) ) ;
#54342 = CARTESIAN_POINT ( 'NONE',  ( 8.718750001229031099, 2.886751345948073588, -5.000000000000094147 ) ) ;
#54343 = CARTESIAN_POINT ( 'NONE',  ( 7.275000000000000355, 6.123233995736764310E-16, -4.999999999999998224 ) ) ;
#54344 = CARTESIAN_POINT ( 'NONE',  ( 10.24687500061451395, 4.119189519843966529, -2.378215178124998275 ) ) ;
#54345 = CARTESIAN_POINT ( 'NONE',  ( 22.79062500061451502, -3.027376345333610441, -5.243569643749999898 ) ) ;
#54346 = CARTESIAN_POINT ( 'NONE',  ( 11.21250000000000036, -5.773502691896255534, -1.060575238724906372E-15 ) ) ;
#54347 = CARTESIAN_POINT ( 'NONE',  ( 3.965625000614515727, 3.027376345333613106, -5.243569643749998122 ) ) ;
#54348 = CARTESIAN_POINT ( 'NONE',  ( 18.93750000000000000, -2.886751345948125991, -5.000000000000000000 ) ) ;
#54349 = EDGE_CURVE ( 'NONE', #8399, #29691, #7683, .T. ) ;
#54350 = CARTESIAN_POINT ( 'NONE',  ( 17.61562500061451786, 3.027376345333611329, 5.243569643749999010 ) ) ;
#54351 = CARTESIAN_POINT ( 'NONE',  ( 15.60000000122903607, 5.773502691896255534, 3.535250795749688401E-16 ) ) ;
#54352 = CARTESIAN_POINT ( 'NONE',  ( 22.50000000122903288, -2.886751345948129988, 4.999999999999997335 ) ) ;
#54353 = CARTESIAN_POINT ( 'NONE',  ( 3.756430356250000102, 19.39062499938548356, 30.00000000000000000 ) ) ;
#54354 = CARTESIAN_POINT ( 'NONE',  ( 29.59687500061451715, -3.027376345333610441, -5.243569643749999898 ) ) ;
#54355 = ORIENTED_EDGE ( 'NONE', *, *, #51734, .T. ) ;
#54356 = CARTESIAN_POINT ( 'NONE',  ( 18.96562500061451573, 3.027376345333611329, 5.243569643749999010 ) ) ;
#54357 = CARTESIAN_POINT ( 'NONE',  ( 24.25312500061451715, 4.541064518000418104, -2.621784821874998173 ) ) ;
#54358 = CARTESIAN_POINT ( 'NONE',  ( 25.65937500061451715, 4.541064518000418104, -2.621784821874998173 ) ) ;
#54359 = CARTESIAN_POINT ( 'NONE',  ( 8.887499999999999289, -2.886751345948129988, 4.999999999999997335 ) ) ;
#54360 = CARTESIAN_POINT ( 'NONE',  ( 11.24062500061451608, 6.054752690667223547, 3.707466751127219781E-16 ) ) ;
#54361 = CARTESIAN_POINT ( 'NONE',  ( 27.02812500061451573, 4.541064518000418104, 2.621784821874999949 ) ) ;
#54362 = CARTESIAN_POINT ( 'NONE',  ( 17.52187500061451431, 3.027376345333613106, -5.243569643749998122 ) ) ;
#54363 = CARTESIAN_POINT ( 'NONE',  ( 8.915625000614515017, 3.027376345333613106, -5.243569643749998122 ) ) ;
#54364 = CARTESIAN_POINT ( 'NONE',  ( 4.243569643749999898, 10.18437500061451750, 30.00000000000000000 ) ) ;
#54365 = CARTESIAN_POINT ( 'NONE',  ( 23.06250000122903288, -4.330127018922190985, -2.500000000000001332 ) ) ;
#54366 = CARTESIAN_POINT ( 'NONE',  ( 16.09687500061451715, -2.746126346562641984, -4.756430356249999214 ) ) ;
#54367 = CARTESIAN_POINT ( 'NONE',  ( 14.76562500061451644, 3.027376345333612662, -5.243569643749998122 ) ) ;
#54368 = CARTESIAN_POINT ( 'NONE',  ( 7.921875000614517326, -6.054752690667223547, -1.112240025338166033E-15 ) ) ;
#54369 = CARTESIAN_POINT ( 'NONE',  ( 6.159375000614517148, -4.541064518000417216, -2.621784821875001281 ) ) ;
#54370 = VERTEX_POINT ( 'NONE', #71949 ) ;
#54371 = CARTESIAN_POINT ( 'NONE',  ( 15.33750000000000036, -2.886751345948126435, -5.000000000000000000 ) ) ;
#54372 = CARTESIAN_POINT ( 'NONE',  ( 21.17812500061451431, 4.541064518000418104, 2.621784821874999949 ) ) ;
#54373 = CARTESIAN_POINT ( 'NONE',  ( 15.75937500061451857, 4.541064518000418104, -2.621784821874998173 ) ) ;
#54374 = CARTESIAN_POINT ( 'NONE',  ( 19.19062500061452070, -3.027376345333610441, -5.243569643749999898 ) ) ;
#54375 = CARTESIAN_POINT ( 'NONE',  ( -1.999999999999997113, 11.52500000000000036, 33.46410161513775705 ) ) ;
#54376 = CARTESIAN_POINT ( 'NONE',  ( 27.25312500061451360, -4.541064518000417216, -2.621784821875001281 ) ) ;
#54377 = CARTESIAN_POINT ( 'NONE',  ( 5.962500001229033231, -4.330127018922190985, -2.500000000000001332 ) ) ;
#54378 = ORIENTED_EDGE ( 'NONE', *, *, #43656, .T. ) ;
#54379 = CARTESIAN_POINT ( 'NONE',  ( 29.69999999999999574, -4.330127018922190985, -2.500000000000001332 ) ) ;
#54380 = CARTESIAN_POINT ( 'NONE',  ( 3.999999999999998668, 18.91249999999999787, -32.30940107675850470 ) ) ;
#54381 = CARTESIAN_POINT ( 'NONE',  ( 24.37500000122903288, -5.773502691896255534, -1.060575238724906372E-15 ) ) ;
#54382 = CARTESIAN_POINT ( 'NONE',  ( -3.756430356249999214, 15.19062499938548250, 27.83122392262697531 ) ) ;
#54383 = CARTESIAN_POINT ( 'NONE',  ( 7.171875000614517326, 3.027376345333613106, -5.243569643749998122 ) ) ;
#54384 = CARTESIAN_POINT ( 'NONE',  ( 4.869423765992945796, -1.135214599616954256, -5.119209941160161037 ) ) ;
#54385 = CARTESIAN_POINT ( 'NONE',  ( 15.21562500061451750, 3.027376345333613106, -5.243569643749998122 ) ) ;
#54386 = CARTESIAN_POINT ( 'NONE',  ( 9.684375000614517504, -4.541064518000419881, 2.621784821874995952 ) ) ;
#54387 = CARTESIAN_POINT ( 'NONE',  ( 27.97500000122903074, -5.773502691896255534, -1.060575238724906372E-15 ) ) ;
#54388 = CARTESIAN_POINT ( 'NONE',  ( 17.48437500061451999, 6.421520780324663323E-16, -5.243569643749999010 ) ) ;
#54389 = CARTESIAN_POINT ( 'NONE',  ( 4.921875000614518214, 3.027376345333613106, -5.243569643749998122 ) ) ;
#54390 = CARTESIAN_POINT ( 'NONE',  ( 5.165625000614518569, -6.054752690667223547, -1.112240025338166033E-15 ) ) ;
#54391 = CARTESIAN_POINT ( 'NONE',  ( 15.29062500061451679, 6.054752690667223547, 3.707466751127219781E-16 ) ) ;
#54392 = VERTEX_POINT ( 'NONE', #32057 ) ;
#54393 = CARTESIAN_POINT ( 'NONE',  ( 11.69062500061451360, 6.054752690667223547, 3.707466751127219781E-16 ) ) ;
#54394 = CARTESIAN_POINT ( 'NONE',  ( 6.412500001229036073, -4.330127018922190985, -2.500000000000001332 ) ) ;
#54395 = CARTESIAN_POINT ( 'NONE',  ( 8.465625000614515727, 3.027376345333613106, -5.243569643749998122 ) ) ;
#54396 = CARTESIAN_POINT ( 'NONE',  ( 21.98437500061451644, 5.824947211148865298E-16, -4.756430356249998326 ) ) ;
#54397 = CARTESIAN_POINT ( 'NONE',  ( 9.487500000000000711, -2.886751345948125991, -5.000000000000000000 ) ) ;
#54398 = CARTESIAN_POINT ( 'NONE',  ( 3.225000001229033408, -5.773502691896255534, -1.060575238724906372E-15 ) ) ;
#54399 = CARTESIAN_POINT ( 'NONE',  ( 19.08750000000000213, 5.773502691896255534, 3.535250795749688894E-16 ) ) ;
#54400 = CARTESIAN_POINT ( 'NONE',  ( 17.55937500061451573, 4.541064518000418104, -2.621784821874998173 ) ) ;
#54401 = CARTESIAN_POINT ( 'NONE',  ( 15.03750000122903252, 6.123233995736764310E-16, -4.999999999999998224 ) ) ;
#54402 = CARTESIAN_POINT ( 'NONE',  ( 21.11249999999999716, -5.773502691896255534, -1.060575238724906372E-15 ) ) ;
#54403 = CARTESIAN_POINT ( 'NONE',  ( -2.121784821874999949, 16.57812500061451644, -33.67503911421598417 ) ) ;
#54404 = DIRECTION ( 'NONE',  ( -1.000000000000000000, -0.000000000000000000, -0.000000000000000000 ) ) ;
#54405 = CARTESIAN_POINT ( 'NONE',  ( 1.626862140677534273E-15, 18.76250000000000284, 34.00000000000000000 ) ) ;
#54406 = DIRECTION ( 'NONE',  ( 1.000000000000000000, 0.000000000000000000, 0.000000000000000000 ) ) ;
#54407 = CARTESIAN_POINT ( 'NONE',  ( 0.000000000000000000, 27.50000000000000000, 30.00000000000000000 ) ) ;
#54408 = DIRECTION ( 'NONE',  ( 0.000000000000000000, 0.000000000000000000, 1.000000000000000000 ) ) ;
#54409 = CARTESIAN_POINT ( 'NONE',  ( 4.661467738957717266, -1.808512791952580301, -4.661467738957749241 ) ) ;
#54410 = CARTESIAN_POINT ( 'NONE',  ( 15.38437500061451679, 4.541064518000418104, 2.621784821874999949 ) ) ;
#54411 = CARTESIAN_POINT ( 'NONE',  ( 29.32499999999999929, 6.123233995736764310E-16, -4.999999999999998224 ) ) ;
#54412 = CARTESIAN_POINT ( 'NONE',  ( 10.56562500061451715, -6.054752690667223547, -1.112240025338166033E-15 ) ) ;
#54413 = CARTESIAN_POINT ( 'NONE',  ( 7.593750001229034652, -2.886751345948129988, 4.999999999999997335 ) ) ;
#54414 = CARTESIAN_POINT ( 'NONE',  ( 20.44687500061451857, -3.027376345333614438, 5.243569643749998122 ) ) ;
#54415 = CARTESIAN_POINT ( 'NONE',  ( 15.12187500061451573, 5.824947211148865298E-16, -4.756430356249998326 ) ) ;
#54416 = CARTESIAN_POINT ( 'NONE',  ( 8.803125000614517859, -4.541064518000417216, -2.621784821875001281 ) ) ;
#54417 = CARTESIAN_POINT ( 'NONE',  ( 13.62187500061451750, 3.027376345333611329, 5.243569643749999010 ) ) ;
#54418 = ORIENTED_EDGE ( 'NONE', *, *, #9015, .T. ) ;
#54419 = CARTESIAN_POINT ( 'NONE',  ( 23.03437500061451715, 4.541064518000418104, 2.621784821874999949 ) ) ;
#54420 = CARTESIAN_POINT ( 'NONE',  ( 27.59062500061451573, -3.027376345333614438, 5.243569643749998122 ) ) ;
#54421 = EDGE_CURVE ( 'NONE', #55550, #49922, #61122, .T. ) ;
#54422 = CARTESIAN_POINT ( 'NONE',  ( 26.09999999999999787, -4.330127018922190985, -2.500000000000001332 ) ) ;
#54423 = CARTESIAN_POINT ( 'NONE',  ( 6.637500000000001066, -2.886751345948129988, 4.999999999999997335 ) ) ;
#54424 = CARTESIAN_POINT ( 'NONE',  ( 16.35000000122903430, -2.886751345948125991, -5.000000000000000000 ) ) ;
#54425 = CARTESIAN_POINT ( 'NONE',  ( 28.64999999999999858, 0.000000000000000000, 4.999999999999998224 ) ) ;
#54426 = CARTESIAN_POINT ( 'NONE',  ( 9.046875000614514661, 0.000000000000000000, 4.756430356249998326 ) ) ;
#54427 = AXIS2_PLACEMENT_3D ( 'NONE', #57886, #69716, #53824 ) ;
#54428 = ORIENTED_EDGE ( 'NONE', *, *, #27670, .T. ) ;
#54429 = CARTESIAN_POINT ( 'NONE',  ( 14.43750000000000000, -2.886751345948125991, -5.000000000000000000 ) ) ;
#54430 = CARTESIAN_POINT ( 'NONE',  ( 18.97499999999999787, 6.123233995736764310E-16, -4.999999999999998224 ) ) ;
#54431 = CARTESIAN_POINT ( 'NONE',  ( 10.19062500061451892, -3.027376345333610441, -5.243569643749999898 ) ) ;
#54432 = VERTEX_POINT ( 'NONE', #54590 ) ;
#54433 = CARTESIAN_POINT ( 'NONE',  ( -3.999999999999999112, 11.00000000000000178, -30.00000000000000000 ) ) ;
#54434 = CARTESIAN_POINT ( 'NONE',  ( -2.121784821874996840, 16.78437500061452070, -26.32496088578401583 ) ) ;
#54435 = CARTESIAN_POINT ( 'NONE',  ( 4.603125000614518569, 0.000000000000000000, 5.243569643749999010 ) ) ;
#54436 = DIRECTION ( 'NONE',  ( 0.000000000000000000, 0.000000000000000000, -1.000000000000000000 ) ) ;
#54437 = CARTESIAN_POINT ( 'NONE',  ( 10.31250000000000355, -5.773502691896255534, -1.060575238724906372E-15 ) ) ;
#54438 = CARTESIAN_POINT ( 'NONE',  ( -1.071796769724488563, 13.34240381056766545, -26.00000000000000000 ) ) ;
#54439 = ORIENTED_EDGE ( 'NONE', *, *, #51854, .F. ) ;
#54440 = CARTESIAN_POINT ( 'NONE',  ( 4.243569643749999898, 11.89062500061451644, 32.45002607614398471 ) ) ;
#54441 = CARTESIAN_POINT ( 'NONE',  ( 27.25312500061451360, -4.541064518000417216, -2.621784821875001281 ) ) ;
#54442 = CARTESIAN_POINT ( 'NONE',  ( 3.548580288327752630, 3.522439202781492806, 3.649653710620935243 ) ) ;
#54443 = CARTESIAN_POINT ( 'NONE',  ( 1.878215178124997609, 18.86562499938548143, 33.25316411605952993 ) ) ;
#54444 = CARTESIAN_POINT ( 'NONE',  ( 20.63437500061451857, 6.421520780324663323E-16, -5.243569643749999010 ) ) ;
#54445 = CARTESIAN_POINT ( 'NONE',  ( 20.12812500061451715, 6.421520780324663323E-16, -5.243569643749999010 ) ) ;
#54446 = CARTESIAN_POINT ( 'NONE',  ( 4.243569643749999898, 12.79062500061459495, -27.54997392385601529 ) ) ;
#54447 = CARTESIAN_POINT ( 'NONE',  ( 22.35000000122903074, 5.773502691896255534, 3.535250795749688894E-16 ) ) ;
#54448 = CARTESIAN_POINT ( 'NONE',  ( 3.253125000614518036, 0.000000000000000000, 5.243569643749999010 ) ) ;
#54449 = CARTESIAN_POINT ( 'NONE',  ( 27.27187500061451431, -5.492252693125287522, -1.008910452111647106E-15 ) ) ;
#54450 = CARTESIAN_POINT ( 'NONE',  ( 22.11562500061451431, 3.027376345333611329, 5.243569643749999010 ) ) ;
#54451 = CYLINDRICAL_SURFACE ( 'NONE', #38600, 4.999999999999998224 ) ;
#54452 = CARTESIAN_POINT ( 'NONE',  ( -7.967954043666661671E-16, 15.67812499938548321, 34.33755215474603517 ) ) ;
#54453 = CARTESIAN_POINT ( 'NONE',  ( 16.02187500061451786, -6.054752690667223547, -1.112240025338166033E-15 ) ) ;
#54454 = CARTESIAN_POINT ( 'NONE',  ( 13.43437500061451750, 6.421520780324663323E-16, -5.243569643749999010 ) ) ;
#54455 = CARTESIAN_POINT ( 'NONE',  ( 24.12187500061451217, -6.054752690667223547, -1.112240025338166033E-15 ) ) ;
#54456 = CARTESIAN_POINT ( 'NONE',  ( 4.243569643749999898, 14.19687500061452035, 32.45002607614398471 ) ) ;
#54457 = CARTESIAN_POINT ( 'NONE',  ( 6.215625000614517504, 3.027376345333613106, -5.243569643749998122 ) ) ;
#54458 = CARTESIAN_POINT ( 'NONE',  ( 29.57812500061451644, 6.421520780324663323E-16, -5.243569643749999010 ) ) ;
#54459 = CARTESIAN_POINT ( 'NONE',  ( 28.11562500061451431, -6.054752690667223547, -1.112240025338166033E-15 ) ) ;
#54460 = FACE_OUTER_BOUND ( 'NONE', #11172, .T. ) ;
#54461 = DIRECTION ( 'NONE',  ( -0.000000000000000000, -1.000000000000000000, -0.000000000000000000 ) ) ;
#54462 = CARTESIAN_POINT ( 'NONE',  ( 7.321875000614516793, 3.027376345333611329, 5.243569643749999010 ) ) ;
#54463 = APPLICATION_PROTOCOL_DEFINITION ( 'draft international standard', 'automotive_design', 1998, #21462 ) ;
#54464 = CARTESIAN_POINT ( 'NONE',  ( 15.00000000122903465, -2.886751345948125991, -5.000000000000000000 ) ) ;
#54465 = CARTESIAN_POINT ( 'NONE',  ( 8.850000001229034297, 5.773502691896255534, 3.535250795749688894E-16 ) ) ;
#54466 = CARTESIAN_POINT ( 'NONE',  ( 4.940625000614515372, 6.054752690667223547, 3.707466751127219781E-16 ) ) ;
#54467 = CARTESIAN_POINT ( 'NONE',  ( 2.000000000000000444, 16.56874999877096499, 26.53589838486224650 ) ) ;
#54468 = CARTESIAN_POINT ( 'NONE',  ( 18.50625000122903430, -4.330127018922190985, -2.500000000000001332 ) ) ;
#54469 = CARTESIAN_POINT ( 'NONE',  ( 13.77187500061451786, -6.054752690667223547, -1.112240025338166033E-15 ) ) ;
#54470 = CARTESIAN_POINT ( 'NONE',  ( 7.500000000000000000, 0.000000000000000000, 4.999999999999998224 ) ) ;
#54471 = ORIENTED_EDGE ( 'NONE', *, *, #43566, .F. ) ;
#54472 = CARTESIAN_POINT ( 'NONE',  ( 21.29062500061451502, -3.027376345333614438, 5.243569643749998122 ) ) ;
#54473 = CARTESIAN_POINT ( 'NONE',  ( 7.903125000614515727, -4.541064518000417216, -2.621784821875001281 ) ) ;
#54474 = CARTESIAN_POINT ( 'NONE',  ( 25.28437500061451715, 4.541064518000418104, 2.621784821874999949 ) ) ;
#54475 = CARTESIAN_POINT ( 'NONE',  ( 6.890625000614516438, -3.027376345333614438, 5.243569643749998122 ) ) ;
#54476 = DIRECTION ( 'NONE',  ( -0.000000000000000000, -1.000000000000000000, -0.000000000000000000 ) ) ;
#54477 = CARTESIAN_POINT ( 'NONE',  ( 8.775000001229033231, 2.886751345948129099, -4.999999999999998224 ) ) ;
#54478 = CARTESIAN_POINT ( 'NONE',  ( 21.62812500061451360, 4.541064518000418104, 2.621784821874999949 ) ) ;
#54479 = CARTESIAN_POINT ( 'NONE',  ( -3.000416591977282496E-16, 10.69062500061451715, -34.90005215228797653 ) ) ;
#54480 = CARTESIAN_POINT ( 'NONE',  ( 10.46250000122903323, -4.330127018922190985, -2.500000000000001332 ) ) ;
#54481 = CARTESIAN_POINT ( 'NONE',  ( 18.74062500061451431, -3.027376345333610441, -5.243569643749999898 ) ) ;
#54482 = CARTESIAN_POINT ( 'NONE',  ( 19.15312500061451573, -4.541064518000417216, -2.621784821875001281 ) ) ;
#54483 = CARTESIAN_POINT ( 'NONE',  ( 29.40937500061451715, 0.000000000000000000, 4.756430356249998326 ) ) ;
#54484 = CARTESIAN_POINT ( 'NONE',  ( 19.12500000000000000, 4.330127018922191873, 2.499999999999999556 ) ) ;
#54485 = CARTESIAN_POINT ( 'NONE',  ( 12.26250000122903394, -4.330127018922190985, -2.500000000000001332 ) ) ;
#54486 = CARTESIAN_POINT ( 'NONE',  ( 8.315625000614515372, -6.054752690667223547, -1.112240025338166033E-15 ) ) ;
#54487 = CARTESIAN_POINT ( 'NONE',  ( 10.52812500061451750, -4.541064518000419881, 2.621784821874995952 ) ) ;
#54488 =( BOUNDED_CURVE ( )  B_SPLINE_CURVE ( 2, ( #6747, #855, #487, #68088, #72901, #44835, #34086, #35177, #50376 ),
 .UNSPECIFIED., .F., .F. ) 
 B_SPLINE_CURVE_WITH_KNOTS ( ( 3, 2, 2, 2, 3 ),
 ( 0.7934782608695651884, 0.7971014492753623060, 0.8043478260869565410, 0.8115942028985507761, 0.8152173913043478937 ),
 .UNSPECIFIED. ) 
 CURVE ( )  GEOMETRIC_REPRESENTATION_ITEM ( )  RATIONAL_B_SPLINE_CURVE ( ( 0.9330127018922194093, 0.9330127018922194093, 1.000000000000000000, 0.8660254037844387076, 1.000000000000000000, 0.8660254037844387076, 1.000000000000000000, 0.9330127018922182991, 0.9330127018922192983 ) ) 
 REPRESENTATION_ITEM ( '' )  );
#54489 = EDGE_CURVE ( 'NONE', #67390, #46076, #65854, .T. ) ;
#54490 = CARTESIAN_POINT ( 'NONE',  ( 22.20000000122903216, -2.886751345948125991, -5.000000000000000000 ) ) ;
#54491 = CARTESIAN_POINT ( 'NONE',  ( 21.38437500061451502, -4.541064518000419881, 2.621784821874995952 ) ) ;
#54492 = CARTESIAN_POINT ( 'NONE',  ( -2.000000000000001776, 18.64999999999999858, 33.46410161513775705 ) ) ;
#54493 = CARTESIAN_POINT ( 'NONE',  ( 5.062500001229035540, -4.330127018922190985, -2.500000000000001332 ) ) ;
#54494 = CARTESIAN_POINT ( 'NONE',  ( 4.996875000614516615, 6.054752690667223547, 3.707466751127219781E-16 ) ) ;
#54495 = CARTESIAN_POINT ( 'NONE',  ( 22.99687500061451573, 6.054752690667223547, 3.707466751127219781E-16 ) ) ;
#54496 = CARTESIAN_POINT ( 'NONE',  ( 4.342984975361706468, -2.477595912125914790, -4.621313785610477787 ) ) ;
#54497 = CARTESIAN_POINT ( 'NONE',  ( 19.94062500061451715, -3.027376345333614438, 5.243569643749998122 ) ) ;
#54498 = CARTESIAN_POINT ( 'NONE',  ( 24.38437500061451502, 4.541064518000418104, 2.621784821874999949 ) ) ;
#54499 = CARTESIAN_POINT ( 'NONE',  ( -1.878215178125001827, 18.90312499938548285, 33.25316411605952283 ) ) ;
#54500 = CARTESIAN_POINT ( 'NONE',  ( 0.000000000000000000, 27.50000000000000000, 30.00000000000000000 ) ) ;
#54501 = CARTESIAN_POINT ( 'NONE',  ( 5.371875000614516615, 3.027376345333613106, -5.243569643749998122 ) ) ;
#54502 = CARTESIAN_POINT ( 'NONE',  ( 15.47812500061451679, -4.541064518000419881, 2.621784821874995952 ) ) ;
#54503 = CARTESIAN_POINT ( 'NONE',  ( 13.99687500061451928, 6.054752690667223547, 3.707466751127219781E-16 ) ) ;
#54504 = ORIENTED_EDGE ( 'NONE', *, *, #65415, .F. ) ;
#54505 = DIRECTION ( 'NONE',  ( -1.000000000000000000, -0.000000000000000000, -0.000000000000000000 ) ) ;
#54506 = CARTESIAN_POINT ( 'NONE',  ( 26.16562500061451502, 3.027376345333611329, 5.243569643749999010 ) ) ;
#54507 = DIRECTION ( 'NONE',  ( -0.000000000000000000, -1.000000000000000000, -0.000000000000000000 ) ) ;
#54508 = CARTESIAN_POINT ( 'NONE',  ( 14.81250000000000000, -5.773502691896255534, -1.060575238724906372E-15 ) ) ;
#54509 = CARTESIAN_POINT ( 'NONE',  ( 24.07500000122903216, 2.886751345948129099, -4.999999999999998224 ) ) ;
#54510 = CARTESIAN_POINT ( 'NONE',  ( 18.36562500061451431, 3.027376345333613106, -5.243569643749998122 ) ) ;
#54511 = ORIENTED_EDGE ( 'NONE', *, *, #64554, .T. ) ;
#54512 = CARTESIAN_POINT ( 'NONE',  ( 23.51249999999999574, 2.886751345948129099, -4.999999999999998224 ) ) ;
#54513 = CARTESIAN_POINT ( 'NONE',  ( 24.79687500061451999, 6.054752690667223547, 3.707466751127219781E-16 ) ) ;
#54514 = ORIENTED_EDGE ( 'NONE', *, *, #55072, .F. ) ;
#54515 = DIRECTION ( 'NONE',  ( 0.000000000000000000, 1.000000000000000000, -8.673617379884036705E-17 ) ) ;
#54516 = CARTESIAN_POINT ( 'NONE',  ( 11.72812500061451857, 4.541064518000418104, 2.621784821874999949 ) ) ;
#54517 = CARTESIAN_POINT ( 'NONE',  ( 2.840625000614518392, -3.027376345333614438, 5.243569643749998122 ) ) ;
#54518 = CARTESIAN_POINT ( 'NONE',  ( 13.54687500061451466, 0.000000000000000000, 4.756430356249998326 ) ) ;
#54519 = CARTESIAN_POINT ( 'NONE',  ( 27.21562500061451928, -6.054752690667223547, -1.112240025338166033E-15 ) ) ;
#54520 = CARTESIAN_POINT ( 'NONE',  ( 16.94999999999999929, 0.000000000000000000, 4.999999999999998224 ) ) ;
#54521 = CARTESIAN_POINT ( 'NONE',  ( 27.22499999999999787, 4.330127018922191873, 2.499999999999999556 ) ) ;
#54522 = CARTESIAN_POINT ( 'NONE',  ( 3.999999999999999112, 10.77500000000000213, -30.00000000000000000 ) ) ;
#54523 = CARTESIAN_POINT ( 'NONE',  ( 7.959375000614516971, -4.541064518000417216, -2.621784821875001281 ) ) ;
#54524 = CARTESIAN_POINT ( 'NONE',  ( 16.77187500061451786, 3.027376345333611329, 5.243569643749999010 ) ) ;
#54525 = CARTESIAN_POINT ( 'NONE',  ( -1.071796769724488563, 13.90490381179670010, 34.00000000000000000 ) ) ;
#54526 = VERTEX_POINT ( 'NONE', #28689 ) ;
#54527 = CARTESIAN_POINT ( 'NONE',  ( 26.76562500061451644, -6.054752690667223547, -1.112240025338166033E-15 ) ) ;
#54528 = CARTESIAN_POINT ( 'NONE',  ( 28.47187500061451715, 3.027376345333611329, 5.243569643749999010 ) ) ;
#54530 = EDGE_CURVE ( 'NONE', #23877, #55608, #33499, .T. ) ;
#54529 = CARTESIAN_POINT ( 'NONE',  ( 3.009375000614516793, -4.541064518000417216, -2.621784821875001281 ) ) ;
#54531 = CARTESIAN_POINT ( 'NONE',  ( 14.88750000000000107, -2.886751345948125991, -5.000000000000000000 ) ) ;
#54532 = CARTESIAN_POINT ( 'NONE',  ( 10.75312500061451715, 4.541064518000418104, -2.621784821874998173 ) ) ;
#54533 = CARTESIAN_POINT ( 'NONE',  ( -1.999999999999999112, 19.40000000000000213, 26.53589838486224650 ) ) ;
#54534 = DIRECTION ( 'NONE',  ( -1.000000000000000000, -0.000000000000000000, -0.000000000000000000 ) ) ;
#54535 = CARTESIAN_POINT ( 'NONE',  ( 27.89062500061451289, 6.054752690667223547, 3.707466751127219781E-16 ) ) ;
#54536 = CARTESIAN_POINT ( 'NONE',  ( 16.35000000122903430, -2.886751345948125991, -5.000000000000000000 ) ) ;
#54537 = CARTESIAN_POINT ( 'NONE',  ( 21.33750000122903145, 6.123233995736764310E-16, -4.999999999999998224 ) ) ;
#54538 = CARTESIAN_POINT ( 'NONE',  ( 16.20937500061451786, 4.119189519843966529, -2.378215178124998275 ) ) ;
#54539 = CARTESIAN_POINT ( 'NONE',  ( 4.603125000614518569, 0.000000000000000000, 5.243569643749999010 ) ) ;
#54540 = CARTESIAN_POINT ( 'NONE',  ( 20.93437500061451573, -4.541064518000419881, 2.621784821874995952 ) ) ;
#54541 = CARTESIAN_POINT ( 'NONE',  ( -3.000416591977282496E-16, 16.59687500061452070, 25.09994784771203058 ) ) ;
#54542 = CARTESIAN_POINT ( 'NONE',  ( 24.49687500061451573, -3.027376345333614438, 5.243569643749998122 ) ) ;
#54543 = CARTESIAN_POINT ( 'NONE',  ( 4.312500000000000000, 2.886751345948126879, 4.999999999999999112 ) ) ;
#54544 = CARTESIAN_POINT ( 'NONE',  ( -3.999999999999997335, 11.15000000122903323, 32.30940107675850470 ) ) ;
#54545 = CARTESIAN_POINT ( 'NONE',  ( 11.95312500061451644, -4.541064518000417216, -2.621784821875001281 ) ) ;
#54546 = CARTESIAN_POINT ( 'NONE',  ( 4.350000001229033408, 5.773502691896255534, 3.535250795749688894E-16 ) ) ;
#54547 = CARTESIAN_POINT ( 'NONE',  ( 10.17187500061451999, -6.054752690667223547, -1.112240025338166033E-15 ) ) ;
#54548 = CARTESIAN_POINT ( 'NONE',  ( 13.01249999999999929, -5.773502691896255534, -1.060575238724906372E-15 ) ) ;
#54549 = CARTESIAN_POINT ( 'NONE',  ( 9.178125000614517859, -4.541064518000419881, 2.621784821874995952 ) ) ;
#54550 = CARTESIAN_POINT ( 'NONE',  ( 14.25937500061451679, -4.541064518000417216, -2.621784821875001281 ) ) ;
#54551 = CARTESIAN_POINT ( 'NONE',  ( 3.479729569495786379, -3.590471016896914946, -3.821457900550485398 ) ) ;
#54552 = CARTESIAN_POINT ( 'NONE',  ( 21.78750000122903074, 6.123233995736764310E-16, -4.999999999999998224 ) ) ;
#54553 = CARTESIAN_POINT ( 'NONE',  ( 10.88437500061451679, 4.541064518000418104, 2.621784821874999949 ) ) ;
#54554 = CARTESIAN_POINT ( 'NONE',  ( 11.42812500061451608, -4.541064518000419881, 2.621784821874995952 ) ) ;
#54555 = CARTESIAN_POINT ( 'NONE',  ( 27.80625000122903145, 0.000000000000000000, 4.999999999999998224 ) ) ;
#54556 = CARTESIAN_POINT ( 'NONE',  ( 21.60937500061451644, 4.541064518000418104, -2.621784821874998173 ) ) ;
#54557 = CARTESIAN_POINT ( 'NONE',  ( 26.83125000122903003, 4.330127018922191873, 2.499999999999999556 ) ) ;
#54558 = DIRECTION ( 'NONE',  ( 0.1736433700863484753, 0.000000000000000000, 0.9848086007062769598 ) ) ;
#54559 = CARTESIAN_POINT ( 'NONE',  ( -1.071796769724490561, 19.90759618943233278, -34.00000000000000000 ) ) ;
#54560 = CARTESIAN_POINT ( 'NONE',  ( -3.000416591977282496E-16, 11.64687500061451786, -34.90005215228797653 ) ) ;
#54561 = CARTESIAN_POINT ( 'NONE',  ( 16.16250000122903430, 0.000000000000000000, 4.999999999999998224 ) ) ;
#54562 = CARTESIAN_POINT ( 'NONE',  ( 9.046875000614518214, 6.054752690667223547, 3.707466751127219781E-16 ) ) ;
#54563 = CARTESIAN_POINT ( 'NONE',  ( -3.000416591977282496E-16, 18.79062500061451857, -34.90005215228797653 ) ) ;
#54564 = CARTESIAN_POINT ( 'NONE',  ( 16.65000000122903501, -2.886751345948129988, 4.999999999999997335 ) ) ;
#54565 = CARTESIAN_POINT ( 'NONE',  ( 10.79062500061451679, 6.054752690667223547, 3.707466751127219781E-16 ) ) ;
#54566 = ORIENTED_EDGE ( 'NONE', *, *, #53564, .F. ) ;
#54567 = CARTESIAN_POINT ( 'NONE',  ( 15.18750000000000000, -2.886751345948129988, 4.999999999999997335 ) ) ;
#54568 = CARTESIAN_POINT ( 'NONE',  ( 29.21249999999999858, -5.773502691896255534, -1.060575238724906372E-15 ) ) ;
#54569 = CARTESIAN_POINT ( 'NONE',  ( 9.571875000614518569, 3.027376345333611329, 5.243569643749999010 ) ) ;
#54570 = CARTESIAN_POINT ( 'NONE',  ( 1.999999999999997335, 16.86874999877096570, 33.46410161513775705 ) ) ;
#54571 = CARTESIAN_POINT ( 'NONE',  ( 9.375000001229036428, 2.886751345948126879, 4.999999999999999112 ) ) ;
#54572 = CARTESIAN_POINT ( 'NONE',  ( 18.48750000122903359, -4.330127018922194537, 2.499999999999995559 ) ) ;
#54573 = CARTESIAN_POINT ( 'NONE',  ( 14.35312500061451679, 4.541064518000418104, -2.621784821874998173 ) ) ;
#54574 = CARTESIAN_POINT ( 'NONE',  ( 17.09062500061451573, 6.054752690667223547, 3.707466751127219781E-16 ) ) ;
#54575 = CARTESIAN_POINT ( 'NONE',  ( 28.27500000122903145, 2.886751345948126879, 4.999999999999999112 ) ) ;
#54576 = CARTESIAN_POINT ( 'NONE',  ( 29.62500000122903288, 2.886751345948126879, 4.999999999999999112 ) ) ;
#54577 = CARTESIAN_POINT ( 'NONE',  ( 25.38749999999999929, 5.773502691896255534, 3.535250795749688894E-16 ) ) ;
#54578 = CARTESIAN_POINT ( 'NONE',  ( 1.878215178125000495, 14.51562499938548356, 26.74683588394047007 ) ) ;
#54579 = CARTESIAN_POINT ( 'NONE',  ( 26.73749999999999716, 5.773502691896255534, 3.535250795749688894E-16 ) ) ;
#54580 = CARTESIAN_POINT ( 'NONE',  ( 25.65937500061451715, 4.541064518000418104, -2.621784821874998173 ) ) ;
#54581 = CARTESIAN_POINT ( 'NONE',  ( 26.56875000122903074, -5.773502691896255534, -1.060575238724906372E-15 ) ) ;
#54582 = CARTESIAN_POINT ( 'NONE',  ( 13.35000000122903430, 5.773502691896255534, 3.535250795749688894E-16 ) ) ;
#54583 = CARTESIAN_POINT ( 'NONE',  ( 3.412500000000002309, 2.886751345948126879, 4.999999999999999112 ) ) ;
#54584 = EDGE_CURVE ( 'NONE', #11143, #61146, #10626, .T. ) ;
#54585 = LINE ( 'NONE', #37953, #40835 ) ;
#54586 = CARTESIAN_POINT ( 'NONE',  ( 6.609375000614519102, -4.541064518000417216, -2.621784821875001281 ) ) ;
#54587 = AXIS2_PLACEMENT_3D ( 'NONE', #20900, #37898, #10918 ) ;
#54588 = CARTESIAN_POINT ( 'NONE',  ( 24.89062500061451644, -3.027376345333614438, 5.243569643749998122 ) ) ;
#54589 = CARTESIAN_POINT ( 'NONE',  ( 4.734375000614518214, -4.541064518000419881, 2.621784821874995952 ) ) ;
#54590 = CARTESIAN_POINT ( 'NONE',  ( 12.90000000000000213, 0.000000000000000000, 4.999999999999998224 ) ) ;
#54591 = CARTESIAN_POINT ( 'NONE',  ( -1.071796769724502107, 16.68259618943233491, 26.00000000000000711 ) ) ;
#54592 = CARTESIAN_POINT ( 'NONE',  ( 4.171875000614517326, 3.027376345333611329, 5.243569643749999010 ) ) ;
#54593 = CARTESIAN_POINT ( 'NONE',  ( 10.02187500061451964, 3.027376345333611329, 5.243569643749999010 ) ) ;
#54594 = CARTESIAN_POINT ( 'NONE',  ( 5.100000000000000533, 4.330127018922192761, -2.499999999999997780 ) ) ;
#54595 = CARTESIAN_POINT ( 'NONE',  ( -4.243569643749998122, 13.54062500061459140, 32.45002607614398471 ) ) ;
#54596 = CARTESIAN_POINT ( 'NONE',  ( 22.72499999999999787, 4.330127018922191873, 2.499999999999999556 ) ) ;
#54597 = CARTESIAN_POINT ( 'NONE',  ( 28.72500000000000142, -4.330127018922194537, 2.499999999999995559 ) ) ;
#54598 = CARTESIAN_POINT ( 'NONE',  ( 5.062500000000000888, 2.886751345948129099, -4.999999999999998224 ) ) ;
#54599 = ORIENTED_EDGE ( 'NONE', *, *, #34645, .F. ) ;
#54600 = CARTESIAN_POINT ( 'NONE',  ( 18.14062500061451644, -3.027376345333614438, 5.243569643749998122 ) ) ;
#54601 = CARTESIAN_POINT ( 'NONE',  ( 11.72812500061451857, 4.541064518000418104, 2.621784821874999949 ) ) ;
#54602 = CARTESIAN_POINT ( 'NONE',  ( 22.17187500061451644, -4.119189519843968306, 2.378215178124996054 ) ) ;
#54603 = CARTESIAN_POINT ( 'NONE',  ( 8.221875000614518925, 3.027376345333611329, 5.243569643749999010 ) ) ;
#54604 = CARTESIAN_POINT ( 'NONE',  ( 24.82499999999999929, 6.123233995736764310E-16, -4.999999999999998224 ) ) ;
#54605 = CARTESIAN_POINT ( 'NONE',  ( 20.81250000122903643, -4.330127018922190985, -2.500000000000001332 ) ) ;
#54606 = CARTESIAN_POINT ( 'NONE',  ( 1.071796769724505438, 10.97990381179670116, 26.00000000000001421 ) ) ;
#54607 = CARTESIAN_POINT ( 'NONE',  ( 8.784375000614518925, -4.541064518000419881, 2.621784821874995952 ) ) ;
#54608 = CARTESIAN_POINT ( 'NONE',  ( 13.32187500061451502, -6.054752690667223547, -1.112240025338166033E-15 ) ) ;
#54609 = CARTESIAN_POINT ( 'NONE',  ( 25.24687500061451573, 6.054752690667223547, 3.707466751127219781E-16 ) ) ;
#54610 = CARTESIAN_POINT ( 'NONE',  ( 13.16249999999999964, 2.886751345948129099, -4.999999999999998224 ) ) ;
#54611 = CARTESIAN_POINT ( 'NONE',  ( 17.97187500061451715, 3.027376345333613106, -5.243569643749998122 ) ) ;
#54612 = CARTESIAN_POINT ( 'NONE',  ( 8.971875000614515372, 3.027376345333613106, -5.243569643749998122 ) ) ;
#54613 = CARTESIAN_POINT ( 'NONE',  ( 3.756430356250000546, 19.99062499938548143, 27.83122392262697886 ) ) ;
#54614 = CARTESIAN_POINT ( 'NONE',  ( 22.05000000000000071, -4.330127018922190985, -2.500000000000001332 ) ) ;
#54615 = CARTESIAN_POINT ( 'NONE',  ( 2.828200636599751609E-16, 13.96250000000000213, 25.38119784648299415 ) ) ;
#54616 = CARTESIAN_POINT ( 'NONE',  ( -4.243569643749997233, 10.44687500061451857, -27.54997392385601174 ) ) ;
#54617 = CARTESIAN_POINT ( 'NONE',  ( 24.08437500061451786, -4.119189519843968306, 2.378215178124996054 ) ) ;
#54618 = CARTESIAN_POINT ( 'NONE',  ( 11.87812500061451537, -4.541064518000419881, 2.621784821874995952 ) ) ;
#54619 = CARTESIAN_POINT ( 'NONE',  ( 28.77187500061451431, 3.027376345333613106, -5.243569643749998122 ) ) ;
#54620 = DIRECTION ( 'NONE',  ( -0.000000000000000000, -1.000000000000000000, -0.000000000000000000 ) ) ;
#54621 = CARTESIAN_POINT ( 'NONE',  ( 3.999999999999999112, 9.987500001229033586, -30.00000000000000000 ) ) ;
#54622 = CARTESIAN_POINT ( 'NONE',  ( 12.71250000000000036, 2.886751345948129099, -4.999999999999998224 ) ) ;
#54623 = CARTESIAN_POINT ( 'NONE',  ( 8.484601909799253346E-16, 17.52500000122903501, 34.61880215351700230 ) ) ;
#54624 = CARTESIAN_POINT ( 'NONE',  ( 11.70000000122903216, -2.886751345948129988, 4.999999999999997335 ) ) ;
#54625 = CARTESIAN_POINT ( 'NONE',  ( 21.30937500061451573, 0.000000000000000000, 5.243569643749999010 ) ) ;
#54626 = CARTESIAN_POINT ( 'NONE',  ( 15.79687500061451821, 6.054752690667223547, 3.707466751127219781E-16 ) ) ;
#54627 = CARTESIAN_POINT ( 'NONE',  ( -4.999999999999996447, -2.928932188134524051, -4.999999999999996447 ) ) ;
#54628 = ORIENTED_EDGE ( 'NONE', *, *, #59386, .F. ) ;
#54629 = CARTESIAN_POINT ( 'NONE',  ( 16.60312500061451857, 4.541064518000418104, -2.621784821874998173 ) ) ;
#54630 = CARTESIAN_POINT ( 'NONE',  ( 28.68750000122903288, 4.330127018922191873, 2.499999999999999556 ) ) ;
#54631 = CARTESIAN_POINT ( 'NONE',  ( 18.30937500061451928, -4.541064518000417216, -2.621784821875001281 ) ) ;
#54632 = CARTESIAN_POINT ( 'NONE',  ( 5.915625000614515905, 3.027376345333611329, 5.243569643749999010 ) ) ;
#54633 = CARTESIAN_POINT ( 'NONE',  ( 20.42812500061451431, -4.541064518000419881, 2.621784821874995952 ) ) ;
#54634 = CARTESIAN_POINT ( 'NONE',  ( -4.000000000000000888, 15.46250000000000036, 32.30940107675850470 ) ) ;
#54635 = EDGE_CURVE ( 'NONE', #6912, #48096, #11057, .T. ) ;
#54636 = CARTESIAN_POINT ( 'NONE',  ( 28.80937500061451573, 4.541064518000418104, -2.621784821874998173 ) ) ;
#54637 = CARTESIAN_POINT ( 'NONE',  ( -3.000416591977282496E-16, 12.04062500061451857, 25.09994784771203058 ) ) ;
#54638 = CARTESIAN_POINT ( 'NONE',  ( 16.20000000122903216, -2.886751345948129988, 4.999999999999997335 ) ) ;
#54639 = CARTESIAN_POINT ( 'NONE',  ( 10.62187500061451750, -5.492252693125287522, -1.008910452111647106E-15 ) ) ;
#54640 = CARTESIAN_POINT ( 'NONE',  ( 27.66562500061451146, -6.054752690667223547, -1.112240025338166033E-15 ) ) ;
#54641 = CARTESIAN_POINT ( 'NONE',  ( 2.000000000000000444, 18.81874999877096499, 26.53589838486224650 ) ) ;
#54642 =( BOUNDED_CURVE ( )  B_SPLINE_CURVE ( 2, ( #69541, #13008, #21013, #43201, #26571, #63259, #65721, #48741, #18900 ),
 .UNSPECIFIED., .F., .F. ) 
 B_SPLINE_CURVE_WITH_KNOTS ( ( 3, 2, 2, 2, 3 ),
 ( 0.9456521739130434590, 0.9492753623188405765, 0.9565217391304348116, 0.9637681159420289356, 0.9662083003288912675 ),
 .UNSPECIFIED. ) 
 CURVE ( )  GEOMETRIC_REPRESENTATION_ITEM ( )  RATIONAL_B_SPLINE_CURVE ( ( 0.9330127018922194093, 0.9330127018922194093, 1.000000000000000000, 0.8660254037844387076, 1.000000000000000000, 0.8660254037844387076, 1.000000000000000000, 0.9548846649268474263, 0.9401540970596797830 ) ) 
 REPRESENTATION_ITEM ( '' )  );
#54643 = CARTESIAN_POINT ( 'NONE',  ( 21.75937500061451502, 0.000000000000000000, 5.243569643749999010 ) ) ;
#54644 = CARTESIAN_POINT ( 'NONE',  ( 22.05000000122903714, -2.886751345948129988, 4.999999999999997335 ) ) ;
#54645 = CARTESIAN_POINT ( 'NONE',  ( 23.80312500061451786, 4.541064518000418104, -2.621784821874998173 ) ) ;
#54646 = CARTESIAN_POINT ( 'NONE',  ( 16.92187500061451999, -6.054752690667223547, -1.112240025338166033E-15 ) ) ;
#54647 = CARTESIAN_POINT ( 'NONE',  ( 11.80312500061451608, 0.000000000000000000, 5.243569643749999010 ) ) ;
#54648 = CARTESIAN_POINT ( 'NONE',  ( 4.243569643749999898, 14.23437500061451821, 30.00000000000000000 ) ) ;
#54649 = CARTESIAN_POINT ( 'NONE',  ( 16.86562500061451786, -6.054752690667223547, -1.112240025338166033E-15 ) ) ;
#54650 = CARTESIAN_POINT ( 'NONE',  ( 23.38125000122903074, -4.330127018922194537, 2.499999999999995559 ) ) ;
#54651 = ORIENTED_EDGE ( 'NONE', *, *, #13863, .F. ) ;
#54652 = ORIENTED_EDGE ( 'NONE', *, *, #6970, .F. ) ;
#54653 = CARTESIAN_POINT ( 'NONE',  ( 23.51249999999999574, 2.886751345948129099, -4.999999999999998224 ) ) ;
#54654 = CARTESIAN_POINT ( 'NONE',  ( -4.243569643749999898, 18.47187500061451715, -32.45002607614398471 ) ) ;
#54655 = CARTESIAN_POINT ( 'NONE',  ( 3.764462467596158657, -3.290797220303479875, -3.829620922746740153 ) ) ;
#54656 = CARTESIAN_POINT ( 'NONE',  ( 23.65312500061451573, -4.541064518000417216, -2.621784821875001281 ) ) ;
#54657 = CARTESIAN_POINT ( 'NONE',  ( 5.353125000614515905, 4.541064518000418104, -2.621784821874998173 ) ) ;
#54658 = CARTESIAN_POINT ( 'NONE',  ( 18.18750000122903288, 6.123233995736764310E-16, -4.999999999999998224 ) ) ;
#54659 = CARTESIAN_POINT ( 'NONE',  ( 23.39062500061451289, 6.054752690667223547, 3.707466751127219781E-16 ) ) ;
#54660 = CARTESIAN_POINT ( 'NONE',  ( 22.05000000000000071, -4.330127018922190985, -2.500000000000001332 ) ) ;
#54661 = CARTESIAN_POINT ( 'NONE',  ( 28.79062500061451502, 6.054752690667223547, 3.707466751127219781E-16 ) ) ;
#54662 = CARTESIAN_POINT ( 'NONE',  ( 7.828125000614517326, -4.541064518000419881, 2.621784821874995952 ) ) ;
#54663 = ORIENTED_EDGE ( 'NONE', *, *, #8736, .F. ) ;
#54664 = CARTESIAN_POINT ( 'NONE',  ( 23.80312500061451786, 4.541064518000418104, -2.621784821874998173 ) ) ;
#54665 = CARTESIAN_POINT ( 'NONE',  ( 4.753125000614515372, -4.541064518000417216, -2.621784821875001281 ) ) ;
#54666 = CARTESIAN_POINT ( 'NONE',  ( 12.60937500061451821, 4.119189519843966529, -2.378215178124998275 ) ) ;
#54667 = CARTESIAN_POINT ( 'NONE',  ( 2.915625000614516793, -6.054752690667223547, -1.112240025338166033E-15 ) ) ;
#54668 = CARTESIAN_POINT ( 'NONE',  ( -3.999999999999997335, 12.95000000122903572, -27.69059892324149175 ) ) ;
#54669 = CARTESIAN_POINT ( 'NONE',  ( 1.071796769724490783, 12.98615380933863328, 26.00000000000000000 ) ) ;
#54670 = EDGE_CURVE ( 'NONE', #54755, #23337, #63907, .T. ) ;
#54671 = CARTESIAN_POINT ( 'NONE',  ( 11.66249999999999964, -5.773502691896255534, -1.060575238724906372E-15 ) ) ;
#54672 = CARTESIAN_POINT ( 'NONE',  ( 10.88437500061451679, 4.541064518000418104, 2.621784821874999949 ) ) ;
#54673 = CARTESIAN_POINT ( 'NONE',  ( 5.512500001229033941, -4.330127018922190985, -2.500000000000001332 ) ) ;
#54674 = CARTESIAN_POINT ( 'NONE',  ( 14.59687500061452070, -3.027376345333614438, 5.243569643749998122 ) ) ;
#54675 = CARTESIAN_POINT ( 'NONE',  ( 5.371875000614516615, 3.027376345333613106, -5.243569643749998122 ) ) ;
#54676 = CARTESIAN_POINT ( 'NONE',  ( 4.243569643749999898, 10.09062500061451928, -27.54997392385601529 ) ) ;
#54677 = CARTESIAN_POINT ( 'NONE',  ( 14.24999999999999822, 0.000000000000000000, 4.999999999999998224 ) ) ;
#54678 = CARTESIAN_POINT ( 'NONE',  ( 13.50937500061451679, 4.541064518000418104, -2.621784821874998173 ) ) ;
#54679 = CARTESIAN_POINT ( 'NONE',  ( 3.662614727433532558, 3.403720994510690101, 3.988704636966998063 ) ) ;
#54680 = CARTESIAN_POINT ( 'NONE',  ( 22.67812500061451431, -4.541064518000419881, 2.621784821874995952 ) ) ;
#54681 = DIRECTION ( 'NONE',  ( -1.000000000000000000, -0.000000000000000000, -0.000000000000000000 ) ) ;
#54682 =( BOUNDED_CURVE ( )  B_SPLINE_CURVE ( 2, ( #32977, #49976, #20047, #65128, #8989, #31521, #457 ),
 .UNSPECIFIED., .F., .F. ) 
 B_SPLINE_CURVE_WITH_KNOTS ( ( 3, 2, 2, 3 ),
 ( 0.5499999999999999334, 0.5533333333333332327, 0.5566666666666666430, 0.5600000000000000533 ),
 .UNSPECIFIED. ) 
 CURVE ( )  GEOMETRIC_REPRESENTATION_ITEM ( )  RATIONAL_B_SPLINE_CURVE ( ( 1.000000000000004441, 0.8660254037844342667, 1.000000000000000000, 0.8660254037844387076, 1.000000000000000000, 0.8660254037844387076, 1.000000000000000000 ) ) 
 REPRESENTATION_ITEM ( '' )  );
#54683 = CARTESIAN_POINT ( 'NONE',  ( -3.000416591977282496E-16, 19.69062500061459176, 25.09994784771203058 ) ) ;
#54684 = CARTESIAN_POINT ( 'NONE',  ( 23.10937500061451644, 0.000000000000000000, 5.243569643749999010 ) ) ;
#54685 = CARTESIAN_POINT ( 'NONE',  ( 29.77499999999999858, 6.123233995736764310E-16, -4.999999999999998224 ) ) ;
#54686 =( BOUNDED_CURVE ( )  B_SPLINE_CURVE ( 2, ( #51979, #23888, #46435, #68974, #18331, #63417, #52336 ),
 .UNSPECIFIED., .F., .F. ) 
 B_SPLINE_CURVE_WITH_KNOTS ( ( 3, 2, 2, 3 ),
 ( 0.7249999999999999778, 0.7277777777777777457, 0.7305555555555555136, 0.7333333333333332815 ),
 .UNSPECIFIED. ) 
 CURVE ( )  GEOMETRIC_REPRESENTATION_ITEM ( )  RATIONAL_B_SPLINE_CURVE ( ( 1.000000000000000000, 0.8660254037844387076, 1.000000000000000000, 0.8660254037844387076, 1.000000000000000000, 0.8660254037844387076, 1.000000000000000000 ) ) 
 REPRESENTATION_ITEM ( '' )  );
#54687 = CARTESIAN_POINT ( 'NONE',  ( 5.240625000614516971, -3.027376345333610441, -5.243569643749999898 ) ) ;
#54688 = CARTESIAN_POINT ( 'NONE',  ( 19.95937500061451786, -5.492252693125287522, -1.008910452111647106E-15 ) ) ;
#54689 = CARTESIAN_POINT ( 'NONE',  ( 23.95312500061451289, 0.000000000000000000, 5.243569643749999010 ) ) ;
#54690 = CARTESIAN_POINT ( 'NONE',  ( 17.69062500061451715, -3.027376345333614438, 5.243569643749998122 ) ) ;
#54691 = CARTESIAN_POINT ( 'NONE',  ( 14.93437500061451750, 4.541064518000418104, 2.621784821874999949 ) ) ;
#54692 = DIRECTION ( 'NONE',  ( 0.000000000000000000, 0.000000000000000000, -1.000000000000000000 ) ) ;
#54693 = CARTESIAN_POINT ( 'NONE',  ( 28.27500000122903145, 2.886751345948126879, 4.999999999999999112 ) ) ;
#54694 = CARTESIAN_POINT ( 'NONE',  ( 5.746875000614517504, -3.027376345333610441, -5.243569643749999898 ) ) ;
#54695 = CARTESIAN_POINT ( 'NONE',  ( 17.37187500061451573, -6.054752690667223547, -1.112240025338166033E-15 ) ) ;
#54696 = CARTESIAN_POINT ( 'NONE',  ( -1.071796769724491005, 11.80759618943233669, 26.00000000000000355 ) ) ;
#54697 = CARTESIAN_POINT ( 'NONE',  ( 23.85000000000000142, -4.330127018922190985, -2.500000000000001332 ) ) ;
#54698 = CARTESIAN_POINT ( 'NONE',  ( 4.012500001229033053, 0.000000000000000000, 4.999999999999998224 ) ) ;
#54699 = CARTESIAN_POINT ( 'NONE',  ( 25.32187500061451857, 3.027376345333611329, 5.243569643749999010 ) ) ;
#54700 = CARTESIAN_POINT ( 'NONE',  ( 16.20937500061451786, 4.541064518000418104, -2.621784821874998173 ) ) ;
#54701 = CARTESIAN_POINT ( 'NONE',  ( 1.071796769724485232, 15.74240381056766402, 25.99999999999999645 ) ) ;
#54702 = CARTESIAN_POINT ( 'NONE',  ( 29.51249999999999929, 2.886751345948126879, 4.999999999999999112 ) ) ;
#54703 = CARTESIAN_POINT ( 'NONE',  ( 8.699999999999999289, 4.330127018922192761, -2.499999999999997780 ) ) ;
#54704 = CARTESIAN_POINT ( 'NONE',  ( 9.159375000614517148, -5.492252693125287522, -1.008910452111647106E-15 ) ) ;
#54705 = CARTESIAN_POINT ( 'NONE',  ( 20.39062500061451644, -3.027376345333614438, 5.243569643749998122 ) ) ;
#54706 = CARTESIAN_POINT ( 'NONE',  ( 10.01250000000000107, 2.886751345948129099, -4.999999999999998224 ) ) ;
#54707 = CARTESIAN_POINT ( 'NONE',  ( 5.090625000614516615, -3.027376345333614438, 5.243569643749998122 ) ) ;
#54708 = CARTESIAN_POINT ( 'NONE',  ( 18.41250000000000142, -5.773502691896255534, -1.060575238724906372E-15 ) ) ;
#54709 =( BOUNDED_CURVE ( )  B_SPLINE_CURVE ( 2, ( #65790, #60230, #9644, #29181, #72798, #17708, #67982 ),
 .UNSPECIFIED., .F., .F. ) 
 B_SPLINE_CURVE_WITH_KNOTS ( ( 3, 2, 2, 3 ),
 ( 0.6800000000000001599, 0.6833333333333334592, 0.6866666666666667584, 0.6900000000000000577 ),
 .UNSPECIFIED. ) 
 CURVE ( )  GEOMETRIC_REPRESENTATION_ITEM ( )  RATIONAL_B_SPLINE_CURVE ( ( 0.9999999999999955591, 0.8660254037844431485, 1.000000000000000000, 0.8660254037844387076, 1.000000000000000000, 0.8660254037844342667, 1.000000000000004441 ) ) 
 REPRESENTATION_ITEM ( '' )  );
#54710 = CARTESIAN_POINT ( 'NONE',  ( 18.66562500061451146, -6.054752690667223547, -1.112240025338166033E-15 ) ) ;
#54711 = CARTESIAN_POINT ( 'NONE',  ( -1.999999999999997113, 17.37500000000000000, 33.46410161513775705 ) ) ;
#54712 = CARTESIAN_POINT ( 'NONE',  ( 23.43750000122902932, -4.330127018922194537, 2.499999999999995559 ) ) ;
#54713 = CYLINDRICAL_SURFACE ( 'NONE', #9983, 4.000000000000000000 ) ;
#54714 = CARTESIAN_POINT ( 'NONE',  ( 29.55937500061451573, -4.541064518000417216, -2.621784821875001281 ) ) ;
#54715 = VERTEX_POINT ( 'NONE', #72309 ) ;
#54716 = CARTESIAN_POINT ( 'NONE',  ( 17.39062500061451644, -3.027376345333610441, -5.243569643749999898 ) ) ;
#54717 = CARTESIAN_POINT ( 'NONE',  ( 23.99062500061451786, -3.027376345333614438, 5.243569643749998122 ) ) ;
#54718 = CARTESIAN_POINT ( 'NONE',  ( 25.58437500061451431, 6.421520780324663323E-16, -5.243569643749999010 ) ) ;
#54719 = CARTESIAN_POINT ( 'NONE',  ( 8.175000000000002487, 6.123233995736764310E-16, -4.999999999999998224 ) ) ;
#54720 = CARTESIAN_POINT ( 'NONE',  ( 13.11562500061451786, 3.027376345333611329, 5.243569643749999010 ) ) ;
#54721 = CARTESIAN_POINT ( 'NONE',  ( 27.17812500061451786, -4.541064518000419881, 2.621784821874995952 ) ) ;
#54722 = CARTESIAN_POINT ( 'NONE',  ( 14.29687500061451821, -3.027376345333610441, -5.243569643749999898 ) ) ;
#54723 = CARTESIAN_POINT ( 'NONE',  ( 18.38437500061451857, 6.421520780324663323E-16, -5.243569643749999010 ) ) ;
#54724 = DIRECTION ( 'NONE',  ( 1.000000000000000000, -0.000000000000000000, -0.000000000000000000 ) ) ;
#54725 = CARTESIAN_POINT ( 'NONE',  ( 4.243569643749999898, 19.09062500061451573, 32.45002607614398471 ) ) ;
#54726 = CARTESIAN_POINT ( 'NONE',  ( 22.80000000122903359, 5.773502691896255534, 3.535250795749688894E-16 ) ) ;
#54727 = CARTESIAN_POINT ( 'NONE',  ( 15.94687500061451502, -2.746126346562646425, 4.756430356249996549 ) ) ;
#54728 = CARTESIAN_POINT ( 'NONE',  ( 15.25312500061451715, 4.541064518000418104, -2.621784821874998173 ) ) ;
#54729 = CARTESIAN_POINT ( 'NONE',  ( 7.209375000614519635, 4.541064518000418104, -2.621784821874998173 ) ) ;
#54730 = CARTESIAN_POINT ( 'NONE',  ( 8.184375000614515727, 4.541064518000418104, 2.621784821874999949 ) ) ;
#54731 = ORIENTED_EDGE ( 'NONE', *, *, #49427, .T. ) ;
#54732 = EDGE_CURVE ( 'NONE', #36300, #29715, #276, .T. ) ;
#54733 = CARTESIAN_POINT ( 'NONE',  ( 27.68437500061451573, -4.541064518000419881, 2.621784821874995952 ) ) ;
#54734 = CARTESIAN_POINT ( 'NONE',  ( 20.20312500061451644, 4.541064518000418104, -2.621784821874998173 ) ) ;
#54735 = CARTESIAN_POINT ( 'NONE',  ( 23.67187500061451999, -6.054752690667223547, -1.112240025338166033E-15 ) ) ;
#54736 = CARTESIAN_POINT ( 'NONE',  ( 19.60312500061451502, -4.541064518000417216, -2.621784821875001281 ) ) ;
#54737 = CARTESIAN_POINT ( 'NONE',  ( 1.999999999999998668, 11.30000000000000071, 26.53589838486224650 ) ) ;
#54738 = CARTESIAN_POINT ( 'NONE',  ( 26.20312500061451644, 0.000000000000000000, 5.243569643749999010 ) ) ;
#54739 = CARTESIAN_POINT ( 'NONE',  ( 6.375000001229031987, -5.773502691896255534, -1.060575238724906372E-15 ) ) ;
#54740 = ORIENTED_EDGE ( 'NONE', *, *, #34570, .F. ) ;
#54741 = CARTESIAN_POINT ( 'NONE',  ( 29.21249999999999858, -5.773502691896255534, -1.060575238724906372E-15 ) ) ;
#54742 = CARTESIAN_POINT ( 'NONE',  ( 8.484601909799253346E-16, 16.06250000000000000, -25.38119784648299770 ) ) ;
#54743 = CARTESIAN_POINT ( 'NONE',  ( 23.40000000122903145, -2.886751345948129988, 4.999999999999997335 ) ) ;
#54744 = CARTESIAN_POINT ( 'NONE',  ( 3.756430356250000546, 14.14062499938548356, 27.83122392262697886 ) ) ;
#54745 = CARTESIAN_POINT ( 'NONE',  ( 5.634375000614519458, -4.541064518000419881, 2.621784821874995952 ) ) ;
#54746 = CARTESIAN_POINT ( 'NONE',  ( 12.67499999999999893, 6.123233995736764310E-16, -4.999999999999998224 ) ) ;
#54747 = CARTESIAN_POINT ( 'NONE',  ( 13.34062500061451750, -3.027376345333610441, -5.243569643749999898 ) ) ;
#54748 = CARTESIAN_POINT ( 'NONE',  ( 9.084375000614517859, 4.541064518000418104, 2.621784821874999949 ) ) ;
#54749 = CARTESIAN_POINT ( 'NONE',  ( 25.61250000122903359, 0.000000000000000000, 4.999999999999998224 ) ) ;
#54750 = CARTESIAN_POINT ( 'NONE',  ( 14.03437500061451715, 4.541064518000418104, 2.621784821874999949 ) ) ;
#54751 = CARTESIAN_POINT ( 'NONE',  ( 6.084375000614518747, -4.541064518000419881, 2.621784821874995952 ) ) ;
#54752 = CARTESIAN_POINT ( 'NONE',  ( 29.96250000000000213, 2.886751345948126879, 4.999999999999999112 ) ) ;
#54753 = CARTESIAN_POINT ( 'NONE',  ( 6.103125000614515905, -4.541064518000417216, -2.621784821875001281 ) ) ;
#54754 = CARTESIAN_POINT ( 'NONE',  ( 14.39062500061451821, 6.054752690667223547, 3.707466751127219781E-16 ) ) ;
#54755 = VERTEX_POINT ( 'NONE', #22419 ) ;
#54756 = CARTESIAN_POINT ( 'NONE',  ( 11.31562500061451892, 3.027376345333611329, 5.243569643749999010 ) ) ;
#54757 = CARTESIAN_POINT ( 'NONE',  ( 9.440625000614517148, 6.054752690667223547, 3.707466751127219781E-16 ) ) ;
#54758 = CARTESIAN_POINT ( 'NONE',  ( 20.63437500061451857, 5.824947211148865298E-16, -4.756430356249998326 ) ) ;
#54759 = CARTESIAN_POINT ( 'NONE',  ( 8.587500000000002132, -2.886751345948125991, -5.000000000000000000 ) ) ;
#54760 = CARTESIAN_POINT ( 'NONE',  ( 3.262500001229035718, -4.330127018922190985, -2.500000000000001332 ) ) ;
#54761 = CARTESIAN_POINT ( 'NONE',  ( 16.76249999999999929, 2.886751345948129099, -4.999999999999998224 ) ) ;
#54762 = EDGE_CURVE ( 'NONE', #69714, #32715, #16150, .T. ) ;
#54763 = CARTESIAN_POINT ( 'NONE',  ( 19.05937500061451928, 0.000000000000000000, 5.243569643749999010 ) ) ;
#54764 = CARTESIAN_POINT ( 'NONE',  ( 14.17500000122903536, 2.886751345948129099, -4.999999999999998224 ) ) ;
#54765 = CARTESIAN_POINT ( 'NONE',  ( 22.42500000000000071, -4.330127018922194537, 2.499999999999995559 ) ) ;
#54766 = CARTESIAN_POINT ( 'NONE',  ( -4.243569643749999898, 16.61562500061451786, -32.45002607614398471 ) ) ;
#54767 = CARTESIAN_POINT ( 'NONE',  ( 22.05000000000000071, -4.330127018922190985, -2.500000000000001332 ) ) ;
#54768 = CARTESIAN_POINT ( 'NONE',  ( 29.76562500061451644, 3.027376345333611329, 5.243569643749999010 ) ) ;
#54769 = CARTESIAN_POINT ( 'NONE',  ( 28.35000000000000142, -4.330127018922190985, -2.500000000000001332 ) ) ;
#54770 = CARTESIAN_POINT ( 'NONE',  ( 24.18750000000000000, -2.886751345948096681, 5.000000000000054179 ) ) ;
#54771 = CARTESIAN_POINT ( 'NONE',  ( 14.59687500061452070, -3.027376345333614438, 5.243569643749998122 ) ) ;
#54772 = CARTESIAN_POINT ( 'NONE',  ( 25.76249999999999929, 2.886751345948129099, -4.999999999999998224 ) ) ;
#54773 = CARTESIAN_POINT ( 'NONE',  ( 10.67812500061451608, 6.421520780324663323E-16, -5.243569643749999010 ) ) ;
#54774 = CARTESIAN_POINT ( 'NONE',  ( 27.68437500061451573, -2.746126346562642428, -4.756430356249999214 ) ) ;
#54775 = CARTESIAN_POINT ( 'NONE',  ( 22.32187500061451502, -6.054752690667223547, -1.112240025338166033E-15 ) ) ;
#54776 = CARTESIAN_POINT ( 'NONE',  ( 14.03437500061451537, -2.746126346562646425, 4.756430356249996549 ) ) ;
#54777 = CARTESIAN_POINT ( 'NONE',  ( 8.840625000614515727, -3.027376345333610441, -5.243569643749999898 ) ) ;
#54778 = CARTESIAN_POINT ( 'NONE',  ( 13.88437500061451679, 6.421520780324663323E-16, -5.243569643749999010 ) ) ;
#54779 = EDGE_LOOP ( 'NONE', ( #3006, #60402, #57486, #65232 ) ) ;
#54780 = CARTESIAN_POINT ( 'NONE',  ( 24.23437500061451644, 6.421520780324663323E-16, -5.243569643749999010 ) ) ;
#54781 = CARTESIAN_POINT ( 'NONE',  ( 30.00000000000000000, 0.000000000000000000, 0.000000000000000000 ) ) ;
#54782 = CARTESIAN_POINT ( 'NONE',  ( 24.60000000000000142, 0.000000000000000000, 4.999999999999998224 ) ) ;
#54783 = CARTESIAN_POINT ( 'NONE',  ( 5.212500000000002132, 2.886751345948126879, 4.999999999999999112 ) ) ;
#54784 = CARTESIAN_POINT ( 'NONE',  ( 16.57500000122903216, 2.886751345948126879, 4.999999999999999112 ) ) ;
#54785 = FACE_OUTER_BOUND ( 'NONE', #14201, .T. ) ;
#54786 = CARTESIAN_POINT ( 'NONE',  ( 7.809375000614515727, -5.492252693125287522, -1.008910452111647106E-15 ) ) ;
#54787 = ORIENTED_EDGE ( 'NONE', *, *, #63337, .T. ) ;
#54788 = CARTESIAN_POINT ( 'NONE',  ( 14.32500000000000107, -4.330127018922194537, 2.499999999999995559 ) ) ;
#54789 = CARTESIAN_POINT ( 'NONE',  ( 16.68750000000000000, -2.886751345948125991, -5.000000000000000000 ) ) ;
#54790 = CARTESIAN_POINT ( 'NONE',  ( 11.12812500061451715, 6.421520780324663323E-16, -5.243569643749999010 ) ) ;
#54791 = EDGE_LOOP ( 'NONE', ( #66234, #46413, #3023, #65217 ) ) ;
#54792 = CARTESIAN_POINT ( 'NONE',  ( 18.63750000122903216, 6.123233995736764310E-16, -4.999999999999998224 ) ) ;
#54793 = CARTESIAN_POINT ( 'NONE',  ( 9.001249775931846008E-16, 16.37187500061451573, -25.09994784771203058 ) ) ;
#54794 = CARTESIAN_POINT ( 'NONE',  ( 29.51250000122903216, 4.330127018922192761, -2.499999999999997780 ) ) ;
#54795 = CARTESIAN_POINT ( 'NONE',  ( 3.756430356250000102, 15.34062499938548285, 30.00000000000000000 ) ) ;
#54796 = CARTESIAN_POINT ( 'NONE',  ( 9.487500000000000711, -2.886751345948125991, -5.000000000000000000 ) ) ;
#54797 = DIRECTION ( 'NONE',  ( -0.000000000000000000, -1.000000000000000000, -0.000000000000000000 ) ) ;
#54798 = AXIS2_PLACEMENT_3D ( 'NONE', #2417, #63385, #12770 ) ;
#54799 = VERTEX_POINT ( 'NONE', #39423 ) ;
#54800 = CARTESIAN_POINT ( 'NONE',  ( 4.243569643749999898, 12.82812500061451821, 30.00000000000000000 ) ) ;
#54801 = CARTESIAN_POINT ( 'NONE',  ( 25.41562500061451146, -6.054752690667223547, -1.112240025338166033E-15 ) ) ;
#54802 = CARTESIAN_POINT ( 'NONE',  ( 3.504965621013899746, 3.565840152826760256, 3.504965621013765631 ) ) ;
#54803 = DIRECTION ( 'NONE',  ( -1.000000000000000000, -0.000000000000000000, -0.000000000000000000 ) ) ;
#54804 = CARTESIAN_POINT ( 'NONE',  ( 20.82187500061451857, 3.027376345333611329, 5.243569643749999010 ) ) ;
#54805 = CARTESIAN_POINT ( 'NONE',  ( 19.00312500061451715, 0.000000000000000000, 5.243569643749999010 ) ) ;
#54806 = CARTESIAN_POINT ( 'NONE',  ( -4.243569643749999898, 13.50312500061459531, -30.00000000000000000 ) ) ;
#54807 = CARTESIAN_POINT ( 'NONE',  ( 22.61250000122903003, -4.330127018922190985, -2.500000000000001332 ) ) ;
#54808 = AXIS2_PLACEMENT_3D ( 'NONE', #3716, #26243, #20682 ) ;
#54809 = CARTESIAN_POINT ( 'NONE',  ( 5.128125000614516260, -4.541064518000419881, 2.621784821874995952 ) ) ;
#54810 = CARTESIAN_POINT ( 'NONE',  ( 23.33437500061451786, 5.824947211148865298E-16, -4.756430356249998326 ) ) ;
#54811 = CARTESIAN_POINT ( 'NONE',  ( 22.52812500061451573, 4.541064518000418104, 2.621784821874999949 ) ) ;
#54812 = CARTESIAN_POINT ( 'NONE',  ( 8.709375000614517859, 0.000000000000000000, 4.756430356249998326 ) ) ;
#54813 = CARTESIAN_POINT ( 'NONE',  ( -3.756430356250000102, 18.71562499938548285, 30.00000000000000000 ) ) ;
#54814 = CARTESIAN_POINT ( 'NONE',  ( 15.87187500061451573, 3.027376345333611329, 5.243569643749999010 ) ) ;
#54815 = CARTESIAN_POINT ( 'NONE',  ( 13.24687500061451750, -3.027376345333614438, 5.243569643749998122 ) ) ;
#54816 = CARTESIAN_POINT ( 'NONE',  ( 22.24687500061451217, -3.027376345333614438, 5.243569643749998122 ) ) ;
#54817 = CARTESIAN_POINT ( 'NONE',  ( -4.243569643749999898, 12.62187500061451750, 27.54997392385601529 ) ) ;
#54818 = CARTESIAN_POINT ( 'NONE',  ( 3.928125000614516527, 6.421520780324663323E-16, -5.243569643749999010 ) ) ;
#54819 = CARTESIAN_POINT ( 'NONE',  ( 25.45312500061451644, -4.541064518000417216, -2.621784821875001281 ) ) ;
#54820 = CARTESIAN_POINT ( 'NONE',  ( 26.24062500061451431, -3.027376345333614438, 5.243569643749998122 ) ) ;
#54821 = CARTESIAN_POINT ( 'NONE',  ( 17.38125000122903074, 4.330127018922191873, 2.499999999999999556 ) ) ;
#54822 = CARTESIAN_POINT ( 'NONE',  ( -2.000000000000000000, 18.57500000000000284, 26.53589838486224650 ) ) ;
#54823 = CARTESIAN_POINT ( 'NONE',  ( 6.159375000614517148, -4.541064518000417216, -2.621784821875001281 ) ) ;
#54824 = SHAPE_DEFINITION_REPRESENTATION ( #15488, #46217 ) ;
#54825 = CARTESIAN_POINT ( 'NONE',  ( 13.98750000122903359, -4.330127018922194537, 2.499999999999995559 ) ) ;
#54826 = AXIS2_PLACEMENT_3D ( 'NONE', #66122, #55410, #15501 ) ;
#54827 = CARTESIAN_POINT ( 'NONE',  ( 8.962500001229033231, 0.000000000000000000, 4.999999999999998224 ) ) ;
#54828 = CARTESIAN_POINT ( 'NONE',  ( 29.10000000122903074, 5.773502691896255534, 3.535250795749688894E-16 ) ) ;
#54829 = CARTESIAN_POINT ( 'NONE',  ( 4.000000000000000000, 16.08124999877096784, 27.69059892324149530 ) ) ;
#54830 = CARTESIAN_POINT ( 'NONE',  ( 17.45625000122903003, 0.000000000000000000, 4.999999999999998224 ) ) ;
#54831 = CARTESIAN_POINT ( 'NONE',  ( 14.52187500061451608, 3.027376345333611329, 5.243569643749999010 ) ) ;
#54832 = DIRECTION ( 'NONE',  ( -0.000000000000000000, -1.000000000000000000, -0.000000000000000000 ) ) ;
#54833 = EDGE_LOOP ( 'NONE', ( #43890, #40845, #25100, #17735 ) ) ;
#54834 = CARTESIAN_POINT ( 'NONE',  ( 19.22812500061451502, 6.421520780324663323E-16, -5.243569643749999010 ) ) ;
#54835 = CARTESIAN_POINT ( 'NONE',  ( 6.965625000614518392, -6.054752690667223547, -1.112240025338166033E-15 ) ) ;
#54836 = CARTESIAN_POINT ( 'NONE',  ( 24.79687500061452354, 6.054752690667223547, 3.707466751127219781E-16 ) ) ;
#54837 = CARTESIAN_POINT ( 'NONE',  ( 8.203125000614518214, 0.000000000000000000, 5.243569643749999010 ) ) ;
#54838 = LINE ( 'NONE', #15301, #60374 ) ;
#54839 = CARTESIAN_POINT ( 'NONE',  ( 7.087500001229034119, 4.330127018922191873, 2.499999999999999556 ) ) ;
#54840 = CARTESIAN_POINT ( 'NONE',  ( 22.22812500061451502, -4.541064518000419881, 2.621784821874995952 ) ) ;
#54841 = CARTESIAN_POINT ( 'NONE',  ( 4.000000000000000000, 18.50000000122903288, -27.69059892324149530 ) ) ;
#54842 = CARTESIAN_POINT ( 'NONE',  ( 9.712500001229033231, 4.330127018922192761, -2.499999999999997780 ) ) ;
#54843 = CARTESIAN_POINT ( 'NONE',  ( 19.37812500061451715, 4.541064518000418104, 2.621784821874999949 ) ) ;
#54844 = CARTESIAN_POINT ( 'NONE',  ( 15.21562500061451750, 3.027376345333613106, -5.243569643749998122 ) ) ;
#54845 = CARTESIAN_POINT ( 'NONE',  ( 28.73437500061451644, 5.824947211148865298E-16, -4.756430356249998326 ) ) ;
#54846 = CARTESIAN_POINT ( 'NONE',  ( 16.80000000000000071, 4.330127018922192761, -2.499999999999997780 ) ) ;
#54847 = CARTESIAN_POINT ( 'NONE',  ( 10.80000000122903536, -2.886751345948129988, 4.999999999999997335 ) ) ;
#54848 = CARTESIAN_POINT ( 'NONE',  ( 8.765625000614518214, -6.054752690667223547, -1.112240025338166033E-15 ) ) ;
#54849 = CARTESIAN_POINT ( 'NONE',  ( 10.79062500061451679, 6.054752690667223547, 3.707466751127219781E-16 ) ) ;
#54850 = EDGE_CURVE ( 'NONE', #63961, #62008, #18145, .T. ) ;
#54851 = CARTESIAN_POINT ( 'NONE',  ( 21.86250000122903003, 4.330127018922192761, -2.499999999999997780 ) ) ;
#54852 = VECTOR ( 'NONE', #17993, 1000.000000000000000 ) ;
#54853 = CARTESIAN_POINT ( 'NONE',  ( 18.83437500061451431, 6.421520780324663323E-16, -5.243569643749999010 ) ) ;
#54854 = CARTESIAN_POINT ( 'NONE',  ( 25.01249999999999929, 2.886751345948126879, 4.999999999999998224 ) ) ;
#54855 = CARTESIAN_POINT ( 'NONE',  ( 6.262500001229034829, 0.000000000000000000, 4.999999999999998224 ) ) ;
#54856 = CARTESIAN_POINT ( 'NONE',  ( 4.809375000614516615, -4.541064518000417216, -2.621784821875001281 ) ) ;
#54857 = CARTESIAN_POINT ( 'NONE',  ( 22.17187500061451644, 3.027376345333611329, 5.243569643749999010 ) ) ;
#54858 = CARTESIAN_POINT ( 'NONE',  ( 3.999999999999998668, 18.57500000122903216, 27.69059892324149530 ) ) ;
#54859 = AXIS2_PLACEMENT_3D ( 'NONE', #27721, #56862, #56155 ) ;
#54860 = CARTESIAN_POINT ( 'NONE',  ( 20.01562500061451644, -6.054752690667223547, -1.112240025338166033E-15 ) ) ;
#54861 = CARTESIAN_POINT ( 'NONE',  ( 23.10937500061451644, 0.000000000000000000, 5.243569643749999010 ) ) ;
#54862 = CARTESIAN_POINT ( 'NONE',  ( 3.756430356250000546, 19.09062499938548285, 27.83122392262697886 ) ) ;
#54863 = CARTESIAN_POINT ( 'NONE',  ( 27.97500000000000142, 6.123233995736764310E-16, -4.999999999999998224 ) ) ;
#54864 = CARTESIAN_POINT ( 'NONE',  ( 28.47187500061451715, 3.027376345333611329, 5.243569643749999010 ) ) ;
#54865 = CARTESIAN_POINT ( 'NONE',  ( 21.98437500061451644, 5.492252693125287522, 3.363034840372157021E-16 ) ) ;
#54866 = CARTESIAN_POINT ( 'NONE',  ( 13.97812500061451679, 4.541064518000418104, 2.621784821874999949 ) ) ;
#54867 = AXIS2_PLACEMENT_3D ( 'NONE', #6440, #21974, #51513 ) ;
#54868 = CARTESIAN_POINT ( 'NONE',  ( 12.34687500061452070, -3.027376345333614438, 5.243569643749998122 ) ) ;
#54869 = VERTEX_POINT ( 'NONE', #39793 ) ;
#54870 = CARTESIAN_POINT ( 'NONE',  ( 18.07499999999999929, 6.123233995736764310E-16, -4.999999999999998224 ) ) ;
#54871 = CARTESIAN_POINT ( 'NONE',  ( 23.57812500061451289, -4.541064518000419881, 2.621784821874995952 ) ) ;
#54872 = CARTESIAN_POINT ( 'NONE',  ( -1.071796769724491005, 10.57009619066136707, -34.00000000000000000 ) ) ;
#54873 = DIRECTION ( 'NONE',  ( -1.000000000000000000, -0.000000000000000000, -0.000000000000000000 ) ) ;
#54874 = CARTESIAN_POINT ( 'NONE',  ( 13.91249999999999964, -5.773502691896255534, -1.060575238724906372E-15 ) ) ;
#54875 = CARTESIAN_POINT ( 'NONE',  ( 23.25000000122903288, 5.773502691896255534, 3.535250795749688894E-16 ) ) ;
#54876 = CARTESIAN_POINT ( 'NONE',  ( 18.70312500061451644, -4.541064518000417216, -2.621784821875001281 ) ) ;
#54877 = ORIENTED_EDGE ( 'NONE', *, *, #65091, .T. ) ;
#54878 = CARTESIAN_POINT ( 'NONE',  ( 21.33749999999999858, 5.773502691896255534, 3.535250795749688894E-16 ) ) ;
#54879 = CARTESIAN_POINT ( 'NONE',  ( 23.33437500061451786, 6.421520780324663323E-16, -5.243569643749999010 ) ) ;
#54880 = VERTEX_POINT ( 'NONE', #62310 ) ;
#54881 = CARTESIAN_POINT ( 'NONE',  ( 1.071796769724488785, 19.15759618943233278, 34.00000000000000000 ) ) ;
#54882 = CARTESIAN_POINT ( 'NONE',  ( 10.41562500061451679, 3.027376345333611329, 5.243569643749999010 ) ) ;
#54883 = CARTESIAN_POINT ( 'NONE',  ( 4.190625000614518925, -3.027376345333614438, 5.243569643749998122 ) ) ;
#54884 = CARTESIAN_POINT ( 'NONE',  ( 13.77187500061451431, 5.824947211148865298E-16, -4.756430356249998326 ) ) ;
#54885 = CARTESIAN_POINT ( 'NONE',  ( 26.39062500061451644, -3.027376345333610441, -5.243569643749999898 ) ) ;
#54886 = CARTESIAN_POINT ( 'NONE',  ( 16.23750000000000071, -2.886751345948125991, -5.000000000000000000 ) ) ;
#54887 = CARTESIAN_POINT ( 'NONE',  ( 24.93750000000000355, 5.773502691896255534, 3.535250795749688894E-16 ) ) ;
#54888 = CARTESIAN_POINT ( 'NONE',  ( 7.725000001229034297, -5.773502691896255534, -1.060575238724906372E-15 ) ) ;
#54889 = CARTESIAN_POINT ( 'NONE',  ( 6.909375000614518036, 0.000000000000000000, 5.243569643749999010 ) ) ;
#54890 = CARTESIAN_POINT ( 'NONE',  ( 17.37187500061451573, -6.054752690667223547, -1.112240025338166033E-15 ) ) ;
#54891 = CARTESIAN_POINT ( 'NONE',  ( 28.02187500061451431, 3.027376345333611329, 5.243569643749999010 ) ) ;
#54892 = VERTEX_POINT ( 'NONE', #11706 ) ;
#54893 = CARTESIAN_POINT ( 'NONE',  ( 26.72812500061451502, -4.541064518000419881, 2.621784821874995952 ) ) ;
#54894 = CARTESIAN_POINT ( 'NONE',  ( 28.20937500061451786, -4.541064518000417216, -2.621784821875001281 ) ) ;
#54895 = CARTESIAN_POINT ( 'NONE',  ( 3.084375000614519191, 6.421520780324663323E-16, -5.243569643749999010 ) ) ;
#54896 = CARTESIAN_POINT ( 'NONE',  ( 13.12500000000000178, 6.123233995736764310E-16, -4.999999999999998224 ) ) ;
#54897 = CARTESIAN_POINT ( 'NONE',  ( 11.72812500061451857, 4.541064518000418104, 2.621784821874999949 ) ) ;
#54898 = DIRECTION ( 'NONE',  ( -1.000000000000000000, -0.000000000000000000, -0.000000000000000000 ) ) ;
#54899 = CARTESIAN_POINT ( 'NONE',  ( 29.46562500061451928, -6.054752690667223547, -1.112240025338166033E-15 ) ) ;
#54900 = CARTESIAN_POINT ( 'NONE',  ( 16.65000000122903501, -2.886751345948129988, 4.999999999999997335 ) ) ;
#54901 = CYLINDRICAL_SURFACE ( 'NONE', #18232, 5.000000000000000000 ) ;
#54902 = CARTESIAN_POINT ( 'NONE',  ( 15.49687500061451750, -2.746126346562646425, 4.756430356249996549 ) ) ;
#54903 = CARTESIAN_POINT ( 'NONE',  ( 5.765625000614519102, 3.027376345333613106, -5.243569643749998122 ) ) ;
#54904 = CARTESIAN_POINT ( 'NONE',  ( 21.83437500061451786, -4.541064518000419881, 2.621784821874995952 ) ) ;
#54905 = CARTESIAN_POINT ( 'NONE',  ( -2.121784821874996840, 17.68437500061451928, 33.67503911421598417 ) ) ;
#54906 = CARTESIAN_POINT ( 'NONE',  ( 20.63437500061451857, 6.421520780324663323E-16, -5.243569643749999010 ) ) ;
#54907 = CARTESIAN_POINT ( 'NONE',  ( 29.14687500061451075, -3.027376345333610441, -5.243569643749999898 ) ) ;
#54908 = CARTESIAN_POINT ( 'NONE',  ( 9.001249775931846008E-16, 18.17187500061451999, 34.90005215228797653 ) ) ;
#54909 = CARTESIAN_POINT ( 'NONE',  ( 11.87812500061451537, -4.541064518000419881, 2.621784821874995952 ) ) ;
#54910 = CARTESIAN_POINT ( 'NONE',  ( 4.012500001229033053, 0.000000000000000000, 4.999999999999998224 ) ) ;
#54911 = ADVANCED_FACE ( 'NONE', ( #34222 ), #56755, .F. ) ;
#54912 = CARTESIAN_POINT ( 'NONE',  ( 7.771875000614516971, 3.027376345333611329, 5.243569643749999010 ) ) ;
#54913 = DIRECTION ( 'NONE',  ( 1.000000000000000000, 0.000000000000000000, 0.000000000000000000 ) ) ;
#54914 = COLOUR_RGB ( '',0.8941176470588234615, 0.8941176470588234615, 0.8941176470588234615 ) ;
#54915 = CARTESIAN_POINT ( 'NONE',  ( 10.64062500061451644, -3.027376345333610441, -5.243569643749999898 ) ) ;
#54916 = CARTESIAN_POINT ( 'NONE',  ( 15.19687500061451857, -3.027376345333610441, -5.243569643749999898 ) ) ;
#54917 = CARTESIAN_POINT ( 'NONE',  ( 25.57499999999999929, -4.330127018922194537, 2.499999999999995559 ) ) ;
#54918 = CARTESIAN_POINT ( 'NONE',  ( 20.32500000122903572, -5.773502691896255534, -1.060575238724906372E-15 ) ) ;
#54919 = CARTESIAN_POINT ( 'NONE',  ( 8.784375000614518925, -4.541064518000419881, 2.621784821874995952 ) ) ;
#54920 = CARTESIAN_POINT ( 'NONE',  ( 12.92812500061451786, 6.421520780324663323E-16, -5.243569643749999010 ) ) ;
#54921 = CARTESIAN_POINT ( 'NONE',  ( 26.86875000122903145, 2.886751345948126879, 4.999999999999999112 ) ) ;
#54922 = CARTESIAN_POINT ( 'NONE',  ( 21.49687500061451573, -3.027376345333610441, -5.243569643749999898 ) ) ;
#54923 = CARTESIAN_POINT ( 'NONE',  ( -3.780580586577210855, 3.275490995243301562, 28.66886852906538863 ) ) ;
#54924 = DIRECTION ( 'NONE',  ( 0.000000000000000000, 0.000000000000000000, 1.000000000000000000 ) ) ;
#54925 = CARTESIAN_POINT ( 'NONE',  ( -2.121784821874996840, 12.28437500061451892, -26.32496088578401583 ) ) ;
#54926 = CARTESIAN_POINT ( 'NONE',  ( 14.51250000122903394, -4.330127018922190985, -2.500000000000001332 ) ) ;
#54927 =( BOUNDED_CURVE ( )  B_SPLINE_CURVE ( 2, ( #29416, #18667, #24221, #45691, #63741, #29770, #34583 ),
 .UNSPECIFIED., .F., .F. ) 
 B_SPLINE_CURVE_WITH_KNOTS ( ( 3, 2, 2, 3 ),
 ( 0.2700000000000000733, 0.2733333333333333726, 0.2766666666666666718, 0.2800000000000000266 ),
 .UNSPECIFIED. ) 
 CURVE ( )  GEOMETRIC_REPRESENTATION_ITEM ( )  RATIONAL_B_SPLINE_CURVE ( ( 0.9999999999999977796, 0.8660254037844409281, 1.000000000000000000, 0.8660254037844387076, 1.000000000000000000, 0.8660254037844387076, 1.000000000000000000 ) ) 
 REPRESENTATION_ITEM ( '' )  );
#54928 = VECTOR ( 'NONE', #71502, 1000.000000000000000 ) ;
#54929 = CARTESIAN_POINT ( 'NONE',  ( 9.001249775931846008E-16, 14.51562500061451466, -25.09994784771203058 ) ) ;
#54930 = CARTESIAN_POINT ( 'NONE',  ( 17.70000000122903216, -2.886751345948125991, -5.000000000000000000 ) ) ;
#54931 = CARTESIAN_POINT ( 'NONE',  ( 10.71562500061451928, 3.027376345333613106, -5.243569643749998122 ) ) ;
#54932 = ORIENTED_EDGE ( 'NONE', *, *, #21442, .F. ) ;
#54933 = AXIS2_PLACEMENT_3D ( 'NONE', #18597, #13060, #41514 ) ;
#54934 = CARTESIAN_POINT ( 'NONE',  ( 15.90000000000000036, 4.330127018922192761, -2.499999999999997780 ) ) ;
#54935 = CARTESIAN_POINT ( 'NONE',  ( 13.74375000122903323, 5.773502691896255534, 3.535250795749688401E-16 ) ) ;
#54936 = CARTESIAN_POINT ( 'NONE',  ( 23.65312500061451573, -4.541064518000417216, -2.621784821875001281 ) ) ;
#54937 = CARTESIAN_POINT ( 'NONE',  ( 11.03437500061451715, -4.541064518000419881, 2.621784821874995952 ) ) ;
#54938 = EDGE_CURVE ( 'NONE', #39465, #54059, #22049, .T. ) ;
#54939 = CARTESIAN_POINT ( 'NONE',  ( 2.000000000000000444, 17.01874999877096428, 26.53589838486224650 ) ) ;
#54940 = CARTESIAN_POINT ( 'NONE',  ( 10.31250000122903288, 0.000000000000000000, 4.999999999999998224 ) ) ;
#54941 = CARTESIAN_POINT ( 'NONE',  ( 18.67500000122903714, 2.886751345948129099, -4.999999999999998224 ) ) ;
#54942 = CARTESIAN_POINT ( 'NONE',  ( 15.06562500061451537, -6.054752690667223547, -1.112240025338166033E-15 ) ) ;
#54943 = CARTESIAN_POINT ( 'NONE',  ( 17.12812500061451715, 4.541064518000418104, 2.621784821874999949 ) ) ;
#54944 = CARTESIAN_POINT ( 'NONE',  ( 24.60000000122903430, 5.773502691896255534, 3.535250795749688894E-16 ) ) ;
#54945 = CARTESIAN_POINT ( 'NONE',  ( 4.378125000614518925, 6.421520780324663323E-16, -5.243569643749999010 ) ) ;
#54946 = CARTESIAN_POINT ( 'NONE',  ( 25.50000000000000000, 0.000000000000000000, 4.999999999999998224 ) ) ;
#54947 = CARTESIAN_POINT ( 'NONE',  ( 3.756430356249998770, 13.95312499938548179, 32.16877607737302469 ) ) ;
#54948 = CARTESIAN_POINT ( 'NONE',  ( 26.78437500061451360, -4.541064518000419881, 2.621784821874995952 ) ) ;
#54949 = CYLINDRICAL_SURFACE ( 'NONE', #7589, 4.000000000000000000 ) ;
#54950 = CARTESIAN_POINT ( 'NONE',  ( 12.63750000122903394, -4.330127018922194537, 2.499999999999995559 ) ) ;
#54951 = CARTESIAN_POINT ( 'NONE',  ( 3.975000000000002753, -4.330127018922194537, 2.499999999999995559 ) ) ;
#54952 = EDGE_CURVE ( 'NONE', #35925, #52021, #33708, .T. ) ;
#54953 = CARTESIAN_POINT ( 'NONE',  ( 0.000000000000000000, 20.00000000000000000, -30.00000000000000000 ) ) ;
#54954 = CARTESIAN_POINT ( 'NONE',  ( 8.521875000614516082, 3.027376345333613106, -5.243569643749998122 ) ) ;
#54955 = CARTESIAN_POINT ( 'NONE',  ( 26.20312500061451644, 0.000000000000000000, 5.243569643749999010 ) ) ;
#54956 = CARTESIAN_POINT ( 'NONE',  ( 4.000000000000000000, 17.03750000000000142, 27.69059892324149885 ) ) ;
#54957 = CARTESIAN_POINT ( 'NONE',  ( 1.626862140677534273E-15, 13.92500000122903181, 34.00000000000000000 ) ) ;
#54958 = CARTESIAN_POINT ( 'NONE',  ( 4.385796401931335353, -2.400997692794667682, 4.385796401931427724 ) ) ;
#54959 = CARTESIAN_POINT ( 'NONE',  ( 5.634375000614519458, -4.541064518000419881, 2.621784821874995952 ) ) ;
#54960 = CARTESIAN_POINT ( 'NONE',  ( 9.571875000614518569, 3.027376345333611329, 5.243569643749999010 ) ) ;
#54961 = CARTESIAN_POINT ( 'NONE',  ( 29.10937500061451644, -4.541064518000417216, -2.621784821875001281 ) ) ;
#54962 = CARTESIAN_POINT ( 'NONE',  ( 2.121784821874999061, 12.45312500061459637, 26.32496088578401583 ) ) ;
#54963 = CARTESIAN_POINT ( 'NONE',  ( 22.27499999999999858, 4.330127018922191873, 2.499999999999999556 ) ) ;
#54964 = ORIENTED_EDGE ( 'NONE', *, *, #45125, .T. ) ;
#54965 = CARTESIAN_POINT ( 'NONE',  ( 28.42499999999999716, 6.123233995736764310E-16, -4.999999999999998224 ) ) ;
#54966 = CARTESIAN_POINT ( 'NONE',  ( 4.650000000000001243, 4.330127018922192761, -2.499999999999997780 ) ) ;
#54967 = EDGE_LOOP ( 'NONE', ( #36684, #55395, #28544, #2397 ) ) ;
#54968 = CARTESIAN_POINT ( 'NONE',  ( 19.04062500061451146, -3.027376345333614438, 5.243569643749998122 ) ) ;
#54969 = CARTESIAN_POINT ( 'NONE',  ( 10.45312500061451644, 0.000000000000000000, 5.243569643749999010 ) ) ;
#54970 = CARTESIAN_POINT ( 'NONE',  ( 20.93437500061451217, -2.746126346562642428, -4.756430356249999214 ) ) ;
#54971 = CARTESIAN_POINT ( 'NONE',  ( 7.059375000614518392, -4.541064518000417216, -2.621784821875001281 ) ) ;
#54972 = CARTESIAN_POINT ( 'NONE',  ( 20.92500000122903714, 2.886751345948129099, -4.999999999999998224 ) ) ;
#54973 = CARTESIAN_POINT ( 'NONE',  ( 3.237770964828680764, -3.810424094601559286, -3.237770964828680764 ) ) ;
#54974 = VECTOR ( 'NONE', #71880, 1000.000000000000000 ) ;
#54975 = CARTESIAN_POINT ( 'NONE',  ( 6.834375000614518747, 4.541064518000418104, 2.621784821874999949 ) ) ;
#54976 = CARTESIAN_POINT ( 'NONE',  ( 14.40937500061451715, 4.541064518000418104, -2.621784821874998173 ) ) ;
#54977 = CARTESIAN_POINT ( 'NONE',  ( 23.25937500061451857, -4.541064518000417216, -2.621784821875001281 ) ) ;
#54978 = CARTESIAN_POINT ( 'NONE',  ( -1.071796769724483234, 16.30759618943233491, 25.99999999999999645 ) ) ;
#54979 = VERTEX_POINT ( 'NONE', #29774 ) ;
#54980 = CARTESIAN_POINT ( 'NONE',  ( 13.95000000000000107, -4.330127018922190985, -2.500000000000001332 ) ) ;
#54981 = CARTESIAN_POINT ( 'NONE',  ( 18.45937500061451431, 4.541064518000418104, -2.621784821874998173 ) ) ;
#54982 = CARTESIAN_POINT ( 'NONE',  ( 9.834375000614517859, 6.421520780324663323E-16, -5.243569643749999010 ) ) ;
#54983 = CARTESIAN_POINT ( 'NONE',  ( -3.756430356249999214, 15.07812499938548356, 27.83122392262697531 ) ) ;
#54984 = CARTESIAN_POINT ( 'NONE',  ( 20.21250000000000213, -5.773502691896255534, -1.060575238724906372E-15 ) ) ;
#54985 = CARTESIAN_POINT ( 'NONE',  ( 1.999999999999997335, 14.67500000000000071, 33.46410161513775705 ) ) ;
#54986 = CARTESIAN_POINT ( 'NONE',  ( -3.000416591977282496E-16, 10.74687500061451928, -34.90005215228797653 ) ) ;
#54987 = CARTESIAN_POINT ( 'NONE',  ( 21.87187500061451573, -5.492252693125287522, -1.008910452111647106E-15 ) ) ;
#54988 = CARTESIAN_POINT ( 'NONE',  ( 13.56562500061451892, 3.027376345333611329, 5.243569643749999010 ) ) ;
#54989 = CARTESIAN_POINT ( 'NONE',  ( 3.037500000000002309, -2.886751345948129988, 4.999999999999997335 ) ) ;
#54990 = CARTESIAN_POINT ( 'NONE',  ( 4.898587196589411843E-16, 20.00000000000000000, -26.00000000000000000 ) ) ;
#54991 = CARTESIAN_POINT ( 'NONE',  ( 27.72187500061451715, -6.054752690667223547, -1.112240025338166033E-15 ) ) ;
#54992 = CARTESIAN_POINT ( 'NONE',  ( 11.13750000000000284, -2.886751345948129988, 4.999999999999997335 ) ) ;
#54993 = CARTESIAN_POINT ( 'NONE',  ( -3.999999999999999112, 18.76250000122903216, 30.00000000000000000 ) ) ;
#54994 = CARTESIAN_POINT ( 'NONE',  ( 12.15000000122903501, -2.886751345948129988, 4.999999999999997335 ) ) ;
#54995 = CARTESIAN_POINT ( 'NONE',  ( 22.54687500061451999, 6.054752690667223547, 3.707466751127219781E-16 ) ) ;
#54996 = CARTESIAN_POINT ( 'NONE',  ( 17.55937500061451573, 4.541064518000418104, -2.621784821874998173 ) ) ;
#54997 = CARTESIAN_POINT ( 'NONE',  ( 3.981242275647779216, 3.024881775420318331, -4.283141675081658661 ) ) ;
#54998 = ORIENTED_EDGE ( 'NONE', *, *, #30954, .T. ) ;
#54999 = CARTESIAN_POINT ( 'NONE',  ( 16.26562500061451289, 3.027376345333611329, 5.243569643749999010 ) ) ;
#55000 = CARTESIAN_POINT ( 'NONE',  ( 29.13750000122903216, 4.330127018922191873, 2.499999999999999556 ) ) ;
#55001 = CARTESIAN_POINT ( 'NONE',  ( 18.72187500061451360, -6.054752690667223547, -1.112240025338166033E-15 ) ) ;
#55002 = CARTESIAN_POINT ( 'NONE',  ( 3.065625000614517592, 3.027376345333613106, -5.243569643749998122 ) ) ;
#55003 = CARTESIAN_POINT ( 'NONE',  ( 18.89062500061451644, 6.054752690667223547, 3.707466751127219781E-16 ) ) ;
#55004 = CARTESIAN_POINT ( 'NONE',  ( 30.00000000000000000, 0.000000000000000000, 4.999999999999998224 ) ) ;
#55005 = CARTESIAN_POINT ( 'NONE',  ( 29.10937500061451644, -4.541064518000417216, -2.621784821875001281 ) ) ;
#55006 = CARTESIAN_POINT ( 'NONE',  ( -4.243569643749999898, 12.60312500061451679, 30.00000000000000000 ) ) ;
#55007 = CARTESIAN_POINT ( 'NONE',  ( 18.60937500061451644, 0.000000000000000000, 5.243569643749999010 ) ) ;
#55008 = CARTESIAN_POINT ( 'NONE',  ( 15.15000000122903323, 5.773502691896255534, 3.535250795749688894E-16 ) ) ;
#55009 = CARTESIAN_POINT ( 'NONE',  ( 10.32187500061451679, 2.746126346562645981, -4.756430356249997438 ) ) ;
#55010 = CARTESIAN_POINT ( 'NONE',  ( -2.121784821874999949, 19.33437500061451786, -33.67503911421598417 ) ) ;
#55011 = EDGE_CURVE ( 'NONE', #29428, #13883, #11672, .T. ) ;
#55012 = CARTESIAN_POINT ( 'NONE',  ( 19.65937500061451360, -4.541064518000417216, -2.621784821875001281 ) ) ;
#55013 = CARTESIAN_POINT ( 'NONE',  ( 21.97500000122903074, 2.886751345948126879, 4.999999999999999112 ) ) ;
#55014 = CARTESIAN_POINT ( 'NONE',  ( 17.10937500061451999, 4.541064518000418104, -2.621784821874998173 ) ) ;
#55015 = CARTESIAN_POINT ( 'NONE',  ( 13.19062500061451537, -3.027376345333614438, 5.243569643749998122 ) ) ;
#55016 = CARTESIAN_POINT ( 'NONE',  ( -4.243569643749999898, 13.52187500061451786, 27.54997392385601529 ) ) ;
#55017 = VECTOR ( 'NONE', #3418, 1000.000000000000000 ) ;
#55018 = CARTESIAN_POINT ( 'NONE',  ( 16.71562500061451573, 3.027376345333611329, 5.243569643749999010 ) ) ;
#55019 = ORIENTED_EDGE ( 'NONE', *, *, #33157, .T. ) ;
#55020 = ORIENTED_EDGE ( 'NONE', *, *, #40081, .T. ) ;
#55021 = CARTESIAN_POINT ( 'NONE',  ( 21.93750000000000000, -2.886751345948129988, 4.999999999999997335 ) ) ;
#55022 = CARTESIAN_POINT ( 'NONE',  ( 4.243569643749999898, 18.69687500061451857, -27.54997392385601529 ) ) ;
#55023 = CARTESIAN_POINT ( 'NONE',  ( 14.90625000122903110, -4.330127018922190985, -2.500000000000001332 ) ) ;
#55024 = CARTESIAN_POINT ( 'NONE',  ( 24.32812500061451289, 4.541064518000418104, 2.621784821874999949 ) ) ;
#55025 = CARTESIAN_POINT ( 'NONE',  ( 6.178125000614518747, 6.421520780324663323E-16, -5.243569643749999010 ) ) ;
#55026 = CARTESIAN_POINT ( 'NONE',  ( 17.96250000122903501, 0.000000000000000000, 4.999999999999998224 ) ) ;
#55027 = CARTESIAN_POINT ( 'NONE',  ( 23.24062500061451786, -3.027376345333610441, -5.243569643749999898 ) ) ;
#55028 = CARTESIAN_POINT ( 'NONE',  ( 24.00000000000000000, 4.330127018922192761, -2.499999999999997780 ) ) ;
#55029 = CARTESIAN_POINT ( 'NONE',  ( 26.20312500061451644, 0.000000000000000000, 5.243569643749999010 ) ) ;
#55030 = CARTESIAN_POINT ( 'NONE',  ( 5.728125000614515905, 6.421520780324663323E-16, -5.243569643749999010 ) ) ;
#55031 = ORIENTED_EDGE ( 'NONE', *, *, #10471, .F. ) ;
#55032 = B_SPLINE_CURVE_WITH_KNOTS ( 'NONE', 3,
 ( #64528, #58613, #30556, #53082, #13922, #72274, #9848, #43473, #10216, #54551 ),
 .UNSPECIFIED., .F., .F.,
 ( 4, 3, 3, 4 ),
 ( 0.000000000000000000, 2.812506322124666422E-05, 5.625012732888523369E-05, 9.479223614486993082E-05 ),
 .UNSPECIFIED. ) ;
#55033 = CARTESIAN_POINT ( 'NONE',  ( 22.26562500061451644, -6.054752690667223547, -1.112240025338166033E-15 ) ) ;
#55034 = CARTESIAN_POINT ( 'NONE',  ( 4.078125000614517326, 4.541064518000418104, 2.621784821874999949 ) ) ;
#55035 = CARTESIAN_POINT ( 'NONE',  ( 11.44687500061451857, -2.746126346562646425, 4.756430356249996549 ) ) ;
#55036 = CARTESIAN_POINT ( 'NONE',  ( 10.98750000122903536, 6.123233995736764310E-16, -4.999999999999998224 ) ) ;
#55037 = CARTESIAN_POINT ( 'NONE',  ( -2.828200636599751609E-16, 14.15000000122903501, -34.61880215351700230 ) ) ;
#55038 = CARTESIAN_POINT ( 'NONE',  ( 13.63125000122903252, 6.123233995736764310E-16, -4.999999999999998224 ) ) ;
#55039 = ADVANCED_FACE ( 'NONE', ( #69310 ), #41233, .F. ) ;
#55040 = CARTESIAN_POINT ( 'NONE',  ( 11.02500000000000036, 4.330127018922191873, 2.499999999999999556 ) ) ;
#55041 = CARTESIAN_POINT ( 'NONE',  ( 10.28437500061451715, 6.421520780324663323E-16, -5.243569643749999010 ) ) ;
#55042 = CARTESIAN_POINT ( 'NONE',  ( 6.975000001229032520, 2.886751345948129099, -4.999999999999998224 ) ) ;
#55043 = CARTESIAN_POINT ( 'NONE',  ( 14.29687500061451821, -3.027376345333610441, -5.243569643749999898 ) ) ;
#55044 = CARTESIAN_POINT ( 'NONE',  ( 5.146875000614517859, -3.027376345333614438, 5.243569643749998122 ) ) ;
#55045 = CARTESIAN_POINT ( 'NONE',  ( 7.320879633048903241E-15, 18.53750000000000142, 26.00000000000000355 ) ) ;
#55046 = VECTOR ( 'NONE', #4027, 1000.000000000000000 ) ;
#55047 = CYLINDRICAL_SURFACE ( 'NONE', #40685, 4.999999999999998224 ) ;
#55048 = CARTESIAN_POINT ( 'NONE',  ( 12.08437500061451608, 6.421520780324663323E-16, -5.243569643749999010 ) ) ;
#55049 = CARTESIAN_POINT ( 'NONE',  ( 6.150000001229033231, 5.773502691896255534, 3.535250795749688401E-16 ) ) ;
#55050 = EDGE_CURVE ( 'NONE', #1482, #59687, #5881, .T. ) ;
#55051 = CARTESIAN_POINT ( 'NONE',  ( 21.21562500061451573, 3.027376345333611329, 5.243569643749999010 ) ) ;
#55052 = CARTESIAN_POINT ( 'NONE',  ( 19.61249999999999716, 2.886751345948126879, 4.999999999999998224 ) ) ;
#55053 = DIRECTION ( 'NONE',  ( 0.000000000000000000, 0.000000000000000000, -1.000000000000000000 ) ) ;
#55054 = CARTESIAN_POINT ( 'NONE',  ( 22.54687500061451999, 6.054752690667223547, 3.707466751127219781E-16 ) ) ;
#55055 = CARTESIAN_POINT ( 'NONE',  ( 29.73749999999999716, -2.886751345948115777, -5.000000000000017764 ) ) ;
#55056 = CARTESIAN_POINT ( 'NONE',  ( 2.915625000614516793, -6.054752690667223547, -1.112240025338166033E-15 ) ) ;
#55057 = CARTESIAN_POINT ( 'NONE',  ( 19.24687500061451573, 4.119189519843966529, -2.378215178124998275 ) ) ;
#55058 = CARTESIAN_POINT ( 'NONE',  ( 24.77812500061451217, 4.541064518000418104, 2.621784821874999949 ) ) ;
#55059 = CARTESIAN_POINT ( 'NONE',  ( 17.09062500061451573, 6.054752690667223547, 3.707466751127219781E-16 ) ) ;
#55060 = CARTESIAN_POINT ( 'NONE',  ( 14.08125000122903181, 6.123233995736764310E-16, -4.999999999999998224 ) ) ;
#55061 = CARTESIAN_POINT ( 'NONE',  ( 14.25937500061451679, -4.541064518000417216, -2.621784821875001281 ) ) ;
#55062 = CARTESIAN_POINT ( 'NONE',  ( 7.162500001229032520, 0.000000000000000000, 4.999999999999998224 ) ) ;
#55063 = CARTESIAN_POINT ( 'NONE',  ( 27.07500000122903216, -5.773502691896255534, -1.060575238724906372E-15 ) ) ;
#55064 = CARTESIAN_POINT ( 'NONE',  ( 6.309375000614517504, 4.541064518000418104, -2.621784821874998173 ) ) ;
#55065 = CARTESIAN_POINT ( 'NONE',  ( 16.13437500061451502, 6.421520780324663323E-16, -5.243569643749999010 ) ) ;
#55066 = CARTESIAN_POINT ( 'NONE',  ( -5.810221930991193690E-16, 11.78749999999999964, 26.00000000000000355 ) ) ;
#55067 = CARTESIAN_POINT ( 'NONE',  ( 4.500000001229034652, -2.886751345948129988, 4.999999999999997335 ) ) ;
#55068 = CARTESIAN_POINT ( 'NONE',  ( 25.43437500061451573, -4.541064518000419881, 2.621784821874995952 ) ) ;
#55069 = CARTESIAN_POINT ( 'NONE',  ( 16.65937500061452070, 4.541064518000418104, -2.621784821874998173 ) ) ;
#55070 = CARTESIAN_POINT ( 'NONE',  ( 3.756430356250000546, 16.39062499938548356, 27.83122392262697886 ) ) ;
#55071 = CARTESIAN_POINT ( 'NONE',  ( 28.61249999999999716, 2.886751345948126879, 4.999999999999999112 ) ) ;
#55072 = EDGE_CURVE ( 'NONE', #53581, #30832, #13395, .T. ) ;
#55073 = CARTESIAN_POINT ( 'NONE',  ( 6.450000000000001066, 4.330127018922192761, -2.499999999999997780 ) ) ;
#55074 = CARTESIAN_POINT ( 'NONE',  ( 28.62187500061451573, -5.492252693125287522, -1.008910452111647106E-15 ) ) ;
#55075 = CARTESIAN_POINT ( 'NONE',  ( 20.54062500061451502, -3.027376345333610441, -5.243569643749999898 ) ) ;
#55076 = CARTESIAN_POINT ( 'NONE',  ( 9.674999999999998934, 4.330127018922191873, 2.499999999999999556 ) ) ;
#55077 =( BOUNDED_CURVE ( )  B_SPLINE_CURVE ( 2, ( #58062, #57707, #51816, #35542, #7112, #29641, #1581 ),
 .UNSPECIFIED., .F., .F. ) 
 B_SPLINE_CURVE_WITH_KNOTS ( ( 3, 2, 2, 3 ),
 ( 0.7416666666666666963, 0.7444444444444444642, 0.7472222222222222321, 0.7500000000000000000 ),
 .UNSPECIFIED. ) 
 CURVE ( )  GEOMETRIC_REPRESENTATION_ITEM ( )  RATIONAL_B_SPLINE_CURVE ( ( 1.000000000000000000, 0.8660254037844387076, 1.000000000000000000, 0.8660254037844387076, 1.000000000000000000, 0.8660254037844387076, 1.000000000000000000 ) ) 
 REPRESENTATION_ITEM ( '' )  );
#55078 = CARTESIAN_POINT ( 'NONE',  ( 3.853125000614517681, -4.541064518000417216, -2.621784821875001281 ) ) ;
#55079 = CARTESIAN_POINT ( 'NONE',  ( 19.98749999999999716, 5.773502691896255534, 3.535250795749688894E-16 ) ) ;
#55080 = CARTESIAN_POINT ( 'NONE',  ( 3.999999999999998668, 16.45624999877096784, 32.30940107675850470 ) ) ;
#55081 = CARTESIAN_POINT ( 'NONE',  ( 23.36250000122903359, 0.000000000000000000, 4.999999999999998224 ) ) ;
#55082 = CARTESIAN_POINT ( 'NONE',  ( 5.838630383562665394, 8.118670948950970967, 31.39639828276943945 ) ) ;
#55083 = CARTESIAN_POINT ( 'NONE',  ( 29.52187500061451431, -6.054752690667223547, -1.112240025338166033E-15 ) ) ;
#55084 = ORIENTED_EDGE ( 'NONE', *, *, #2651, .T. ) ;
#55085 = CARTESIAN_POINT ( 'NONE',  ( 17.27812500061451217, -4.541064518000419881, 2.621784821874995952 ) ) ;
#55086 = CARTESIAN_POINT ( 'NONE',  ( 25.30312500061451431, 0.000000000000000000, 5.243569643749999010 ) ) ;
#55087 = CARTESIAN_POINT ( 'NONE',  ( 23.63437500061451502, -4.541064518000419881, 2.621784821874995952 ) ) ;
#55088 = CARTESIAN_POINT ( 'NONE',  ( 6.862500000000002487, 2.886751345948129099, -4.999999999999998224 ) ) ;
#55089 = CARTESIAN_POINT ( 'NONE',  ( 11.57812500061451644, 6.421520780324663323E-16, -5.243569643749999010 ) ) ;
#55090 = CARTESIAN_POINT ( 'NONE',  ( 26.57812500061451644, 4.541064518000418104, 2.621784821874999949 ) ) ;
#55091 = CARTESIAN_POINT ( 'NONE',  ( 14.82187500061451679, 3.027376345333613106, -5.243569643749998122 ) ) ;
#55092 = CARTESIAN_POINT ( 'NONE',  ( 19.92187500061451644, 3.027376345333611329, 5.243569643749999010 ) ) ;
#55093 = CARTESIAN_POINT ( 'NONE',  ( 1.071796769724489895, 11.87990381179669974, -34.00000000000000000 ) ) ;
#55094 = CARTESIAN_POINT ( 'NONE',  ( 4.243569643749999898, 10.63437500061451857, 30.00000000000000000 ) ) ;
#55095 = EDGE_CURVE ( 'NONE', #31243, #1482, #5450, .T. ) ;
#55096 = CARTESIAN_POINT ( 'NONE',  ( 24.63750000122903216, 4.330127018922191873, 2.499999999999999556 ) ) ;
#55097 = CARTESIAN_POINT ( 'NONE',  ( 17.14687500061451786, 5.492252693125287522, 3.363034840372157021E-16 ) ) ;
#55098 = CARTESIAN_POINT ( 'NONE',  ( 15.47812500061451679, -4.541064518000419881, 2.621784821874995952 ) ) ;
#55099 = CARTESIAN_POINT ( 'NONE',  ( 7.134375000614516793, 6.421520780324663323E-16, -5.243569643749999010 ) ) ;
#55100 = CARTESIAN_POINT ( 'NONE',  ( 8.034375000614518925, 6.421520780324663323E-16, -5.243569643749999010 ) ) ;
#55101 = ORIENTED_EDGE ( 'NONE', *, *, #5758, .F. ) ;
#55102 = CARTESIAN_POINT ( 'NONE',  ( 27.94687500061451502, 6.054752690667223547, 3.707466751127219781E-16 ) ) ;
#55103 = CARTESIAN_POINT ( 'NONE',  ( 18.77812500061451573, 6.421520780324663323E-16, -5.243569643749999010 ) ) ;
#55104 = CARTESIAN_POINT ( 'NONE',  ( 29.43750000122903288, 6.123233995736764310E-16, -4.999999999999998224 ) ) ;
#55105 = CARTESIAN_POINT ( 'NONE',  ( 3.309375000614518836, 0.000000000000000000, 5.243569643749999010 ) ) ;
#55106 = CARTESIAN_POINT ( 'NONE',  ( 23.78437500061451360, 6.421520780324663323E-16, -5.243569643749999010 ) ) ;
#55107 = CARTESIAN_POINT ( 'NONE',  ( 20.39062500061451644, -3.027376345333614438, 5.243569643749998122 ) ) ;
#55108 = CARTESIAN_POINT ( 'NONE',  ( 3.999999999999998668, 12.61250000000000071, 27.69059892324149175 ) ) ;
#55109 = CARTESIAN_POINT ( 'NONE',  ( 25.19062500061451715, 6.054752690667223547, 3.707466751127219781E-16 ) ) ;
#55110 = CARTESIAN_POINT ( 'NONE',  ( 5.175000001229033586, 2.886751345948129099, -4.999999999999998224 ) ) ;
#55111 = ORIENTED_EDGE ( 'NONE', *, *, #25529, .T. ) ;
#55112 = CARTESIAN_POINT ( 'NONE',  ( 2.925000001229034918, 2.886751345948129099, -4.999999999999998224 ) ) ;
#55113 = CARTESIAN_POINT ( 'NONE',  ( 4.000000000000000000, 14.78750000000000320, -27.69059892324149530 ) ) ;
#55114 = CARTESIAN_POINT ( 'NONE',  ( 22.23750000122903003, 6.123233995736764310E-16, -4.999999999999998224 ) ) ;
#55115 = CARTESIAN_POINT ( 'NONE',  ( 3.756430356250000102, 15.90312499938548108, 30.00000000000000000 ) ) ;
#55116 = CARTESIAN_POINT ( 'NONE',  ( 3.534375000614518036, 6.421520780324663323E-16, -5.243569643749999010 ) ) ;
#55117 = CARTESIAN_POINT ( 'NONE',  ( 30.00000000000000000, 0.000000000000000000, 0.000000000000000000 ) ) ;
#55118 = CARTESIAN_POINT ( 'NONE',  ( 11.46562500061451573, -6.054752690667223547, -1.112240025338166033E-15 ) ) ;
#55119 = CARTESIAN_POINT ( 'NONE',  ( 6.684375000614518392, 6.421520780324663323E-16, -5.243569643749999010 ) ) ;
#55120 = CARTESIAN_POINT ( 'NONE',  ( 24.15000000122903145, 5.773502691896255534, 3.535250795749688894E-16 ) ) ;
#55121 = VECTOR ( 'NONE', #46243, 1000.000000000000000 ) ;
#55122 = CARTESIAN_POINT ( 'NONE',  ( 14.59687500061452070, -3.027376345333614438, 5.243569643749998122 ) ) ;
#55123 = CARTESIAN_POINT ( 'NONE',  ( 28.97812500061451502, -4.541064518000419881, 2.621784821874995952 ) ) ;
#55124 = DIRECTION ( 'NONE',  ( -1.000000000000000000, -0.000000000000000000, -0.000000000000000000 ) ) ;
#55125 = CARTESIAN_POINT ( 'NONE',  ( 14.28749999999999787, -2.886751345948019409, 5.000000000000189182 ) ) ;
#55126 = CARTESIAN_POINT ( 'NONE',  ( 15.55312500061451608, -4.541064518000417216, -2.621784821875001281 ) ) ;
#55127 = ORIENTED_EDGE ( 'NONE', *, *, #14279, .T. ) ;
#55128 = CARTESIAN_POINT ( 'NONE',  ( 10.82812500061451644, 4.541064518000418104, 2.621784821874999949 ) ) ;
#55129 = CARTESIAN_POINT ( 'NONE',  ( 8.090625000614515727, 6.054752690667223547, 3.707466751127219781E-16 ) ) ;
#55130 = CARTESIAN_POINT ( 'NONE',  ( 19.58437500061451786, -4.119189519843968306, 2.378215178124996054 ) ) ;
#55131 = CARTESIAN_POINT ( 'NONE',  ( 8.400000000000000355, 0.000000000000000000, 4.999999999999998224 ) ) ;
#55132 = CARTESIAN_POINT ( 'NONE',  ( 3.412500001229032964, 4.330127018922192761, -2.499999999999997780 ) ) ;
#55133 = CARTESIAN_POINT ( 'NONE',  ( 17.58749999999999858, -2.886751345948125991, -5.000000000000000000 ) ) ;
#55134 =( BOUNDED_CURVE ( )  B_SPLINE_CURVE ( 2, ( #929, #28992, #29708, #23437, #12351, #68879, #57414, #45983, #68519 ),
 .UNSPECIFIED., .F., .F. ) 
 B_SPLINE_CURVE_WITH_KNOTS ( ( 3, 2, 2, 2, 3 ),
 ( 0.7361111111111111605, 0.7407407407407406996, 0.7500000000000000000, 0.7592592592592593004, 0.7638888888888889506 ),
 .UNSPECIFIED. ) 
 CURVE ( )  GEOMETRIC_REPRESENTATION_ITEM ( )  RATIONAL_B_SPLINE_CURVE ( ( 0.9330127018922192983, 0.9330127018922200755, 1.000000000000000000, 0.8660254037844387076, 1.000000000000000000, 0.8660254037844387076, 1.000000000000000000, 0.9330127018922185211, 0.9330127018922192983 ) ) 
 REPRESENTATION_ITEM ( '' )  );
#55135 = CARTESIAN_POINT ( 'NONE',  ( 19.32187500061451857, 3.027376345333613106, -5.243569643749998122 ) ) ;
#55136 = CARTESIAN_POINT ( 'NONE',  ( 14.58750000122903323, 6.123233995736764310E-16, -4.999999999999998224 ) ) ;
#55137 = CARTESIAN_POINT ( 'NONE',  ( 20.02500000000000213, 4.330127018922191873, 2.499999999999999556 ) ) ;
#55138 = CARTESIAN_POINT ( 'NONE',  ( 4.243569643749999898, 16.39062500061451999, -27.54997392385601529 ) ) ;
#55139 = CARTESIAN_POINT ( 'NONE',  ( 18.84375000122903643, -2.886751345948157965, 4.999999999999948486 ) ) ;
#55140 = CARTESIAN_POINT ( 'NONE',  ( 29.01562500061451644, -6.054752690667223547, -1.112240025338166033E-15 ) ) ;
#55141 = CARTESIAN_POINT ( 'NONE',  ( 17.23125000122903572, 6.123233995736764310E-16, -4.999999999999998224 ) ) ;
#55142 = CARTESIAN_POINT ( 'NONE',  ( 24.33749999999999858, -2.886751345948112224, -5.000000000000023981 ) ) ;
#55143 = CARTESIAN_POINT ( 'NONE',  ( 13.17187500061451999, 3.027376345333611329, 5.243569643749999010 ) ) ;
#55144 = CARTESIAN_POINT ( 'NONE',  ( 27.44999999999999929, -4.330127018922190985, -2.500000000000001332 ) ) ;
#55145 = CARTESIAN_POINT ( 'NONE',  ( 8.840625000614515727, -3.027376345333610441, -5.243569643749999898 ) ) ;
#55146 = CARTESIAN_POINT ( 'NONE',  ( 26.40937500061451360, 2.746126346562645981, -4.756430356249997438 ) ) ;
#55147 = CARTESIAN_POINT ( 'NONE',  ( 20.89687500061452141, -3.027376345333614438, 5.243569643749998122 ) ) ;
#55148 = CARTESIAN_POINT ( 'NONE',  ( 13.47187500061451715, 4.119189519843966529, 2.378215178124999607 ) ) ;
#55149 = CARTESIAN_POINT ( 'NONE',  ( 8.765625000614518214, -6.054752690667223547, -1.112240025338166033E-15 ) ) ;
#55150 = CARTESIAN_POINT ( 'NONE',  ( 13.47187500061451537, 3.027376345333613106, -5.243569643749998122 ) ) ;
#55151 = EDGE_LOOP ( 'NONE', ( #56905, #66056, #19598, #61136 ) ) ;
#55152 = CARTESIAN_POINT ( 'NONE',  ( 23.78437500061451360, 6.421520780324663323E-16, -5.243569643749999010 ) ) ;
#55153 = CARTESIAN_POINT ( 'NONE',  ( 3.779877903161416253, 3.276378095916669508, -31.33357467763542914 ) ) ;
#55154 = FACE_OUTER_BOUND ( 'NONE', #67073, .T. ) ;
#55155 = EDGE_CURVE ( 'NONE', #19407, #27917, #12981, .T. ) ;
#55156 = CARTESIAN_POINT ( 'NONE',  ( 5.512499999999999289, 2.886751345948129099, -4.999999999999998224 ) ) ;
#55157 = AXIS2_PLACEMENT_3D ( 'NONE', #320, #51283, #57171 ) ;
#55158 = CARTESIAN_POINT ( 'NONE',  ( 16.20000000122903216, -2.886751345948129988, 4.999999999999997335 ) ) ;
#55159 = CARTESIAN_POINT ( 'NONE',  ( 27.41250000122903430, 0.000000000000000000, 4.999999999999998224 ) ) ;
#55160 = CARTESIAN_POINT ( 'NONE',  ( -0.6945831915928805111, 10.00052343484236950, -33.93923269050669944 ) ) ;
#55161 = ORIENTED_EDGE ( 'NONE', *, *, #44604, .T. ) ;
#55162 = CARTESIAN_POINT ( 'NONE',  ( 12.71250000000000036, 2.886751345948129099, -4.999999999999998224 ) ) ;
#55163 = CARTESIAN_POINT ( 'NONE',  ( 16.46249999999999503, 2.886751345948126879, 4.999999999999999112 ) ) ;
#55164 = CARTESIAN_POINT ( 'NONE',  ( 13.31250000122903288, 4.330127018922192761, -2.499999999999997780 ) ) ;
#55165 = CARTESIAN_POINT ( 'NONE',  ( 11.69062500061451360, 6.054752690667223547, 3.707466751127219781E-16 ) ) ;
#55166 = VERTEX_POINT ( 'NONE', #12064 ) ;
#55167 = CARTESIAN_POINT ( 'NONE',  ( -3.999999999999999112, 16.96250000122903145, -30.00000000000000000 ) ) ;
#55168 = CARTESIAN_POINT ( 'NONE',  ( 4.243569643749999010, 13.82187500061451857, -32.45002607614398471 ) ) ;
#55169 = CARTESIAN_POINT ( 'NONE',  ( 4.678125000614516971, -4.541064518000419881, 2.621784821874995952 ) ) ;
#55170 = CARTESIAN_POINT ( 'NONE',  ( -7.967954043666661671E-16, 14.77812499938548463, 34.33755215474603517 ) ) ;
#55171 = CARTESIAN_POINT ( 'NONE',  ( 10.27499999999999858, -4.330127018922194537, 2.499999999999995559 ) ) ;
#55172 = CARTESIAN_POINT ( 'NONE',  ( 9.074999999999999289, 6.123233995736764310E-16, -4.999999999999998224 ) ) ;
#55173 = ORIENTED_EDGE ( 'NONE', *, *, #65759, .T. ) ;
#55174 = CARTESIAN_POINT ( 'NONE',  ( 24.77812500061451217, 4.541064518000418104, 2.621784821874999949 ) ) ;
#55175 = DIRECTION ( 'NONE',  ( 1.000000000000000000, 0.000000000000000000, 0.000000000000000000 ) ) ;
#55176 = CARTESIAN_POINT ( 'NONE',  ( -1.878215178124999163, 19.09062499938548285, 26.74683588394047007 ) ) ;
#55177 = CARTESIAN_POINT ( 'NONE',  ( 21.34687500061451715, -3.027376345333614438, 5.243569643749998122 ) ) ;
#55178 = CARTESIAN_POINT ( 'NONE',  ( 18.74062500061451431, -3.027376345333610441, -5.243569643749999898 ) ) ;
#55179 = EDGE_CURVE ( 'NONE', #44765, #63037, #25734, .T. ) ;
#55180 = CARTESIAN_POINT ( 'NONE',  ( -2.121784821874996840, 14.92812500061459424, -26.32496088578401583 ) ) ;
#55181 = CARTESIAN_POINT ( 'NONE',  ( 6.403125000614517504, 0.000000000000000000, 5.243569643749999010 ) ) ;
#55182 = CARTESIAN_POINT ( 'NONE',  ( 4.115625000614516082, 3.027376345333611329, 5.243569643749999010 ) ) ;
#55183 = CARTESIAN_POINT ( 'NONE',  ( 25.50937500061451502, -4.119189519843965641, -2.378215178125001383 ) ) ;
#55184 = CARTESIAN_POINT ( 'NONE',  ( 22.34062500061451573, -3.027376345333610441, -5.243569643749999898 ) ) ;
#55185 = CARTESIAN_POINT ( 'NONE',  ( 7.771875000614516971, 2.746126346562643317, 4.756430356249998326 ) ) ;
#55186 = CARTESIAN_POINT ( 'NONE',  ( 3.756430356249998770, 17.55312499938548143, 32.16877607737302469 ) ) ;
#55187 = CARTESIAN_POINT ( 'NONE',  ( 16.35937500061451644, 0.000000000000000000, 5.243569643749999010 ) ) ;
#55188 = CARTESIAN_POINT ( 'NONE',  ( 14.55937500061451573, 0.000000000000000000, 5.243569643749999010 ) ) ;
#55189 = CARTESIAN_POINT ( 'NONE',  ( 22.20937500061451431, 0.000000000000000000, 5.243569643749999010 ) ) ;
#55190 = ORIENTED_EDGE ( 'NONE', *, *, #30133, .T. ) ;
#55191 = CARTESIAN_POINT ( 'NONE',  ( 2.121784821875001281, 11.45937500061451786, 33.67503911421598417 ) ) ;
#55192 = CARTESIAN_POINT ( 'NONE',  ( 3.328125000614516438, -4.541064518000419881, 2.621784821874995952 ) ) ;
#55193 = CARTESIAN_POINT ( 'NONE',  ( 26.27812500061451573, -4.541064518000419881, 2.621784821874995952 ) ) ;
#55194 = EDGE_CURVE ( 'NONE', #3917, #70308, #63478, .T. ) ;
#55195 = CARTESIAN_POINT ( 'NONE',  ( 25.94062500061451715, -3.027376345333610441, -5.243569643749999898 ) ) ;
#55196 = CARTESIAN_POINT ( 'NONE',  ( 8.362500001229031810, 4.330127018922192761, -2.499999999999997780 ) ) ;
#55197 = CARTESIAN_POINT ( 'NONE',  ( 4.000000000000000000, 18.83749999999999858, 32.30940107675849049 ) ) ;
#55198 = CARTESIAN_POINT ( 'NONE',  ( 5.446875000614518569, 6.054752690667223547, 3.707466751127219781E-16 ) ) ;
#55199 = CARTESIAN_POINT ( 'NONE',  ( 0.000000000000000000, 0.000000000000000000, 0.000000000000000000 ) ) ;
#55200 = CARTESIAN_POINT ( 'NONE',  ( 14.62500000122903288, 2.886751345948129099, -4.999999999999998224 ) ) ;
#55201 = CARTESIAN_POINT ( 'NONE',  ( 8.325000001229033941, 2.886751345948129099, -4.999999999999998224 ) ) ;
#55202 = CARTESIAN_POINT ( 'NONE',  ( 3.140625000614516882, 6.054752690667223547, 3.707466751127219781E-16 ) ) ;
#55203 = CARTESIAN_POINT ( 'NONE',  ( 2.828200636599751609E-16, 16.15624999877096712, 25.38119784648299415 ) ) ;
#55204 = CARTESIAN_POINT ( 'NONE',  ( 19.25625000122903430, 0.000000000000000000, 4.999999999999998224 ) ) ;
#55205 = CARTESIAN_POINT ( 'NONE',  ( 12.79687500061451821, -3.027376345333614438, 5.243569643749998122 ) ) ;
#55206 = CARTESIAN_POINT ( 'NONE',  ( 29.45625000122903003, 4.330127018922192761, -2.499999999999997780 ) ) ;
#55207 = ORIENTED_EDGE ( 'NONE', *, *, #37992, .T. ) ;
#55208 = CARTESIAN_POINT ( 'NONE',  ( 20.76562500061451644, 3.027376345333611329, 5.243569643749999010 ) ) ;
#55209 = CARTESIAN_POINT ( 'NONE',  ( 14.37187500061451928, 3.027376345333613106, -5.243569643749998122 ) ) ;
#55210 = CARTESIAN_POINT ( 'NONE',  ( 5.090625000614516615, -3.027376345333614438, 5.243569643749998122 ) ) ;
#55211 = CARTESIAN_POINT ( 'NONE',  ( 23.07187500061452212, 3.027376345333611329, 5.243569643749999010 ) ) ;
#55212 = CARTESIAN_POINT ( 'NONE',  ( 6.365625000614518747, 3.027376345333611329, 5.243569643749999010 ) ) ;
#55213 = CARTESIAN_POINT ( 'NONE',  ( 9.112500001229033586, -4.330127018922190985, -2.500000000000001332 ) ) ;
#55214 = CARTESIAN_POINT ( 'NONE',  ( 23.31562500061451715, 3.027376345333613106, -5.243569643749998122 ) ) ;
#55215 = CARTESIAN_POINT ( 'NONE',  ( -1.999999999999997113, 17.03750000122903430, -26.53589838486224295 ) ) ;
#55216 = CARTESIAN_POINT ( 'NONE',  ( 8.512500001229033941, 0.000000000000000000, 4.999999999999998224 ) ) ;
#55217 = CARTESIAN_POINT ( 'NONE',  ( 17.54062500061451502, 6.054752690667223547, 3.707466751127219781E-16 ) ) ;
#55218 = CARTESIAN_POINT ( 'NONE',  ( 16.26562500061451289, 3.027376345333611329, 5.243569643749999010 ) ) ;
#55219 = CARTESIAN_POINT ( 'NONE',  ( 25.69687500061451502, 5.492252693125287522, 3.363034840372157021E-16 ) ) ;
#55220 = CARTESIAN_POINT ( 'NONE',  ( 15.00000000000000000, 4.330127018922192761, -2.499999999999997780 ) ) ;
#55221 = CARTESIAN_POINT ( 'NONE',  ( 12.15000000122903501, -2.886751345948129988, 4.999999999999997335 ) ) ;
#55222 = AXIS2_PLACEMENT_3D ( 'NONE', #16573, #61640, #43945 ) ;
#55223 = CARTESIAN_POINT ( 'NONE',  ( 7.903125000614515727, -4.541064518000417216, -2.621784821875001281 ) ) ;
#55224 = CARTESIAN_POINT ( 'NONE',  ( 10.82812500061451644, 4.541064518000418104, 2.621784821874999949 ) ) ;
#55225 = CARTESIAN_POINT ( 'NONE',  ( 20.40000000122903145, -2.886751345948125991, -5.000000000000000000 ) ) ;
#55226 = CARTESIAN_POINT ( 'NONE',  ( -4.243569643749997233, 14.04687500061451999, -27.54997392385601174 ) ) ;
#55227 = CARTESIAN_POINT ( 'NONE',  ( 20.25937500061451857, 4.541064518000418104, -2.621784821874998173 ) ) ;
#55228 = CARTESIAN_POINT ( 'NONE',  ( 21.44999999999999929, 0.000000000000000000, 4.999999999999998224 ) ) ;
#55229 = CARTESIAN_POINT ( 'NONE',  ( 5.325000001229033941, 2.886751345948126879, 4.999999999999999112 ) ) ;
#55230 = CARTESIAN_POINT ( 'NONE',  ( 3.234375000614516438, 4.541064518000418104, 2.621784821874999949 ) ) ;
#55231 = CARTESIAN_POINT ( 'NONE',  ( 20.82187500061451857, 3.027376345333611329, 5.243569643749999010 ) ) ;
#55232 = CARTESIAN_POINT ( 'NONE',  ( 7.320879633048903241E-15, 18.53750000000000142, 26.00000000000000355 ) ) ;
#55233 = CARTESIAN_POINT ( 'NONE',  ( 18.36562500061451431, 3.027376345333613106, -5.243569643749998122 ) ) ;
#55234 = CARTESIAN_POINT ( 'NONE',  ( 11.38125000122903252, 6.123233995736764310E-16, -4.999999999999998224 ) ) ;
#55235 = CARTESIAN_POINT ( 'NONE',  ( 7.950000000000001954, 0.000000000000000000, 4.999999999999998224 ) ) ;
#55236 = CARTESIAN_POINT ( 'NONE',  ( 26.84999999999999787, 0.000000000000000000, 4.999999999999998224 ) ) ;
#55237 = CARTESIAN_POINT ( 'NONE',  ( 29.67187500061451644, 3.027376345333613106, -5.243569643749998122 ) ) ;
#55238 = CARTESIAN_POINT ( 'NONE',  ( 20.52187500061451786, 5.824947211148865298E-16, -4.756430356249998326 ) ) ;
#55239 = CARTESIAN_POINT ( 'NONE',  ( 15.40312500061451573, 0.000000000000000000, 5.243569643749999010 ) ) ;
#55240 = CARTESIAN_POINT ( 'NONE',  ( 12.42187500061451821, -6.054752690667223547, -1.112240025338166033E-15 ) ) ;
#55241 = ORIENTED_EDGE ( 'NONE', *, *, #16377, .T. ) ;
#55242 = CARTESIAN_POINT ( 'NONE',  ( 4.000000000000000000, 17.03750000000000142, -27.69059892324149885 ) ) ;
#55243 = CARTESIAN_POINT ( 'NONE',  ( 22.22812500061451502, -4.541064518000419881, 2.621784821874995952 ) ) ;
#55244 = LINE ( 'NONE', #26063, #20342 ) ;
#55245 = LINE ( 'NONE', #26804, #18292 ) ;
#55246 = CARTESIAN_POINT ( 'NONE',  ( 12.33750000000000036, 5.773502691896255534, 3.535250795749688894E-16 ) ) ;
#55247 = CARTESIAN_POINT ( 'NONE',  ( 23.81250000122903288, 0.000000000000000000, 4.999999999999998224 ) ) ;
#55248 = CARTESIAN_POINT ( 'NONE',  ( 19.37812500061451715, 4.541064518000418104, 2.621784821874999949 ) ) ;
#55249 = ORIENTED_EDGE ( 'NONE', *, *, #64836, .T. ) ;
#55250 = CARTESIAN_POINT ( 'NONE',  ( 23.43750000000000000, -2.886751345948125991, -5.000000000000000000 ) ) ;
#55251 = CARTESIAN_POINT ( 'NONE',  ( 24.90937500061451715, 0.000000000000000000, 5.243569643749999010 ) ) ;
#55252 = ORIENTED_EDGE ( 'NONE', *, *, #10225, .F. ) ;
#55253 = CARTESIAN_POINT ( 'NONE',  ( 7.320879633048903241E-15, 18.08749999999999858, -34.00000000000000000 ) ) ;
#55254 = CARTESIAN_POINT ( 'NONE',  ( 11.57812500061451644, 6.421520780324663323E-16, -5.243569643749999010 ) ) ;
#55255 = CARTESIAN_POINT ( 'NONE',  ( 3.288170700621412479, 3.766687330211323737, 3.553104967622100929 ) ) ;
#55256 = CARTESIAN_POINT ( 'NONE',  ( 15.04687500061451466, -4.119189519843965641, -2.378215178125001383 ) ) ;
#55257 = CARTESIAN_POINT ( 'NONE',  ( 17.81250000000000355, 2.886751345948126879, 4.999999999999999112 ) ) ;
#55258 = CARTESIAN_POINT ( 'NONE',  ( 24.33749999999999858, -2.886751345948125991, -5.000000000000000000 ) ) ;
#55259 = CARTESIAN_POINT ( 'NONE',  ( -4.243569643749999898, 18.90312500061451573, 30.00000000000000000 ) ) ;
#55260 = CARTESIAN_POINT ( 'NONE',  ( 4.959375000614516971, 4.541064518000418104, -2.621784821874998173 ) ) ;
#55261 = CARTESIAN_POINT ( 'NONE',  ( 29.59687500061451715, -3.027376345333610441, -5.243569643749999898 ) ) ;
#55262 = EDGE_LOOP ( 'NONE', ( #12432, #55111, #14246, #32621 ) ) ;
#55263 = CARTESIAN_POINT ( 'NONE',  ( 25.19062500061451715, 6.054752690667223547, 3.707466751127219781E-16 ) ) ;
#55264 = CARTESIAN_POINT ( 'NONE',  ( 27.00937500061451857, 4.541064518000418104, -2.621784821874998173 ) ) ;
#55265 = DIRECTION ( 'NONE',  ( -1.000000000000000000, -0.000000000000000000, -0.000000000000000000 ) ) ;
#55266 = CARTESIAN_POINT ( 'NONE',  ( 13.64999999999999858, 4.330127018922192761, -2.499999999999997780 ) ) ;
#55267 = CARTESIAN_POINT ( 'NONE',  ( 11.05312500061451608, -4.541064518000417216, -2.621784821875001281 ) ) ;
#55268 = FACE_OUTER_BOUND ( 'NONE', #19935, .T. ) ;
#55269 = CARTESIAN_POINT ( 'NONE',  ( 4.000000000000000000, 19.28749999999999787, -27.69059892324149885 ) ) ;
#55270 = CARTESIAN_POINT ( 'NONE',  ( 28.07812500061451289, -4.541064518000419881, 2.621784821874995952 ) ) ;
#55271 = CARTESIAN_POINT ( 'NONE',  ( 15.60000000122903607, 5.773502691896255534, 3.535250795749688894E-16 ) ) ;
#55272 = CARTESIAN_POINT ( 'NONE',  ( 29.25937500061451502, 2.746126346562643317, 4.756430356249998326 ) ) ;
#55273 = CARTESIAN_POINT ( 'NONE',  ( 16.39687500061451786, -2.746126346562646425, 4.756430356249996549 ) ) ;
#55274 = CARTESIAN_POINT ( 'NONE',  ( 6.403125000614517504, 0.000000000000000000, 5.243569643749999010 ) ) ;
#55275 = CARTESIAN_POINT ( 'NONE',  ( 22.95937500061451431, 4.541064518000418104, -2.621784821874998173 ) ) ;
#55276 = CARTESIAN_POINT ( 'NONE',  ( -3.000416591977282496E-16, 14.79687500061451821, 25.09994784771203058 ) ) ;
#55277 = CARTESIAN_POINT ( 'NONE',  ( 22.09687500061451715, 6.054752690667223547, 3.707466751127219781E-16 ) ) ;
#55278 = CARTESIAN_POINT ( 'NONE',  ( 29.07187500061451502, -6.054752690667223547, -1.112240025338166033E-15 ) ) ;
#55279 = CARTESIAN_POINT ( 'NONE',  ( -4.243569643749999898, 18.05937500061451928, 30.00000000000000000 ) ) ;
#55280 = CARTESIAN_POINT ( 'NONE',  ( 9.215625000614515727, -6.054752690667223547, -1.112240025338166033E-15 ) ) ;
#55281 = CARTESIAN_POINT ( 'NONE',  ( 2.850000001229036073, -2.886751345948125991, -5.000000000000000000 ) ) ;
#55282 = EDGE_CURVE ( 'NONE', #39309, #11494, #15228, .T. ) ;
#55283 = CARTESIAN_POINT ( 'NONE',  ( 7.134375000614516793, 6.421520780324663323E-16, -5.243569643749999010 ) ) ;
#55284 = CARTESIAN_POINT ( 'NONE',  ( 7.575000001229033053, 2.886751345948126879, 4.999999999999998224 ) ) ;
#55285 = CARTESIAN_POINT ( 'NONE',  ( 10.49062500061451431, -3.027376345333614438, 5.243569643749998122 ) ) ;
#55286 = CARTESIAN_POINT ( 'NONE',  ( 14.82187500061451679, 3.027376345333613106, -5.243569643749998122 ) ) ;
#55287 = DIRECTION ( 'NONE',  ( -1.000000000000000000, -0.000000000000000000, -0.000000000000000000 ) ) ;
#55288 = CARTESIAN_POINT ( 'NONE',  ( 22.08750000122903501, -4.330127018922194537, 2.499999999999995559 ) ) ;
#55289 = CARTESIAN_POINT ( 'NONE',  ( 6.946875000614517681, -3.027376345333614438, 5.243569643749998122 ) ) ;
#55290 = CARTESIAN_POINT ( 'NONE',  ( 9.778125000614517504, 6.421520780324663323E-16, -5.243569643749999010 ) ) ;
#55291 = CARTESIAN_POINT ( 'NONE',  ( 26.94375000122903074, -2.886751345948129988, 4.999999999999997335 ) ) ;
#55292 = CARTESIAN_POINT ( 'NONE',  ( 19.17187500061451999, -6.054752690667223547, -1.112240025338166033E-15 ) ) ;
#55293 = FACE_BOUND ( 'NONE', #55756, .T. ) ;
#55294 = CARTESIAN_POINT ( 'NONE',  ( -0.5524690355592152269, 4.971316854763021986, 33.96409715941054230 ) ) ;
#55295 = CARTESIAN_POINT ( 'NONE',  ( 29.33437500061451431, 4.541064518000418104, 2.621784821874999949 ) ) ;
#55296 = CARTESIAN_POINT ( 'NONE',  ( -2.121784821874996840, 10.93437500061451928, -26.32496088578401583 ) ) ;
#55297 = CARTESIAN_POINT ( 'NONE',  ( 16.23750000122903359, -4.330127018922194537, 2.499999999999995559 ) ) ;
#55298 = CARTESIAN_POINT ( 'NONE',  ( -4.243569643749999898, 15.75312500061451537, -30.00000000000000000 ) ) ;
#55299 = CARTESIAN_POINT ( 'NONE',  ( 15.86250000122903181, -4.330127018922190985, -2.500000000000001332 ) ) ;
#55300 = CARTESIAN_POINT ( 'NONE',  ( 11.16562500061451679, 3.027376345333613106, -5.243569643749998122 ) ) ;
#55301 = EDGE_LOOP ( 'NONE', ( #26664, #47561, #42784, #38828 ) ) ;
#55302 = CARTESIAN_POINT ( 'NONE',  ( 12.93750000000000178, -2.886751345948129988, 4.999999999999997335 ) ) ;
#55303 = CARTESIAN_POINT ( 'NONE',  ( 10.40625000122903288, -4.330127018922190985, -2.500000000000001332 ) ) ;
#55304 = CARTESIAN_POINT ( 'NONE',  ( 22.04062500061451502, 6.054752690667223547, 3.707466751127219781E-16 ) ) ;
#55305 = CARTESIAN_POINT ( 'NONE',  ( 9.871875000614517504, 3.027376345333612662, -5.243569643749998122 ) ) ;
#55306 = LINE ( 'NONE', #9505, #24393 ) ;
#55307 = CARTESIAN_POINT ( 'NONE',  ( 9.037500001229034297, -4.330127018922194537, 2.499999999999995559 ) ) ;
#55308 = CARTESIAN_POINT ( 'NONE',  ( 18.37500000122903288, 2.886751345948126879, 4.999999999999999112 ) ) ;
#55309 = CARTESIAN_POINT ( 'NONE',  ( 16.19062500061451715, 6.054752690667223547, 3.707466751127219781E-16 ) ) ;
#55310 = CARTESIAN_POINT ( 'NONE',  ( 19.30312500061451786, 4.541064518000418104, -2.621784821874998173 ) ) ;
#55311 = CARTESIAN_POINT ( 'NONE',  ( 25.01250000122903216, 4.330127018922192761, -2.499999999999997780 ) ) ;
#55312 = CARTESIAN_POINT ( 'NONE',  ( 28.16250000122903074, 4.330127018922192761, -2.499999999999997780 ) ) ;
#55313 = CARTESIAN_POINT ( 'NONE',  ( 22.23750000000000071, 5.773502691896255534, 3.535250795749688894E-16 ) ) ;
#55314 = CARTESIAN_POINT ( 'NONE',  ( 1.878215178125000495, 13.16562499938548392, 26.74683588394047007 ) ) ;
#55315 = CARTESIAN_POINT ( 'NONE',  ( 25.99687500061451928, -3.027376345333610441, -5.243569643749999898 ) ) ;
#55316 = CARTESIAN_POINT ( 'NONE',  ( 1.999999999999998668, 12.65000000000000213, -33.46410161513775705 ) ) ;
#55317 = CARTESIAN_POINT ( 'NONE',  ( 11.58750000122903501, 4.330127018922191873, 2.499999999999999556 ) ) ;
#55318 = CARTESIAN_POINT ( 'NONE',  ( 28.50937500061451502, 0.000000000000000000, 5.243569643749999010 ) ) ;
#55319 = CARTESIAN_POINT ( 'NONE',  ( 12.56250000000000000, -5.773502691896255534, -1.060575238724906372E-15 ) ) ;
#55320 = CARTESIAN_POINT ( 'NONE',  ( 5.934375000614517504, 4.541064518000418104, 2.621784821874999949 ) ) ;
#55321 = CARTESIAN_POINT ( 'NONE',  ( 25.90312500061451573, -4.541064518000417216, -2.621784821875001281 ) ) ;
#55322 = CARTESIAN_POINT ( 'NONE',  ( 2.655984681222220721E-16, 15.56562499938548250, 25.66244784525396483 ) ) ;
#55323 = CARTESIAN_POINT ( 'NONE',  ( 4.661467738957717266, -1.808512791952580301, -4.661467738957749241 ) ) ;
#55324 = CARTESIAN_POINT ( 'NONE',  ( 11.14687500061451608, -3.027376345333610441, -5.243569643749999898 ) ) ;
#55325 = CARTESIAN_POINT ( 'NONE',  ( 22.12500000122903288, -5.773502691896255534, -1.060575238724906372E-15 ) ) ;
#55326 = CARTESIAN_POINT ( 'NONE',  ( 4.021875000614516082, 3.027376345333613106, -5.243569643749998122 ) ) ;
#55327 = CARTESIAN_POINT ( 'NONE',  ( 7.846875000614518036, -3.027376345333614438, 5.243569643749998122 ) ) ;
#55328 = CARTESIAN_POINT ( 'NONE',  ( 28.47187500061451715, 3.027376345333611329, 5.243569643749999010 ) ) ;
#55329 = CARTESIAN_POINT ( 'NONE',  ( -2.121784821874996840, 11.77812500061459566, 33.67503911421598417 ) ) ;
#55330 = CARTESIAN_POINT ( 'NONE',  ( 19.61249999999999716, 2.886751345948126879, 4.999999999999999112 ) ) ;
#55331 = ORIENTED_EDGE ( 'NONE', *, *, #51411, .T. ) ;
#55332 = CARTESIAN_POINT ( 'NONE',  ( 29.58749999999999858, -2.886751345948129988, 4.999999999999997335 ) ) ;
#55333 = CARTESIAN_POINT ( 'NONE',  ( 3.787500000000002753, 5.773502691896255534, 3.535250795749688894E-16 ) ) ;
#55334 = VERTEX_POINT ( 'NONE', #37866 ) ;
#55335 = CARTESIAN_POINT ( 'NONE',  ( 18.21562500061451573, -6.054752690667223547, -1.112240025338166033E-15 ) ) ;
#55336 = CARTESIAN_POINT ( 'NONE',  ( 9.365625000614519635, 3.027376345333613106, -5.243569643749998122 ) ) ;
#55337 = CARTESIAN_POINT ( 'NONE',  ( 21.79687500061451644, -4.119189519843965641, -2.378215178125001383 ) ) ;
#55338 = CARTESIAN_POINT ( 'NONE',  ( 7.546875000614517326, -3.027376345333610441, -5.243569643749999898 ) ) ;
#55339 = CARTESIAN_POINT ( 'NONE',  ( 16.72500000122903430, -5.773502691896255534, -1.060575238724906372E-15 ) ) ;
#55340 = LINE ( 'NONE', #27269, #52728 ) ;
#55341 = CARTESIAN_POINT ( 'NONE',  ( 7.584375000614516082, 6.421520780324663323E-16, -5.243569643749999010 ) ) ;
#55342 = CARTESIAN_POINT ( 'NONE',  ( 11.59687500061451892, -3.027376345333610441, -5.243569643749999898 ) ) ;
#55343 = CARTESIAN_POINT ( 'NONE',  ( 25.32187500061451857, 3.027376345333611329, 5.243569643749999010 ) ) ;
#55344 = ADVANCED_FACE ( 'NONE', ( #60385 ), #58922, .F. ) ;
#55345 = CARTESIAN_POINT ( 'NONE',  ( 26.69999999999999929, 4.330127018922192761, -2.499999999999997780 ) ) ;
#55346 = EDGE_LOOP ( 'NONE', ( #14488, #26726, #37379 ) ) ;
#55347 = CARTESIAN_POINT ( 'NONE',  ( 11.13750000000000284, -2.886751345948129988, 4.999999999999997335 ) ) ;
#55348 = CARTESIAN_POINT ( 'NONE',  ( 17.52187500061451431, 3.027376345333613106, -5.243569643749998122 ) ) ;
#55349 = CARTESIAN_POINT ( 'NONE',  ( 10.54687500061451644, -3.027376345333614438, 5.243569643749998122 ) ) ;
#55350 = CARTESIAN_POINT ( 'NONE',  ( 3.756430356250000102, 15.79062499938548392, 30.00000000000000000 ) ) ;
#55351 = CARTESIAN_POINT ( 'NONE',  ( 20.40000000000000213, 4.330127018922192761, -2.499999999999997780 ) ) ;
#55352 = CARTESIAN_POINT ( 'NONE',  ( -1.999999999999999112, 16.25000000000000000, 26.53589838486224650 ) ) ;
#55353 = CARTESIAN_POINT ( 'NONE',  ( 2.121784821874999061, 10.25937500061451857, -33.67503911421598417 ) ) ;
#55354 = CARTESIAN_POINT ( 'NONE',  ( 22.35937500061451644, -4.119189519843965641, -2.378215178125001383 ) ) ;
#55355 = CARTESIAN_POINT ( 'NONE',  ( 13.26562500061451644, -6.054752690667223547, -1.112240025338166033E-15 ) ) ;
#55356 = CARTESIAN_POINT ( 'NONE',  ( 29.74687500061451217, 6.054752690667223547, 3.707466751127219781E-16 ) ) ;
#55357 = CARTESIAN_POINT ( 'NONE',  ( -2.000000000000000000, 19.13750000122903216, -33.46410161513775705 ) ) ;
#55358 = CARTESIAN_POINT ( 'NONE',  ( 4.241277253184729368, 2.648812835464926518, -4.241277253184729368 ) ) ;
#55359 = CARTESIAN_POINT ( 'NONE',  ( 9.487500000000000711, -2.886751345948125991, -5.000000000000000000 ) ) ;
#55360 = CARTESIAN_POINT ( 'NONE',  ( 3.999999999999998668, 15.42500000122903359, 27.69059892324149175 ) ) ;
#55362 =( BOUNDED_CURVE ( )  B_SPLINE_CURVE ( 2, ( #62527, #29280, #11571, #11924, #51091, #51810, #67722 ),
 .UNSPECIFIED., .F., .F. ) 
 B_SPLINE_CURVE_WITH_KNOTS ( ( 3, 2, 2, 3 ),
 ( 0.2000000000000000389, 0.2033333333333333659, 0.2066666666666667207, 0.2100000000000000477 ),
 .UNSPECIFIED. ) 
 CURVE ( )  GEOMETRIC_REPRESENTATION_ITEM ( )  RATIONAL_B_SPLINE_CURVE ( ( 0.9999999999999988898, 0.8660254037844398178, 1.000000000000000000, 0.8660254037844387076, 1.000000000000000000, 0.8660254037844364872, 1.000000000000002220 ) ) 
 REPRESENTATION_ITEM ( '' )  );
#55361 = CARTESIAN_POINT ( 'NONE',  ( 9.000000001229034652, -2.886751345948129988, 4.999999999999997335 ) ) ;
#55363 = CARTESIAN_POINT ( 'NONE',  ( 19.32187500061451857, 3.027376345333613106, -5.243569643749998122 ) ) ;
#55364 = CARTESIAN_POINT ( 'NONE',  ( 13.58437500061451786, 4.541064518000418104, 2.621784821874999949 ) ) ;
#55365 = CARTESIAN_POINT ( 'NONE',  ( 2.000000000000001332, 16.66250000122903430, 33.46410161513774995 ) ) ;
#55366 = VERTEX_POINT ( 'NONE', #54863 ) ;
#55367 = CARTESIAN_POINT ( 'NONE',  ( 18.25312500061451715, -4.541064518000417216, -2.621784821875001281 ) ) ;
#55368 = CARTESIAN_POINT ( 'NONE',  ( 29.32500000122903216, -5.773502691896255534, -1.060575238724906372E-15 ) ) ;
#55369 = CARTESIAN_POINT ( 'NONE',  ( 15.27187500061451786, 3.027376345333613106, -5.243569643749998122 ) ) ;
#55370 = CARTESIAN_POINT ( 'NONE',  ( 0.8036833610285047946, 9.975469519845873378, -24.04062768261224647 ) ) ;
#55371 = CARTESIAN_POINT ( 'NONE',  ( 16.19062500061451715, 6.054752690667223547, 3.707466751127219781E-16 ) ) ;
#55372 = CARTESIAN_POINT ( 'NONE',  ( 18.41249999999999787, -5.773502691896255534, -1.060575238724906372E-15 ) ) ;
#55373 = CARTESIAN_POINT ( 'NONE',  ( 9.001249775931846008E-16, 11.81562500061451715, 34.90005215228797653 ) ) ;
#55374 = CARTESIAN_POINT ( 'NONE',  ( 18.49687500061452283, 6.054752690667223547, 3.707466751127219781E-16 ) ) ;
#55375 = CARTESIAN_POINT ( 'NONE',  ( 14.13750000122903394, 6.123233995736764310E-16, -4.999999999999998224 ) ) ;
#55376 = CARTESIAN_POINT ( 'NONE',  ( 9.646875000614519635, -2.746126346562646425, 4.756430356249996549 ) ) ;
#55377 = CARTESIAN_POINT ( 'NONE',  ( -3.000416591977282496E-16, 18.84687500061451360, -34.90005215228797653 ) ) ;
#55378 = CARTESIAN_POINT ( 'NONE',  ( 19.69687500061451857, -3.027376345333610441, -5.243569643749999898 ) ) ;
#55379 = CARTESIAN_POINT ( 'NONE',  ( 21.30000000122903359, -2.886751345948125991, -5.000000000000000000 ) ) ;
#55380 = CARTESIAN_POINT ( 'NONE',  ( 17.40937500061451715, -4.541064518000417216, -2.621784821875001281 ) ) ;
#55381 = CARTESIAN_POINT ( 'NONE',  ( 12.92812500061451786, 6.421520780324663323E-16, -5.243569643749999010 ) ) ;
#55382 = CARTESIAN_POINT ( 'NONE',  ( 9.001249775931846008E-16, 12.77187500061451786, 34.90005215228797653 ) ) ;
#55383 = CARTESIAN_POINT ( 'NONE',  ( 18.59062500061451573, -3.027376345333614438, 5.243569643749998122 ) ) ;
#55384 = ORIENTED_EDGE ( 'NONE', *, *, #4790, .T. ) ;
#55385 = VERTEX_POINT ( 'NONE', #20492 ) ;
#55386 = CARTESIAN_POINT ( 'NONE',  ( 19.46249999999999858, 2.886751345948129099, -4.999999999999998224 ) ) ;
#55387 = DIRECTION ( 'NONE',  ( 0.000000000000000000, 0.000000000000000000, -1.000000000000000000 ) ) ;
#55388 = CARTESIAN_POINT ( 'NONE',  ( 24.51562500061451289, -6.054752690667223547, -1.112240025338166033E-15 ) ) ;
#55389 = CARTESIAN_POINT ( 'NONE',  ( 5.990625000614517859, -3.027376345333614438, 5.243569643749998122 ) ) ;
#55390 = CARTESIAN_POINT ( 'NONE',  ( 17.17500000122903359, -5.773502691896255534, -1.060575238724906372E-15 ) ) ;
#55391 = CARTESIAN_POINT ( 'NONE',  ( 23.01562500061451644, 3.027376345333611329, 5.243569643749999010 ) ) ;
#55392 = CARTESIAN_POINT ( 'NONE',  ( 22.38749999999999929, -2.886751345948129988, 4.999999999999997335 ) ) ;
#55393 = CARTESIAN_POINT ( 'NONE',  ( 26.09062500061451573, 6.054752690667223547, 3.707466751127219781E-16 ) ) ;
#55394 = CARTESIAN_POINT ( 'NONE',  ( 6.590625000614518392, -3.027376345333610441, -5.243569643749999898 ) ) ;
#55395 = ORIENTED_EDGE ( 'NONE', *, *, #71031, .T. ) ;
#55396 = CARTESIAN_POINT ( 'NONE',  ( 26.73750000122903003, 6.123233995736764310E-16, -4.999999999999998224 ) ) ;
#55397 = CARTESIAN_POINT ( 'NONE',  ( 3.253125000614518036, 0.000000000000000000, 5.243569643749999010 ) ) ;
#55398 = CARTESIAN_POINT ( 'NONE',  ( 11.03437500061451715, -4.119189519843968306, 2.378215178124996054 ) ) ;
#55399 = CARTESIAN_POINT ( 'NONE',  ( -3.137519842735245283E-14, 12.91250000000000142, 34.00000000000000000 ) ) ;
#55400 = B_SPLINE_CURVE_WITH_KNOTS ( 'NONE', 3,
 ( #54958, #48687, #4363, #71951, #60852, #43880, #10618, #72311, #66406, #15782 ),
 .UNSPECIFIED., .F., .F.,
 ( 4, 3, 3, 4 ),
 ( 9.758590510124697839E-17, 0.0001554715923351995962, 0.0002333273007130473695, 0.0003112188215848752607 ),
 .UNSPECIFIED. ) ;
#55401 = CARTESIAN_POINT ( 'NONE',  ( -3.999999999999999556, 14.22500000122903430, -32.30940107675850470 ) ) ;
#55402 = CARTESIAN_POINT ( 'NONE',  ( 4.243569643749999898, 17.83437500061451786, -30.00000000000000000 ) ) ;
#55403 = CARTESIAN_POINT ( 'NONE',  ( 9.975000000000001421, 6.123233995736764310E-16, -4.999999999999998224 ) ) ;
#55404 = EDGE_CURVE ( 'NONE', #58120, #4995, #43071, .T. ) ;
#55405 = CARTESIAN_POINT ( 'NONE',  ( 12.08437500061451608, 6.421520780324663323E-16, -5.243569643749999010 ) ) ;
#55406 = CARTESIAN_POINT ( 'NONE',  ( 7.275000001229035007, -5.773502691896255534, -1.060575238724906372E-15 ) ) ;
#55407 = CARTESIAN_POINT ( 'NONE',  ( 12.38437500061451857, -4.541064518000419881, 2.621784821874995952 ) ) ;
#55408 = CARTESIAN_POINT ( 'NONE',  ( 4.809375000614516615, -4.541064518000417216, -2.621784821875001281 ) ) ;
#55409 = CARTESIAN_POINT ( 'NONE',  ( -4.243569643749999898, 10.35312500061451857, -30.00000000000000000 ) ) ;
#55410 = DIRECTION ( 'NONE',  ( -0.000000000000000000, -1.000000000000000000, -0.000000000000000000 ) ) ;
#55412 = ADVANCED_FACE ( 'NONE', ( #42318 ), #64844, .T. ) ;
#55411 = CARTESIAN_POINT ( 'NONE',  ( 10.50937500061451679, 0.000000000000000000, 5.243569643749999010 ) ) ;
#55413 = CARTESIAN_POINT ( 'NONE',  ( 0.000000000000000000, 20.00000000000000000, 26.00000000000000000 ) ) ;
#55414 = CARTESIAN_POINT ( 'NONE',  ( 18.55312500061451431, 0.000000000000000000, 5.243569643749999010 ) ) ;
#55415 = CARTESIAN_POINT ( 'NONE',  ( 16.50000000000000000, 0.000000000000000000, 4.999999999999998224 ) ) ;
#55416 = CARTESIAN_POINT ( 'NONE',  ( 4.243569643749999010, 19.16562500061459673, 27.54997392385601174 ) ) ;
#55417 = CARTESIAN_POINT ( 'NONE',  ( 24.00937500061451502, 0.000000000000000000, 5.243569643749999010 ) ) ;
#55418 = EDGE_CURVE ( 'NONE', #8622, #38892, #70752, .T. ) ;
#55419 = CARTESIAN_POINT ( 'NONE',  ( 4.070823519296731696, 2.903409097154723284, -4.275654497055423775 ) ) ;
#55420 = CARTESIAN_POINT ( 'NONE',  ( 28.38750000122903216, -4.330127018922194537, 2.499999999999995559 ) ) ;
#55421 = CARTESIAN_POINT ( 'NONE',  ( 19.17187500061451289, 5.824947211148865298E-16, -4.756430356249998326 ) ) ;
#55422 = CARTESIAN_POINT ( 'NONE',  ( 24.40312500061451573, 0.000000000000000000, 5.243569643749999010 ) ) ;
#55423 = CARTESIAN_POINT ( 'NONE',  ( 16.90312500061451573, -4.541064518000417216, -2.621784821875001281 ) ) ;
#55424 = CARTESIAN_POINT ( 'NONE',  ( 13.40625000122903288, 0.000000000000000000, 4.999999999999998224 ) ) ;
#55425 = CARTESIAN_POINT ( 'NONE',  ( 13.77187500061451786, -6.054752690667223547, -1.112240025338166033E-15 ) ) ;
#55426 = CARTESIAN_POINT ( 'NONE',  ( 1.138803498474273873E-14, 15.98750000000000249, 34.00000000000000000 ) ) ;
#55427 = CARTESIAN_POINT ( 'NONE',  ( 26.58750000122903145, -4.330127018922194537, 2.499999999999995559 ) ) ;
#55428 = CARTESIAN_POINT ( 'NONE',  ( 3.796875000614517326, -3.027376345333614438, 5.243569643749998122 ) ) ;
#55429 = CARTESIAN_POINT ( 'NONE',  ( 14.63437500061451679, -4.541064518000419881, 2.621784821874995952 ) ) ;
#55430 = CARTESIAN_POINT ( 'NONE',  ( 1.626862140677534273E-15, 12.01250000000000284, 34.00000000000000000 ) ) ;
#55431 = CARTESIAN_POINT ( 'NONE',  ( -3.999999999999997335, 11.48750000000000071, 32.30940107675850470 ) ) ;
#55432 = CARTESIAN_POINT ( 'NONE',  ( 4.312500001229034652, 4.330127018922192761, -2.499999999999997780 ) ) ;
#55433 = CARTESIAN_POINT ( 'NONE',  ( 23.82187500061451502, 3.027376345333613106, -5.243569643749998122 ) ) ;
#55434 = CARTESIAN_POINT ( 'NONE',  ( 17.37187500061451573, -6.054752690667223547, -1.112240025338166033E-15 ) ) ;
#55435 = CARTESIAN_POINT ( 'NONE',  ( 2.655984681222220721E-16, 16.46562499938548285, 25.66244784525396483 ) ) ;
#55436 = CARTESIAN_POINT ( 'NONE',  ( 27.52500000000000213, 6.123233995736764310E-16, -4.999999999999998224 ) ) ;
#55437 = CYLINDRICAL_SURFACE ( 'NONE', #13606, 4.000000000000000000 ) ;
#55438 = CARTESIAN_POINT ( 'NONE',  ( 6.712500000000000355, -5.773502691896255534, -1.060575238724906372E-15 ) ) ;
#55439 = CARTESIAN_POINT ( 'NONE',  ( 7.846875000614515372, -4.119189519843965641, -2.378215178125001383 ) ) ;
#55440 = CARTESIAN_POINT ( 'NONE',  ( 19.34062500061451573, 6.054752690667223547, 3.707466751127219781E-16 ) ) ;
#55441 = CARTESIAN_POINT ( 'NONE',  ( 10.49999999999999822, 4.330127018922192761, -2.499999999999997780 ) ) ;
#55442 = CARTESIAN_POINT ( 'NONE',  ( 4.603125000614518569, 0.000000000000000000, 5.243569643749999010 ) ) ;
#55443 = CARTESIAN_POINT ( 'NONE',  ( 17.88749999999999929, -2.886751345948129988, 4.999999999999997335 ) ) ;
#55444 = CARTESIAN_POINT ( 'NONE',  ( 21.52500000122903145, 2.886751345948126879, 4.999999999999999112 ) ) ;
#55445 = CARTESIAN_POINT ( 'NONE',  ( -2.000000000000000000, 10.02500000000000036, -33.46410161513775705 ) ) ;
#55446 = CARTESIAN_POINT ( 'NONE',  ( 28.99687500061451573, -3.027376345333614438, 5.243569643749998122 ) ) ;
#55447 = VERTEX_POINT ( 'NONE', #8695 ) ;
#55448 = CARTESIAN_POINT ( 'NONE',  ( 17.50312500061451715, 4.541064518000418104, -2.621784821874998173 ) ) ;
#55449 = CARTESIAN_POINT ( 'NONE',  ( 25.34062500061451217, -3.027376345333614438, 5.243569643749998122 ) ) ;
#55450 = CARTESIAN_POINT ( 'NONE',  ( 23.33437500061451786, 6.421520780324663323E-16, -5.243569643749999010 ) ) ;
#55451 = CARTESIAN_POINT ( 'NONE',  ( 6.375000000000001776, 6.123233995736764310E-16, -4.999999999999998224 ) ) ;
#55452 = CARTESIAN_POINT ( 'NONE',  ( 8.503125000614515372, 4.541064518000418104, -2.621784821874998173 ) ) ;
#55453 = CARTESIAN_POINT ( 'NONE',  ( 27.70312500061451289, -4.541064518000417216, -2.621784821875001281 ) ) ;
#55454 = CARTESIAN_POINT ( 'NONE',  ( 14.37187500061451928, 3.027376345333613106, -5.243569643749998122 ) ) ;
#55455 = CARTESIAN_POINT ( 'NONE',  ( 18.45937500061451431, 4.541064518000418104, -2.621784821874998173 ) ) ;
#55456 = LINE ( 'NONE', #38837, #14444 ) ;
#55457 = CARTESIAN_POINT ( 'NONE',  ( -2.121784821874999949, 9.884375000614518569, 26.32496088578401938 ) ) ;
#55458 = EDGE_CURVE ( 'NONE', #44903, #22838, #31227, .T. ) ;
#55459 = CARTESIAN_POINT ( 'NONE',  ( 21.90000000122903145, 5.773502691896255534, 3.535250795749688894E-16 ) ) ;
#55460 = CARTESIAN_POINT ( 'NONE',  ( 17.37187500061451573, -5.492252693125287522, -1.008910452111647106E-15 ) ) ;
#55461 = CARTESIAN_POINT ( 'NONE',  ( 10.86562500061451608, 3.027376345333611329, 5.243569643749999010 ) ) ;
#55462 = CARTESIAN_POINT ( 'NONE',  ( 8.409375000614518925, -4.541064518000417216, -2.621784821875001281 ) ) ;
#55463 = CARTESIAN_POINT ( 'NONE',  ( 8.259375000614518569, 0.000000000000000000, 5.243569643749999010 ) ) ;
#55464 = VERTEX_POINT ( 'NONE', #41954 ) ;
#55465 = CARTESIAN_POINT ( 'NONE',  ( 28.77187500061451431, 3.027376345333613106, -5.243569643749998122 ) ) ;
#55466 = CARTESIAN_POINT ( 'NONE',  ( 18.32812500061451644, 6.421520780324663323E-16, -5.243569643749999010 ) ) ;
#55467 = CARTESIAN_POINT ( 'NONE',  ( 29.40000000122903145, -2.886751345948125991, -5.000000000000000000 ) ) ;
#55468 = CARTESIAN_POINT ( 'NONE',  ( 3.721875000614518036, 3.027376345333611329, 5.243569643749999010 ) ) ;
#55469 = CARTESIAN_POINT ( 'NONE',  ( 24.79687500061451999, 6.054752690667223547, 3.707466751127219781E-16 ) ) ;
#55470 = CARTESIAN_POINT ( 'NONE',  ( 20.05312500061451431, -4.541064518000417216, -2.621784821875001281 ) ) ;
#55471 = CARTESIAN_POINT ( 'NONE',  ( 9.001249775931846008E-16, 18.62187500061451928, 34.90005215228797653 ) ) ;
#55472 = CARTESIAN_POINT ( 'NONE',  ( 23.50312500061451360, 0.000000000000000000, 5.243569643749999010 ) ) ;
#55473 = CARTESIAN_POINT ( 'NONE',  ( 4.275000001229035895, 2.886751345948129099, -4.999999999999998224 ) ) ;
#55474 = VERTEX_POINT ( 'NONE', #37129 ) ;
#55475 = CARTESIAN_POINT ( 'NONE',  ( 27.26249999999999929, 2.886751345948126879, 4.999999999999999112 ) ) ;
#55476 = CARTESIAN_POINT ( 'NONE',  ( -3.999999999999997335, 16.43750000000000000, -27.69059892324149175 ) ) ;
#55477 = CARTESIAN_POINT ( 'NONE',  ( -3.756430356250001434, 17.06562499938548427, 32.16877607737301048 ) ) ;
#55478 = CARTESIAN_POINT ( 'NONE',  ( 4.171875000614517326, 3.027376345333611329, 5.243569643749999010 ) ) ;
#55479 = CARTESIAN_POINT ( 'NONE',  ( 11.84062500061451750, -3.027376345333614438, 5.243569643749998122 ) ) ;
#55480 = CARTESIAN_POINT ( 'NONE',  ( 5.446875000614518569, 6.054752690667223547, 3.707466751127219781E-16 ) ) ;
#55481 = CARTESIAN_POINT ( 'NONE',  ( 24.48750000122903359, 6.123233995736764310E-16, -4.999999999999998224 ) ) ;
#55482 = CARTESIAN_POINT ( 'NONE',  ( 15.27187500061451786, 3.027376345333612662, -5.243569643749998122 ) ) ;
#55483 = CARTESIAN_POINT ( 'NONE',  ( 3.646875000614520079, 6.054752690667223547, 3.707466751127219781E-16 ) ) ;
#55484 = LINE ( 'NONE', #38864, #41566 ) ;
#55485 = CARTESIAN_POINT ( 'NONE',  ( 25.65937500061451715, 4.541064518000418104, -2.621784821874998173 ) ) ;
#55486 = CARTESIAN_POINT ( 'NONE',  ( 12.59062500061451573, 6.054752690667223547, 3.707466751127219781E-16 ) ) ;
#55487 = ORIENTED_EDGE ( 'NONE', *, *, #13371, .F. ) ;
#55488 = CARTESIAN_POINT ( 'NONE',  ( 10.60312500061451679, -4.541064518000417216, -2.621784821875001281 ) ) ;
#55489 = CARTESIAN_POINT ( 'NONE',  ( 9.215625000614515727, -6.054752690667223547, -1.112240025338166033E-15 ) ) ;
#55490 = CARTESIAN_POINT ( 'NONE',  ( 18.12187500061451573, 2.746126346562643317, 4.756430356249998326 ) ) ;
#55491 = CARTESIAN_POINT ( 'NONE',  ( 8.737500000000002487, 5.773502691896255534, 3.535250795749688894E-16 ) ) ;
#55492 = CARTESIAN_POINT ( 'NONE',  ( 4.125000001229034652, -5.773502691896255534, -1.060575238724906372E-15 ) ) ;
#55493 = CARTESIAN_POINT ( 'NONE',  ( 17.13749999999999929, -2.886751345948125991, -5.000000000000000000 ) ) ;
#55494 = CARTESIAN_POINT ( 'NONE',  ( 18.08437500061451431, 4.541064518000418104, 2.621784821874999949 ) ) ;
#55495 = CARTESIAN_POINT ( 'NONE',  ( 12.97500000122903252, 2.886751345948126879, 4.999999999999999112 ) ) ;
#55496 = CARTESIAN_POINT ( 'NONE',  ( 20.58750000000000213, -2.886751345948129988, 4.999999999999997335 ) ) ;
#55497 = CARTESIAN_POINT ( 'NONE',  ( 2.121784821875001281, 15.45312500061451644, -26.32496088578401938 ) ) ;
#55498 = CARTESIAN_POINT ( 'NONE',  ( -2.000000000000001776, 20.00000000000000000, 33.46410161513775705 ) ) ;
#55499 = DIRECTION ( 'NONE',  ( 0.000000000000000000, 0.000000000000000000, 1.000000000000000000 ) ) ;
#55500 = CARTESIAN_POINT ( 'NONE',  ( 27.32812500061451644, 6.421520780324663323E-16, -5.243569643749999010 ) ) ;
#55501 = DIRECTION ( 'NONE',  ( 1.000000000000000000, 0.000000000000000000, -0.000000000000000000 ) ) ;
#55502 = CARTESIAN_POINT ( 'NONE',  ( 24.26249999999999929, -5.773502691896255534, -1.060575238724906372E-15 ) ) ;
#55503 = CARTESIAN_POINT ( 'NONE',  ( 14.82187500061451679, 3.027376345333613106, -5.243569643749998122 ) ) ;
#55504 =( BOUNDED_CURVE ( )  B_SPLINE_CURVE ( 2, ( #15772, #26138, #19854, #60841, #64927, #14317, #59369 ),
 .UNSPECIFIED., .F., .F. ) 
 B_SPLINE_CURVE_WITH_KNOTS ( ( 3, 2, 2, 3 ),
 ( 0.6750000000000000444, 0.6777777777777778123, 0.6805555555555555802, 0.6833333333333333481 ),
 .UNSPECIFIED. ) 
 CURVE ( )  GEOMETRIC_REPRESENTATION_ITEM ( )  RATIONAL_B_SPLINE_CURVE ( ( 1.000000000000000000, 0.8660254037844387076, 1.000000000000000000, 0.8660254037844387076, 1.000000000000000000, 0.8660254037844387076, 1.000000000000000000 ) ) 
 REPRESENTATION_ITEM ( '' )  );
#55505 = EDGE_CURVE ( 'NONE', #56216, #45736, #35649, .T. ) ;
#55506 = EDGE_CURVE ( 'NONE', #67424, #29801, #33287, .T. ) ;
#55507 = CARTESIAN_POINT ( 'NONE',  ( 25.94999999999999929, 0.000000000000000000, 4.999999999999998224 ) ) ;
#55508 = CARTESIAN_POINT ( 'NONE',  ( 9.553125000614517859, 0.000000000000000000, 5.243569643749999010 ) ) ;
#55509 = CARTESIAN_POINT ( 'NONE',  ( 28.43437500061451573, -2.746126346562646425, 4.756430356249996549 ) ) ;
#55510 = CARTESIAN_POINT ( 'NONE',  ( 20.82187500061451857, 3.027376345333611329, 5.243569643749999010 ) ) ;
#55511 = CARTESIAN_POINT ( 'NONE',  ( 14.44687500061451502, 0.000000000000000000, 4.756430356249998326 ) ) ;
#55512 = CARTESIAN_POINT ( 'NONE',  ( 7.640625000614517326, 6.054752690667223547, 3.707466751127219781E-16 ) ) ;
#55513 = CARTESIAN_POINT ( 'NONE',  ( 11.70937500061451608, 4.541064518000418104, -2.621784821874998173 ) ) ;
#55514 = ORIENTED_EDGE ( 'NONE', *, *, #11404, .T. ) ;
#55515 = CARTESIAN_POINT ( 'NONE',  ( 22.17187500061451644, 3.027376345333611329, 5.243569643749999010 ) ) ;
#55516 = CARTESIAN_POINT ( 'NONE',  ( 2.064291216241248783, 4.560108959200712242, -26.56427412444418579 ) ) ;
#55517 = CYLINDRICAL_SURFACE ( 'NONE', #30185, 4.999999999999998224 ) ;
#55518 = CARTESIAN_POINT ( 'NONE',  ( 4.275000000000001243, 4.330127018922191873, 2.499999999999999556 ) ) ;
#55519 = CARTESIAN_POINT ( 'NONE',  ( 15.45000000122903216, -2.886751345948125991, -5.000000000000000000 ) ) ;
#55520 = DIRECTION ( 'NONE',  ( -1.000000000000000000, -0.000000000000000000, -0.000000000000000000 ) ) ;
#55521 = CARTESIAN_POINT ( 'NONE',  ( 1.626862140677534273E-15, 11.67500000122903181, 34.00000000000000000 ) ) ;
#55522 = ORIENTED_EDGE ( 'NONE', *, *, #9642, .T. ) ;
#55523 = CARTESIAN_POINT ( 'NONE',  ( 11.96250000000000213, 2.886751345948126879, 4.999999999999999112 ) ) ;
#55524 = CARTESIAN_POINT ( 'NONE',  ( 16.57499999999999929, -4.330127018922194537, 2.499999999999995559 ) ) ;
#55525 = CARTESIAN_POINT ( 'NONE',  ( 13.38750000122903394, 4.330127018922191873, 2.499999999999999556 ) ) ;
#55526 = CARTESIAN_POINT ( 'NONE',  ( 10.41562500061451679, 3.027376345333611329, 5.243569643749999010 ) ) ;
#55527 = EDGE_LOOP ( 'NONE', ( #50444, #63794, #64156, #8699 ) ) ;
#55528 = CARTESIAN_POINT ( 'NONE',  ( 9.262499999999999289, 2.886751345948126879, 4.999999999999999112 ) ) ;
#55529 = CARTESIAN_POINT ( 'NONE',  ( -1.071796769724496556, 15.70490381179669903, 33.99999999999998579 ) ) ;
#55530 = CARTESIAN_POINT ( 'NONE',  ( 2.121784821874999061, 13.40937500061451892, -33.67503911421598417 ) ) ;
#55531 = CARTESIAN_POINT ( 'NONE',  ( 29.58750000122903501, 4.330127018922191873, 2.499999999999999556 ) ) ;
#55532 = CARTESIAN_POINT ( 'NONE',  ( -1.878215178125001827, 15.19062499938548427, 33.25316411605952283 ) ) ;
#55533 = CARTESIAN_POINT ( 'NONE',  ( 8.699999999999999289, 4.330127018922192761, -2.499999999999997780 ) ) ;
#55534 = VERTEX_POINT ( 'NONE', #67060 ) ;
#55535 = CARTESIAN_POINT ( 'NONE',  ( 24.47812500061451502, -4.541064518000419881, 2.621784821874995952 ) ) ;
#55536 = CARTESIAN_POINT ( 'NONE',  ( 1.999999999999998668, 13.55000000000000071, -33.46410161513775705 ) ) ;
#55537 = CARTESIAN_POINT ( 'NONE',  ( 29.70937500061451431, 4.541064518000418104, -2.621784821874998173 ) ) ;
#55538 = CARTESIAN_POINT ( 'NONE',  ( 22.47187500061451715, 3.027376345333613106, -5.243569643749998122 ) ) ;
#55539 = CARTESIAN_POINT ( 'NONE',  ( 17.61562500061451786, 3.027376345333611329, 5.243569643749999010 ) ) ;
#55540 = CARTESIAN_POINT ( 'NONE',  ( 4.243569643749999010, 11.96562500061459389, -32.45002607614398471 ) ) ;
#55541 = CARTESIAN_POINT ( 'NONE',  ( 6.628125000614517148, 6.421520780324663323E-16, -5.243569643749999010 ) ) ;
#55542 = CARTESIAN_POINT ( 'NONE',  ( 28.20000000122903216, 5.773502691896255534, 3.535250795749688894E-16 ) ) ;
#55543 = CARTESIAN_POINT ( 'NONE',  ( 25.13437500061451502, 5.824947211148865298E-16, -4.756430356249998326 ) ) ;
#55544 = CARTESIAN_POINT ( 'NONE',  ( 18.32812500061451644, 6.421520780324663323E-16, -5.243569643749999010 ) ) ;
#55545 = CARTESIAN_POINT ( 'NONE',  ( 7.959375000614516971, -4.119189519843965641, -2.378215178125001383 ) ) ;
#55546 = CARTESIAN_POINT ( 'NONE',  ( 2.655984681222220721E-16, 18.60312499938548214, 25.66244784525396483 ) ) ;
#55547 = CARTESIAN_POINT ( 'NONE',  ( 14.14687500061451786, -3.027376345333614438, 5.243569643749998122 ) ) ;
#55548 = CARTESIAN_POINT ( 'NONE',  ( 13.92187500061451644, 3.027376345333613106, -5.243569643749998122 ) ) ;
#55549 = CARTESIAN_POINT ( 'NONE',  ( 22.99687500061451573, 6.054752690667223547, 3.707466751127219781E-16 ) ) ;
#55550 = VERTEX_POINT ( 'NONE', #44527 ) ;
#55551 = CARTESIAN_POINT ( 'NONE',  ( -2.121784821874999949, 12.13437500061451857, 26.32496088578401938 ) ) ;
#55552 = CARTESIAN_POINT ( 'NONE',  ( 3.103125000614517237, 4.541064518000418104, -2.621784821874998173 ) ) ;
#55553 = CARTESIAN_POINT ( 'NONE',  ( 27.70312500061451289, -4.541064518000417216, -2.621784821875001281 ) ) ;
#55554 = CARTESIAN_POINT ( 'NONE',  ( 25.82812500061451644, -4.541064518000419881, 2.621784821874995952 ) ) ;
#55555 = CARTESIAN_POINT ( 'NONE',  ( 30.00000000000000000, 0.000000000000000000, 4.999999999999998224 ) ) ;
#55556 = CARTESIAN_POINT ( 'NONE',  ( -1.999999999999997113, 19.17500000000000071, 33.46410161513775705 ) ) ;
#55557 = CARTESIAN_POINT ( 'NONE',  ( 4.621875000614516615, 3.027376345333611329, 5.243569643749999010 ) ) ;
#55558 = CARTESIAN_POINT ( 'NONE',  ( 12.75000000122903643, -2.886751345948125991, -5.000000000000000000 ) ) ;
#55559 = CARTESIAN_POINT ( 'NONE',  ( 9.825000001229033941, 2.886751345948126879, 4.999999999999999112 ) ) ;
#55560 = CARTESIAN_POINT ( 'NONE',  ( 29.28750000122903074, -4.330127018922194537, 2.499999999999995559 ) ) ;
#55561 = CARTESIAN_POINT ( 'NONE',  ( 2.000000000000000444, 15.66874999877096464, 26.53589838486224650 ) ) ;
#55562 = CARTESIAN_POINT ( 'NONE',  ( 19.36875000122903501, -5.773502691896255534, -1.060575238724906372E-15 ) ) ;
#55563 = CARTESIAN_POINT ( 'NONE',  ( 11.52187500061451608, -6.054752690667223547, -1.112240025338166033E-15 ) ) ;
#55564 = LINE ( 'NONE', #509, #32546 ) ;
#55565 = ORIENTED_EDGE ( 'NONE', *, *, #33711, .F. ) ;
#55566 = EDGE_CURVE ( 'NONE', #17652, #9450, #65728, .T. ) ;
#55567 = CARTESIAN_POINT ( 'NONE',  ( 20.27812500061451573, 4.541064518000418104, 2.621784821874999949 ) ) ;
#55568 = CARTESIAN_POINT ( 'NONE',  ( 12.23437500061451821, 4.541064518000418104, 2.621784821874999949 ) ) ;
#55569 = CARTESIAN_POINT ( 'NONE',  ( 5.165625000614518569, -6.054752690667223547, -1.112240025338166033E-15 ) ) ;
#55570 = CARTESIAN_POINT ( 'NONE',  ( 21.72187500061451715, 3.027376345333611329, 5.243569643749999010 ) ) ;
#55571 = CARTESIAN_POINT ( 'NONE',  ( 5.278125000614516615, 6.421520780324663323E-16, -5.243569643749999010 ) ) ;
#55572 = FACE_OUTER_BOUND ( 'NONE', #54077, .T. ) ;
#55573 = CARTESIAN_POINT ( 'NONE',  ( 6.075000001229034829, 2.886751345948129099, -4.999999999999998224 ) ) ;
#55574 =( BOUNDED_CURVE ( )  B_SPLINE_CURVE ( 2, ( #52677, #2085, #19404, #63031, #46058, #47142, #6895 ),
 .UNSPECIFIED., .F., .F. ) 
 B_SPLINE_CURVE_WITH_KNOTS ( ( 3, 2, 2, 3 ),
 ( 0.9515180543127474966, 0.9527777777777777235, 0.9555555555555556024, 0.9567008448923609576 ),
 .UNSPECIFIED. ) 
 CURVE ( )  GEOMETRIC_REPRESENTATION_ITEM ( )  RATIONAL_B_SPLINE_CURVE ( ( 0.9335920638844523722, 0.9392424606745505278, 1.000000000000000000, 0.8660254037844387076, 1.000000000000000000, 0.9447617164785451216, 0.9350733812694886904 ) ) 
 REPRESENTATION_ITEM ( '' )  );
#55575 = CARTESIAN_POINT ( 'NONE',  ( 20.99062500061451431, -3.027376345333610441, -5.243569643749999898 ) ) ;
#55576 = CARTESIAN_POINT ( 'NONE',  ( -1.999999999999997113, 18.38750000122903572, -26.53589838486224295 ) ) ;
#55577 = CARTESIAN_POINT ( 'NONE',  ( 8.137500001229033941, -4.330127018922194537, 2.499999999999995559 ) ) ;
#55578 = CARTESIAN_POINT ( 'NONE',  ( 16.34062500061451573, -3.027376345333614438, 5.243569643749998122 ) ) ;
#55579 = CARTESIAN_POINT ( 'NONE',  ( 16.67812500061451786, 4.541064518000418104, 2.621784821874999949 ) ) ;
#55580 = CARTESIAN_POINT ( 'NONE',  ( 25.92187500061451999, -5.492252693125287522, -1.008910452111647106E-15 ) ) ;
#55581 = CARTESIAN_POINT ( 'NONE',  ( 16.94999999999999929, 0.000000000000000000, 4.999999999999998224 ) ) ;
#55582 = CARTESIAN_POINT ( 'NONE',  ( 11.40000000122903501, -2.886751345948125991, -5.000000000000000000 ) ) ;
#55583 = CARTESIAN_POINT ( 'NONE',  ( 7.340625000614518392, -3.027376345333614438, 5.243569643749998122 ) ) ;
#55584 = CARTESIAN_POINT ( 'NONE',  ( 10.30312500061451431, 4.541064518000418104, -2.621784821874998173 ) ) ;
#55585 = CARTESIAN_POINT ( 'NONE',  ( 20.32500000122903572, -5.773502691896255534, -1.060575238724906372E-15 ) ) ;
#55586 = CARTESIAN_POINT ( 'NONE',  ( -2.121784821874999949, 13.93437500061451750, -33.67503911421598417 ) ) ;
#55587 = CARTESIAN_POINT ( 'NONE',  ( 30.00000000000000000, 0.000000000000000000, 0.000000000000000000 ) ) ;
#55588 = CARTESIAN_POINT ( 'NONE',  ( 5.737500001229033586, 4.330127018922191873, 2.499999999999999556 ) ) ;
#55589 = CARTESIAN_POINT ( 'NONE',  ( 2.971875000614517592, -6.054752690667223547, -1.112240025338166033E-15 ) ) ;
#55590 = CARTESIAN_POINT ( 'NONE',  ( 19.84687500061451360, 6.054752690667223547, 3.707466751127219781E-16 ) ) ;
#55591 = CARTESIAN_POINT ( 'NONE',  ( 1.071796769724489895, 18.62990381179669797, 26.00000000000000355 ) ) ;
#55592 = CARTESIAN_POINT ( 'NONE',  ( 17.01562500061451644, 3.027376345333613106, -5.243569643749998122 ) ) ;
#55593 = CARTESIAN_POINT ( 'NONE',  ( 11.26875000122903003, -5.773502691896255534, -1.060575238724906372E-15 ) ) ;
#55594 = CARTESIAN_POINT ( 'NONE',  ( -1.999999999999999112, 20.69374999877096499, 26.53589838486224650 ) ) ;
#55595 = CARTESIAN_POINT ( 'NONE',  ( 26.62500000000000000, 6.123233995736764310E-16, -4.999999999999998224 ) ) ;
#55596 = CARTESIAN_POINT ( 'NONE',  ( 29.78437500061451715, 4.541064518000418104, 2.621784821874999949 ) ) ;
#55597 = CARTESIAN_POINT ( 'NONE',  ( 19.73437500061451289, 5.492252693125287522, 3.363034840372157021E-16 ) ) ;
#55598 = CARTESIAN_POINT ( 'NONE',  ( 14.31562500061451537, 3.027376345333613106, -5.243569643749998122 ) ) ;
#55599 = CARTESIAN_POINT ( 'NONE',  ( 14.14687500061451786, -3.027376345333614438, 5.243569643749998122 ) ) ;
#55600 = ORIENTED_EDGE ( 'NONE', *, *, #64818, .T. ) ;
#55601 = CARTESIAN_POINT ( 'NONE',  ( 21.70312500061451644, 0.000000000000000000, 5.243569643749999010 ) ) ;
#55602 = CARTESIAN_POINT ( 'NONE',  ( 1.071796769724491893, 11.13259618943233420, -26.00000000000000355 ) ) ;
#55603 = CARTESIAN_POINT ( 'NONE',  ( 22.34999999999999787, 0.000000000000000000, 4.999999999999998224 ) ) ;
#55604 = CARTESIAN_POINT ( 'NONE',  ( 11.96250000000000213, 2.886751345948126879, 4.999999999999999112 ) ) ;
#55605 = CARTESIAN_POINT ( 'NONE',  ( 20.62500000122903288, 2.886751345948126879, 4.999999999999999112 ) ) ;
#55606 = CARTESIAN_POINT ( 'NONE',  ( 16.22812500061451857, 4.541064518000418104, 2.621784821874999949 ) ) ;
#55607 = CARTESIAN_POINT ( 'NONE',  ( 11.82187500061451502, -4.119189519843968306, 2.378215178124996054 ) ) ;
#55608 = VERTEX_POINT ( 'NONE', #32699 ) ;
#55609 = CARTESIAN_POINT ( 'NONE',  ( 19.04999999999999716, 4.330127018922192761, -2.499999999999997780 ) ) ;
#55610 = CARTESIAN_POINT ( 'NONE',  ( 21.57187500061451502, 3.027376345333613106, -5.243569643749998122 ) ) ;
#55611 = CARTESIAN_POINT ( 'NONE',  ( 27.29062500061451502, -3.027376345333610441, -5.243569643749999898 ) ) ;
#55612 = ORIENTED_EDGE ( 'NONE', *, *, #32061, .T. ) ;
#55613 = LINE ( 'NONE', #50075, #70193 ) ;
#55614 = CARTESIAN_POINT ( 'NONE',  ( 9.740625000614516082, -3.027376345333610441, -5.243569643749999898 ) ) ;
#55615 = DIRECTION ( 'NONE',  ( 0.000000000000000000, 0.000000000000000000, -1.000000000000000000 ) ) ;
#55616 = CARTESIAN_POINT ( 'NONE',  ( 13.80937500061451395, 2.746126346562645981, -4.756430356249997438 ) ) ;
#55617 = CARTESIAN_POINT ( 'NONE',  ( 17.17500000000000071, 6.123233995736764310E-16, -4.999999999999998224 ) ) ;
#55618 = CARTESIAN_POINT ( 'NONE',  ( 23.77499999999999858, -4.330127018922194537, 2.499999999999995559 ) ) ;
#55619 = CARTESIAN_POINT ( 'NONE',  ( 45.00000000000000000, 0.000000000000000000, 0.000000000000000000 ) ) ;
#55620 = CARTESIAN_POINT ( 'NONE',  ( 3.421875000614516882, -6.054752690667223547, -1.112240025338166033E-15 ) ) ;
#55621 = CARTESIAN_POINT ( 'NONE',  ( 27.90937500061451715, 4.541064518000418104, -2.621784821874998173 ) ) ;
#55622 = VERTEX_POINT ( 'NONE', #17147 ) ;
#55623 = CARTESIAN_POINT ( 'NONE',  ( 26.87812500061451360, 6.421520780324663323E-16, -5.243569643749999010 ) ) ;
#55624 = CARTESIAN_POINT ( 'NONE',  ( 26.22187500061451715, 3.027376345333611329, 5.243569643749999010 ) ) ;
#55625 = CARTESIAN_POINT ( 'NONE',  ( -4.243569643749999898, 18.45312500061459104, -30.00000000000000000 ) ) ;
#55626 = CARTESIAN_POINT ( 'NONE',  ( 14.17500000000000071, 4.330127018922191873, 2.499999999999999556 ) ) ;
#55627 = CARTESIAN_POINT ( 'NONE',  ( 10.45312500061451644, 0.000000000000000000, 5.243569643749999010 ) ) ;
#55628 = CARTESIAN_POINT ( 'NONE',  ( 5.810221930991193690E-16, 17.50624999877096499, 26.00000000000000000 ) ) ;
#55629 = CARTESIAN_POINT ( 'NONE',  ( -2.556497649636125342E-15, 19.21250000000000213, -26.00000000000000000 ) ) ;
#55630 = CARTESIAN_POINT ( 'NONE',  ( 26.09062500061451573, 6.054752690667223547, 3.707466751127219781E-16 ) ) ;
#55631 = CARTESIAN_POINT ( 'NONE',  ( 16.38750000122903216, 6.123233995736764310E-16, -4.999999999999998224 ) ) ;
#55632 = CARTESIAN_POINT ( 'NONE',  ( 8.568750001229034297, -5.773502691896255534, -1.060575238724906372E-15 ) ) ;
#55633 = CARTESIAN_POINT ( 'NONE',  ( 15.90937500061451892, 0.000000000000000000, 4.756430356249998326 ) ) ;
#55634 = CARTESIAN_POINT ( 'NONE',  ( 4.115625000614516082, 3.027376345333611329, 5.243569643749999010 ) ) ;
#55635 = CARTESIAN_POINT ( 'NONE',  ( 21.45937500061451786, -4.541064518000417216, -2.621784821875001281 ) ) ;
#55636 = CARTESIAN_POINT ( 'NONE',  ( -4.243569643749999898, 13.97187500061451715, 27.54997392385601529 ) ) ;
#55637 = CARTESIAN_POINT ( 'NONE',  ( 22.17187500061451644, 3.027376345333611329, 5.243569643749999010 ) ) ;
#55638 = CARTESIAN_POINT ( 'NONE',  ( 29.82187500061451502, 3.027376345333611329, 5.243569643749999010 ) ) ;
#55639 = CARTESIAN_POINT ( 'NONE',  ( 4.243569643749999898, 17.83437500061451786, 30.00000000000000000 ) ) ;
#55640 = CARTESIAN_POINT ( 'NONE',  ( 8.803125000614517859, -4.541064518000417216, -2.621784821875001281 ) ) ;
#55641 = DIRECTION ( 'NONE',  ( -0.000000000000000000, 6.195440985631455317E-17, 1.000000000000000000 ) ) ;
#55642 = CARTESIAN_POINT ( 'NONE',  ( 7.396875000614519635, -3.027376345333614438, 5.243569643749998122 ) ) ;
#55643 = FACE_OUTER_BOUND ( 'NONE', #29310, .T. ) ;
#55644 = CARTESIAN_POINT ( 'NONE',  ( 8.465625000614515727, 3.027376345333613106, -5.243569643749998122 ) ) ;
#55645 = CARTESIAN_POINT ( 'NONE',  ( 12.49687500061451573, -3.027376345333610441, -5.243569643749999898 ) ) ;
#55646 = CARTESIAN_POINT ( 'NONE',  ( 18.63750000122903216, 6.123233995736764310E-16, -4.999999999999998224 ) ) ;
#55647 = CARTESIAN_POINT ( 'NONE',  ( 7.359375000614516438, 0.000000000000000000, 5.243569643749999010 ) ) ;
#55648 = CARTESIAN_POINT ( 'NONE',  ( 10.94062500061451537, -3.027376345333614438, 5.243569643749998122 ) ) ;
#55649 = CARTESIAN_POINT ( 'NONE',  ( 7.265625000614516438, 3.027376345333611329, 5.243569643749999010 ) ) ;
#55650 = CARTESIAN_POINT ( 'NONE',  ( 25.81875000122903074, 2.886751345948129099, -4.999999999999998224 ) ) ;
#55651 = CARTESIAN_POINT ( 'NONE',  ( 18.68437500061451928, -4.541064518000419881, 2.621784821874995952 ) ) ;
#55652 = CARTESIAN_POINT ( 'NONE',  ( 4.535435261965744758, 2.105238004946854868, 4.730754414875756986 ) ) ;
#55653 = CARTESIAN_POINT ( 'NONE',  ( 11.39062500061451644, -3.027376345333614438, 5.243569643749998122 ) ) ;
#55654 = DIRECTION ( 'NONE',  ( 1.000000000000000000, -0.000000000000000000, -0.000000000000000000 ) ) ;
#55655 = CARTESIAN_POINT ( 'NONE',  ( -4.243569643749999898, 13.07187500061452035, -32.45002607614398471 ) ) ;
#55656 = CARTESIAN_POINT ( 'NONE',  ( 12.15000000122903501, -2.886751345948129988, 4.999999999999997335 ) ) ;
#55657 = CARTESIAN_POINT ( 'NONE',  ( -2.121784821874996840, 15.82812500061451644, -26.32496088578401583 ) ) ;
#55658 = CARTESIAN_POINT ( 'NONE',  ( 14.81250000122903288, 0.000000000000000000, 4.999999999999998224 ) ) ;
#55659 = CARTESIAN_POINT ( 'NONE',  ( 11.35312500061451679, 0.000000000000000000, 5.243569643749999010 ) ) ;
#55660 = ORIENTED_EDGE ( 'NONE', *, *, #41079, .F. ) ;
#55661 = CARTESIAN_POINT ( 'NONE',  ( 13.98750000000000249, -2.886751345948125991, -5.000000000000000000 ) ) ;
#55662 = CYLINDRICAL_SURFACE ( 'NONE', #47977, 4.999999999999998224 ) ;
#55663 = CARTESIAN_POINT ( 'NONE',  ( 23.80312500061451786, 4.541064518000418104, -2.621784821874998173 ) ) ;
#55664 = CARTESIAN_POINT ( 'NONE',  ( 7.396875000614519635, -3.027376345333614438, 5.243569643749998122 ) ) ;
#55665 = CARTESIAN_POINT ( 'NONE',  ( 10.42500000122903536, -5.773502691896255534, -1.060575238724906372E-15 ) ) ;
#55666 = CARTESIAN_POINT ( 'NONE',  ( 18.30000000122903359, 5.773502691896255534, 3.535250795749688894E-16 ) ) ;
#55667 = CARTESIAN_POINT ( 'NONE',  ( 14.99062500061451786, -3.027376345333614438, 5.243569643749998122 ) ) ;
#55668 = CARTESIAN_POINT ( 'NONE',  ( 17.76562500061451644, -6.054752690667223547, -1.112240025338166033E-15 ) ) ;
#55669 = CARTESIAN_POINT ( 'NONE',  ( 25.65000000122903145, -2.886751345948129988, 4.999999999999997335 ) ) ;
#55670 = EDGE_CURVE ( 'NONE', #8461, #17653, #40851, .T. ) ;
#55671 = CARTESIAN_POINT ( 'NONE',  ( 27.93750000122903288, -4.330127018922194537, 2.499999999999995559 ) ) ;
#55672 = CARTESIAN_POINT ( 'NONE',  ( 22.94999999999999929, -4.330127018922190985, -2.500000000000001332 ) ) ;
#55673 = CARTESIAN_POINT ( 'NONE',  ( 3.756430356249998770, 14.85312499938548392, 32.16877607737302469 ) ) ;
#55674 = CARTESIAN_POINT ( 'NONE',  ( 25.17187500061451644, 3.027376345333613106, -5.243569643749998122 ) ) ;
#55675 = CARTESIAN_POINT ( 'NONE',  ( 18.41250000122903430, 0.000000000000000000, 4.999999999999998224 ) ) ;
#55676 = CARTESIAN_POINT ( 'NONE',  ( 11.85000000122903430, -2.886751345948125991, -5.000000000000000000 ) ) ;
#55677 = CARTESIAN_POINT ( 'NONE',  ( 27.87187500061451573, 3.027376345333613106, -5.243569643749998122 ) ) ;
#55678 = ADVANCED_FACE ( 'NONE', ( #72950 ), #22332, .T. ) ;
#55679 = CARTESIAN_POINT ( 'NONE',  ( 22.61250000000000426, 2.886751345948095793, -5.000000000000055067 ) ) ;
#55680 = CARTESIAN_POINT ( 'NONE',  ( 5.671875000614519102, -6.054752690667223547, -1.112240025338166033E-15 ) ) ;
#55681 = CARTESIAN_POINT ( 'NONE',  ( 24.85312500061451502, 0.000000000000000000, 5.243569643749999010 ) ) ;
#55682 = CARTESIAN_POINT ( 'NONE',  ( 3.756430356249998770, 13.61562499938548321, 32.16877607737301759 ) ) ;
#55683 = CARTESIAN_POINT ( 'NONE',  ( 1.071796769724490783, 19.68259618943233491, -26.00000000000000000 ) ) ;
#55684 = CARTESIAN_POINT ( 'NONE',  ( 10.62187500061451928, -6.054752690667223547, -1.112240025338166033E-15 ) ) ;
#55685 = LINE ( 'NONE', #72680, #34763 ) ;
#55686 = CARTESIAN_POINT ( 'NONE',  ( 3.609375000614516882, 4.541064518000418104, -2.621784821874998173 ) ) ;
#55687 = CARTESIAN_POINT ( 'NONE',  ( 5.484375000614518214, 4.541064518000418104, 2.621784821874999949 ) ) ;
#55688 = CARTESIAN_POINT ( 'NONE',  ( 28.13437500061451502, -4.541064518000419881, 2.621784821874995952 ) ) ;
#55689 = CARTESIAN_POINT ( 'NONE',  ( 45.00000000000000000, 0.000000000000000000, 4.999999999999998224 ) ) ;
#55690 = CARTESIAN_POINT ( 'NONE',  ( 19.01249999999999929, 2.886751345948129099, -4.999999999999998224 ) ) ;
#55691 = EDGE_LOOP ( 'NONE', ( #40533, #73061, #21170, #55487 ) ) ;
#55693 = EDGE_CURVE ( 'NONE', #7820, #53311, #42088, .T. ) ;
#55692 = CARTESIAN_POINT ( 'NONE',  ( 27.33750000000000213, -2.886751345948129988, 4.999999999999997335 ) ) ;
#55694 = CARTESIAN_POINT ( 'NONE',  ( 27.75937500061451502, -4.541064518000417216, -2.621784821875001281 ) ) ;
#55695 = EDGE_LOOP ( 'NONE', ( #50084, #48977, #15706, #46259 ) ) ;
#55696 = AXIS2_PLACEMENT_3D ( 'NONE', #25196, #3045, #13754 ) ;
#55697 = CARTESIAN_POINT ( 'NONE',  ( 17.65312500061451573, 0.000000000000000000, 5.243569643749999010 ) ) ;
#55698 = CARTESIAN_POINT ( 'NONE',  ( 8.540625000614518569, 6.054752690667223547, 3.707466751127219781E-16 ) ) ;
#55699 = CARTESIAN_POINT ( 'NONE',  ( 20.59687500061451715, 4.119189519843966529, -2.378215178124998275 ) ) ;
#55700 = CARTESIAN_POINT ( 'NONE',  ( 4.134375000614517681, 4.541064518000418104, 2.621784821874999949 ) ) ;
#55701 = CARTESIAN_POINT ( 'NONE',  ( 17.32500000122903216, 2.886751345948129099, -4.999999999999998224 ) ) ;
#55702 = CARTESIAN_POINT ( 'NONE',  ( 3.999999999999999112, 13.92500000000000071, -30.00000000000000000 ) ) ;
#55703 = CARTESIAN_POINT ( 'NONE',  ( 7.396875000614519635, -3.027376345333614438, 5.243569643749998122 ) ) ;
#55704 = CARTESIAN_POINT ( 'NONE',  ( 11.10937500061451644, -4.541064518000417216, -2.621784821875001281 ) ) ;
#55705 = CARTESIAN_POINT ( 'NONE',  ( 23.33437500061451786, 6.421520780324663323E-16, -5.243569643749999010 ) ) ;
#55706 = CARTESIAN_POINT ( 'NONE',  ( 9.525000000000002132, 6.123233995736764310E-16, -4.999999999999998224 ) ) ;
#55707 = ORIENTED_EDGE ( 'NONE', *, *, #14692, .F. ) ;
#55708 = CARTESIAN_POINT ( 'NONE',  ( 9.862500000000000711, -5.773502691896255534, -1.060575238724906372E-15 ) ) ;
#55709 = CARTESIAN_POINT ( 'NONE',  ( 17.29687500061451999, -3.027376345333614438, 5.243569643749998122 ) ) ;
#55710 = CARTESIAN_POINT ( 'NONE',  ( 9.346875000614517148, -3.027376345333610441, -5.243569643749999898 ) ) ;
#55711 = CARTESIAN_POINT ( 'NONE',  ( 3.756430356250000102, 14.89062499938548356, 30.00000000000000000 ) ) ;
#55712 = CARTESIAN_POINT ( 'NONE',  ( 20.96250000000000213, 2.886751345948126879, 4.999999999999999112 ) ) ;
#55713 = CARTESIAN_POINT ( 'NONE',  ( -3.999999999999999556, 17.18750000000000000, 27.69059892324149175 ) ) ;
#55714 = CARTESIAN_POINT ( 'NONE',  ( -2.121784821874999949, 9.884375000614518569, -33.67503911421598417 ) ) ;
#55715 = CARTESIAN_POINT ( 'NONE',  ( 22.47187500061451715, 2.746126346562645981, -4.756430356249997438 ) ) ;
#55716 = CARTESIAN_POINT ( 'NONE',  ( 12.96562500061451750, 3.027376345333613106, -5.243569643749998122 ) ) ;
#55717 = CARTESIAN_POINT ( 'NONE',  ( 28.88437500061451502, 4.541064518000418104, 2.621784821874999949 ) ) ;
#55718 =( BOUNDED_CURVE ( )  B_SPLINE_CURVE ( 2, ( #60925, #16225, #73111, #38776, #50225, #6235, #55396 ),
 .UNSPECIFIED., .F., .F. ) 
 B_SPLINE_CURVE_WITH_KNOTS ( ( 3, 2, 2, 3 ),
 ( 0.1000000000000000611, 0.1027777777777778151, 0.1055555555555555969, 0.1083333333333333648 ),
 .UNSPECIFIED. ) 
 CURVE ( )  GEOMETRIC_REPRESENTATION_ITEM ( )  RATIONAL_B_SPLINE_CURVE ( ( 0.9999999999999973355, 0.8660254037844413721, 1.000000000000000000, 0.8660254037844387076, 1.000000000000000000, 0.8660254037844373753, 1.000000000000001332 ) ) 
 REPRESENTATION_ITEM ( '' )  );
#55719 = CARTESIAN_POINT ( 'NONE',  ( 10.08750000122903323, 6.123233995736764310E-16, -4.999999999999998224 ) ) ;
#55720 = CARTESIAN_POINT ( 'NONE',  ( 29.82187500061451502, 3.027376345333611329, 5.243569643749999010 ) ) ;
#55721 = CARTESIAN_POINT ( 'NONE',  ( 9.562500000000001776, 2.886751345948129099, -4.999999999999998224 ) ) ;
#55722 = CARTESIAN_POINT ( 'NONE',  ( 3.999999999999999112, 16.28750000122903430, 30.00000000000000000 ) ) ;
#55723 = CARTESIAN_POINT ( 'NONE',  ( 10.35000000122903074, -2.886751345948129988, 4.999999999999997335 ) ) ;
#55724 = CARTESIAN_POINT ( 'NONE',  ( 19.73437500061451644, 6.421520780324663323E-16, -5.243569643749999010 ) ) ;
#55725 = CARTESIAN_POINT ( 'NONE',  ( 13.73437500061451821, -4.541064518000419881, 2.621784821874995952 ) ) ;
#55726 = CYLINDRICAL_SURFACE ( 'NONE', #45477, 3.999999999999996447 ) ;
#55727 = ORIENTED_EDGE ( 'NONE', *, *, #21809, .F. ) ;
#55728 = CARTESIAN_POINT ( 'NONE',  ( 15.92812500061451608, -4.541064518000419881, 2.621784821874995952 ) ) ;
#55729 = CARTESIAN_POINT ( 'NONE',  ( 29.43750000122903288, 6.123233995736764310E-16, -4.999999999999998224 ) ) ;
#55730 = CARTESIAN_POINT ( 'NONE',  ( 15.45937500061451608, 0.000000000000000000, 5.243569643749999010 ) ) ;
#55731 = CARTESIAN_POINT ( 'NONE',  ( 27.20625000122903359, 4.330127018922192761, -2.499999999999997780 ) ) ;
#55732 = CARTESIAN_POINT ( 'NONE',  ( 16.56562500061451715, 3.027376345333613106, -5.243569643749998122 ) ) ;
#55733 = CARTESIAN_POINT ( 'NONE',  ( 18.07500000122903216, -5.773502691896255534, -1.060575238724906372E-15 ) ) ;
#55734 = CARTESIAN_POINT ( 'NONE',  ( 27.30937500061451573, -4.541064518000417216, -2.621784821875001281 ) ) ;
#55735 = CARTESIAN_POINT ( 'NONE',  ( -2.121784821874999949, 9.828125000614516438, 26.32496088578401938 ) ) ;
#55736 = CARTESIAN_POINT ( 'NONE',  ( 15.72187500061451892, 3.027376345333613106, -5.243569643749998122 ) ) ;
#55737 = CARTESIAN_POINT ( 'NONE',  ( 13.27500000122903323, 2.886751345948129099, -4.999999999999998224 ) ) ;
#55738 = CARTESIAN_POINT ( 'NONE',  ( 9.946875000614516793, 5.492252693125287522, 3.363034840372157021E-16 ) ) ;
#55739 = CARTESIAN_POINT ( 'NONE',  ( -2.121784821874996840, 18.13437500061451502, -26.32496088578401583 ) ) ;
#55740 = CARTESIAN_POINT ( 'NONE',  ( 20.18437500061451573, 6.421520780324663323E-16, -5.243569643749999010 ) ) ;
#55741 = CARTESIAN_POINT ( 'NONE',  ( 22.20000000122903216, -2.886751345948125991, -5.000000000000000000 ) ) ;
#55742 = CARTESIAN_POINT ( 'NONE',  ( 17.63437500061451502, 4.541064518000418104, 2.621784821874999949 ) ) ;
#55743 = CARTESIAN_POINT ( 'NONE',  ( -4.243569643749997233, 12.69687500061451857, 32.45002607614398471 ) ) ;
#55744 = CARTESIAN_POINT ( 'NONE',  ( 16.82812500061451644, -4.541064518000419881, 2.621784821874995952 ) ) ;
#55745 = VERTEX_POINT ( 'NONE', #56674 ) ;
#55746 = ORIENTED_EDGE ( 'NONE', *, *, #12056, .T. ) ;
#55747 = CARTESIAN_POINT ( 'NONE',  ( 21.03750000000000142, -2.886751345948129988, 4.999999999999997335 ) ) ;
#55748 = CARTESIAN_POINT ( 'NONE',  ( 3.972658874145789110, 3.036112888163414514, -4.275165627105516286 ) ) ;
#55749 = CARTESIAN_POINT ( 'NONE',  ( 23.80312500061451786, 4.541064518000418104, -2.621784821874998173 ) ) ;
#55750 = CARTESIAN_POINT ( 'NONE',  ( 4.865625000614517859, 3.027376345333613106, -5.243569643749998122 ) ) ;
#55751 = CARTESIAN_POINT ( 'NONE',  ( 16.42500000122903359, 2.886751345948129099, -4.999999999999998224 ) ) ;
#55752 = CARTESIAN_POINT ( 'NONE',  ( 23.05312500061451431, 0.000000000000000000, 5.243569643749999010 ) ) ;
#55753 = CARTESIAN_POINT ( 'NONE',  ( 20.24999999999999645, -4.330127018922190985, -2.500000000000001332 ) ) ;
#55754 = CARTESIAN_POINT ( 'NONE',  ( 26.54062500061451146, 6.054752690667223547, 3.707466751127219781E-16 ) ) ;
#55755 = CARTESIAN_POINT ( 'NONE',  ( 6.553125000614518747, -4.541064518000417216, -2.621784821875001281 ) ) ;
#55756 = EDGE_LOOP ( 'NONE', ( #12126, #23865 ) ) ;
#55757 = VECTOR ( 'NONE', #70577, 1000.000000000000000 ) ;
#55758 = FACE_OUTER_BOUND ( 'NONE', #66652, .T. ) ;
#55759 = CARTESIAN_POINT ( 'NONE',  ( 2.803125000614518747, 0.000000000000000000, 5.243569643749999010 ) ) ;
#55760 = CARTESIAN_POINT ( 'NONE',  ( 12.04687500061451821, -2.746126346562642428, -4.756430356249999214 ) ) ;
#55761 = LINE ( 'NONE', #49861, #8765 ) ;
#55762 = CARTESIAN_POINT ( 'NONE',  ( -3.999999999999999556, 10.62500000122903643, -32.30940107675850470 ) ) ;
#55763 = EDGE_CURVE ( 'NONE', #13629, #20263, #21233, .T. ) ;
#55764 = CARTESIAN_POINT ( 'NONE',  ( -2.121784821874996840, 19.03437500061451715, -26.32496088578401583 ) ) ;
#55765 =( BOUNDED_SURFACE ( )  B_SPLINE_SURFACE ( 1, 2, ( 
 ( #51082, #28195, #38914, #45549, #55537, #61434, #6013, #22988, #68078, #17447, #56969, #4932, #21912, #67714, #6373, #27467, #67362, #40004, #62518, #10827, #33362, #44468, #55899, #50368, #44827, #17086, #11197, #11916, #39647, #61792, #56269, #5659, #50724, #127, #56618, #34441, #28905, #51443, #845, #12635, #57335, #29273, #7099, #29628, #40725, #63603, #52165, #24440, #24802, #52887, #58050, #1568, #19614, #46624, #18526, #34803, #13720, #41091, #2644, #1935, #68801, #24078, #25163, #69167, #46989, #64327, #63241, #12993, #8185, #35529, #7458, #29985, #69525, #52527, #18883, #57694, #51803, #47704, #41446, #70243, #63964, #46261, #35170, #13348, #58776, #35885, #58410, #42171, #36261, #7823, #1206, #30358, #64697, #2285, #30713, #47345, #69879, #19244, #23711, #41799, #53246, #6739, #18157, #43639, #38083, #3390, #3009, #9651, #49548, #72070, #21450, #65797, #54358, #43276, #54718, #71343, #19981, #31819, #44006, #8921, #14451, #15178, #37717, #60237, #20718, #10014, #26276, #14081, #8551, #9286, #31451, #14815, #3752, #48080, #36621, #59142, #31078, #25911, #32185, #42901, #21088, #48813, #48451, #66163, #4487, #27016, #53618, #15539, #4121, #37358, #42534, #26650, #70608, #49186, #59880, #25539, #60605, #65060, #70975, #53993, #36985, #59507, #20350, #71716, #65425, #32550, #55087, #27742, #11104, #50281, #16275, #38831, #33275, #61346, #55450, #67988, #72805, #23265, #66528, #27377, #55814, #51354, #4843, #40, #49909, #22188, #39190, #33993, #39919, #5201, #33633, #15908, #44742, #22545, #56177, #38456, #10742, #66907, #45093, #67628, #16994, #39552, #62433, #5570, #28816, #60982, #61705, #67276, #16635, #28107, #72433, #757, #10381, #32913, #50636, #62077, #11470, #390, #56530, #5923, #45456, #56882, #6287, #21817, #17362, #28457, #50992, #44382, #22897, #11831, #34349, #18440, #40272, #52804, #17712, #7012, #12549, #23629, #12186, #52079, #7372, #2561, #53164, #18074, #29543, #63520, #1484, #68714, #40635, #35083, #63154, #34713, #47263, #23990, #45815, #68351, #6656, #57609, #30632, #57243, #52443, #29185, #46537, #41005, #13265, #19163, #69079, #12907, #62793, #35440, #1848, #1120, #57964, #41717, #29903, #24356, #46904, #69443, #18800, #41364, #63874, #51718, #13632, #35803, #58693, #58325, #46175, #7736, #30271, #69797, #2205, #24720, #64244, #36176, #8104, #42092, #70529, #55001, #59795, #71631, #53910, #71254, #70893, #64614, #3303, #59425, #36905, #25830, #54631, #49102, #14370, #14000, #20634, #60523, #9929, #32468, #3668, #65341, #54274, #65712, #9201, #30999, #48731, #43192, #15098, #37634, #26562, #38001, #36539, #37273, #21004, #25081, #8833, #60157, #9567, #59059, #8464, #47624, #70157, #19534, #2928, #31736, #48367, #32099, #26191, #53532, #25457, #48001, #19904, #31369, #4038, #20266, #43556, #66078, #15456, #42456, #64979, #42818, #14731, #49829, #10300, #33191, #72353, #67193, #67550, #22464, #27658, #44295, #62355, #16196, #61267, #4407, #56454, #10661, #45373, #44663, #38370, #21734, #67909, #66823, #16554, #33910, #16913, #5844, #55730, #45014, #311, #32831, #50555, #55369, #33547, #26936, #50197, #61991, #43923, #4762, #39468, #11391, #39106, #72722, #22821, #49461, #28376, #15826, #22105, #73083, #61622, #60895, #71995, #50913, #5124, #38747, #11025, #17279, #27295, #21369, #56097, #39841, #11751, #34268, #66449, #5488, #28027, #68998, #6206, #46460, #18723, #41287, #17997, #29106, #35005, #18359, #1766, #29827, #57163, #46099, #35727, #63444, #2129, #57888, #23549, #23185, #58249, #62717, #52362, #29466, #40196, #46828, #24640, #17636, #40930, #12111, #34634, #45739, #28734, #63074, #7297, #52002, #7654, #69365, #12830, #6576, #51275, #679, #51641, #1042, #68635, #12476, #40556, #35364, #63798, #24280, #6935, #57535, #41641, #1403, #23912, #56801, #30193, #13188, #47186, #52722, #69718, #19086, #64160, #13548, #68274, #65630, #26110, #15017, #19824, #54191, #32017, #42010, #9120, #64530, #65258, #36095, #8751, #20546, #2479, #13924, #3588, #48649, #25748, #59340, #54553, #8022, #37555, #47546, #31284, #31657, #48285, #70075, #58615, #60077, #64898, #30914, #53455, #9488, #19450, #30558, #53826, #43104, #71174, #3955, #26478, #49018, #2845, #70809, #53084, #20184, #71549, #20923, #70448, #8384, #14288, #42739, #43475, #65999, #36462, #25374, #25004, #14648, #58977, #37189, #47919, #42376, #36825, #3219, #59713, #61187, #71914, #5405, #56376, #49383, #39027, #33465, #10943, #56012, #16835, #28299, #54919, #27579, #39389, #50834, #27213, #27942, #50475, #21288, #26851, #234, #37922, #22742, #66367, #50111, #44210, #73001, #10218, #15743, #44580, #16468, #67112, #22023, #11313, #72640, #45292, #9850, #10582, #32751, #16112, #33109, #43841, #15380, #60440, #32379, #49748, #61541, #66742, #22385, #55647, #72276, #67472, #5768, #4326, #38282, #61908, #44934, #38664, #60810, #33834, #55289, #4683, #5043, #21653, #1676, #39760, #29022, #34551, #45659, #34188, #959, #29383, #24551, #2040, #40116, #51558, #12382, #23468, #17555, #62632, #57079, #12026, #56722, #69273, #46014, #67826, #17199, #28655, #6487, #52634, #6124, #1314, #51194, #68551, #40472, #35277, #41199, #17909, #34918, #62277, #62987, #23823, #23102, #57445, #63707, #6849, #51917, #46374, #68908, #18266, #40839, #63357, #11671, #35637, #12741, #7563, #57799, #597, #68192, #7208, #18635, #29737, #52274, #24185, #46739, #13099, #58159, #30099, #4860, #8659, #21470, #2756, #21104, #19730, #64070, #25276, #8296, #58886, #47823, #4505, #72087, #36370, #36000, #43657, #10398, #32930, #55468, #25654, #14194, #3125, #15557, #31190, #52996, #64804, #47097, #66179, #70353, #55105, #36729, #30826, #27034, #38475, #60999, #18991, #49565, #38100, #42280, #2392, #60622, #30467 ),
 ( #69629, #41553, #19357, #41914, #24911, #59251, #64439, #53732, #10032, #32567, #48190, #13831, #13452, #53359, #71734, #58519, #44024, #66546, #15925, #7929, #47454, #69987, #17729, #22205, #17012, #56898, #17378, #6304, #11123, #45473, #23282, #33292, #407, #55831, #56547, #27395, #57, #11847, #66925, #5218, #68006, #39936, #39570, #50653, #45831, #72451, #28832, #38848, #22563, #22916, #62094, #61363, #49926, #51371, #56195, #44759, #67294, #774, #10760, #21835, #45110, #34366, #62449, #68368, #40288, #62809, #16652, #11488, #44399, #34010, #12202, #34730, #61722, #72822, #5588, #5941, #57259, #16294, #27760, #39209, #50300, #28474, #33650, #51010, #28125, #67646, #8118, #12565, #2220, #52457, #63170, #69811, #18814, #35456, #41730, #63888, #40650, #35099, #68730, #51735, #12922, #7749, #1864, #30646, #19176, #13278, #57624, #29200, #1135, #52095, #1499, #7028, #57979, #24005, #69456, #64258, #24733, #29917, #46553, #64628, #18456, #63536, #6672, #58707, #7388, #47638, #46918, #29558, #69094, #70171, #41020, #41377, #36189, #13645, #53178, #24370, #47277, #2575, #35817, #52818, #58339, #30286, #23645, #25094, #19548, #46190, #42105, #14014, #36553, #18089, #65355, #21016, #31011, #4049, #25469, #14745, #43204, #9215, #48015, #8477, #54645, #70907, #59439, #8846, #49115, #70541, #59073, #31752, #26575, #32111, #71643, #38013, #43569, #3317, #26206, #53544, #48745, #66090, #15469, #42833, #25843, #37287, #71269, #9579, #37647, #31382, #20279, #60535, #20647, #9942, #15110, #48380, #19916, #2940, #59810, #42470, #65724, #54289, #64993, #14383, #3682, #36918, #53922, #60170, #70033, #53410, #64854, #18315, #64118, #2802, #14242, #63755, #19406, #13879, #12787, #63402, #36780, #1363, #59296, #29784, #40886, #25329, #35684, #8706, #51964, #35324, #41243, #23872, #57846, #58571, #7256, #13144, #24596, #41964, #47875, #18680, #69675, #46420, #58206, #7978, #52320, #46785, #70403, #7610, #30147, #52679, #19041, #2087, #47144, #1723, #68958, #19779, #41599, #24235, #13503, #69320, #36050, #30514, #42329, #53041, #2436, #24958, #30870, #47502, #64486, #36418, #58934, #8341, #4643, #60035, #4281, #3913, #48239, #9446, #65586, #43061, #31974, #60769, #55248, #20504, #20139, #26807, #66698, #16070, #38620, #9805, #71505, #60397, #71873, #15337, #37143, #48976, #61144, #26067, #31614, #32338, #54876, #49341, #37877, #27173, #43435, #31239, #25703, #26435, #48606, #54510, #20881, #65216, #53780, #3176, #70764, #14976, #21245, #65957, #38240, #43799, #37514, #10176, #21613, #44168, #42694, #32711, #66324, #15701, #59670, #49707, #14606, #72235, #9078, #54150, #3544, #71131, #44896, #50437, #61502, #50068, #16794, #45252, #40429, #17870, #55970, #67432, #28261, #39351, #33427, #5364, #72962, #27902, #45619, #44540, #21981, #68507, #33067, #10539, #10899, #22700, #61865, #68153, #67785, #67071, #16429, #72598, #55606, #11272, #11632, #56336, #34511, #554, #17159, #22344, #5002, #27536, #33793, #5726, #38987, #50792, #195, #39718, #23064, #28616, #62236, #34148, #56685, #6084, #51153, #17516, #62592, #40077, #51519, #11988, #57040, #6446, #918, #28981, #23427, #45973, #41167, #19694, #2360, #41520, #13066, #59584, #69954, #31529, #13800, #30065, #24520, #69598, #42610, #53325, #70319, #3465, #70680, #18960, #35605, #64039, #48524, #2724, #65135, #47424, #64771, #64407, #58124, #19324, #52963, #30435, #41878, #48155, #14526, #7898, #7532, #14161, #54069, #25985, #18603, #42247, #58854, #47786, #59217, #25240, #47064, #36340, #63676, #13418, #35967, #36695, #8625, #31154, #53695, #37060, #30795, #52603, #2009, #8264, #58489, #3089, #25618, #24877, #20055, #8997, #55889, #9724, #44083, #26725, #4920, #38158, #32257, #49985, #61423, #10817, #42975, #72510, #66610, #21162, #26351, #15985, #59955, #65505, #4196, #72149, #43715, #21898, #61058, #55165, #48890, #20426, #14893, #43353, #65875, #3830, #49260, #15256, #60681, #10457, #38535, #66237, #37793, #5277, #54790, #71793, #71051, #44455, #15616, #38904, #10095, #31895, #60314, #33351, #32625, #4562, #66985, #27090, #49622, #71420, #32986, #16349, #20797, #55526, #21527, #27455, #37433, #27823, #9362, #54431, #56257, #68424, #62866, #39994, #469, #68791, #22264, #51793, #61781, #22977, #45892, #62507, #11185, #72882, #6729, #6002, #45171, #67702, #23702, #33710, #50355, #45539, #57325, #40346, #12262, #18147, #46250, #17074, #11906, #44817, #34430, #34792, #29263, #11549, #22620, #28535, #56959, #17786, #23344, #50711, #39634, #1194, #6362, #40714, #51433, #62152, #16713, #63231, #5647, #12625, #68068, #28183, #35160, #57684, #115, #835, #7089, #67351, #39269, #34065, #56606, #51071, #28894, #17436, #42524, #41436, #70230, #64687, #63594, #41081, #14440, #52154, #36975, #7448, #41788, #58399, #14072, #13708, #12983, #35519, #58765, #29618, #2275, #36611, #69156, #58038, #47694, #42160, #19234, #52877, #48070, #1557, #31068, #29974, #24792, #25154, #64318, #52516, #24068, #59132, #7813, #24430, #46979, #2999, #1925, #46613, #47335, #8540, #19604, #53606, #70597, #25527, #69515, #36251, #18515, #8175, #19971, #65050, #63952, #18874, #30349, #30703, #59497, #2633, #13337, #35875, #69868, #53236, #27368, #10005, #48803, #48440, #10372, #14804, #4478, #54707, #65416, #72061, #49900, #42891, #32540, #27007, #49538, #21440, #32903, #21807, #70965, #21080, #55442, #44371, #20708, #43997, #66519, #37348, #20338, #66898, #31441, #16266, #59870, #43630, #37705, #15899, #66152, #9274, #31809, #54347, #53981, #15168, #55078, #4112, #4834, #38446, #15530, #3741, #3379, #25900, #26266, #71332, #43265, #60227, #65787, #71707, #60972, #72424, #32174, #9640, #38821, #26640, #49177, #8910, #38072, #60596, #29178, #28448, #22178, #56166, #51711 ) ),
 .UNSPECIFIED., .F., .F., .F. ) 
 B_SPLINE_SURFACE_WITH_KNOTS ( ( 2, 2 ),
 ( 3, 2, 2, 2, 2, 2, 2, 2, 2, 2, 2, 2, 2, 2, 2, 2, 2, 2, 2, 2, 2, 2, 2, 2, 2, 2, 2, 2, 2, 2, 2, 2, 2, 2, 2, 2, 2, 2, 2, 2, 2, 2, 2, 2, 2, 2, 2, 2, 2, 2, 2, 2, 2, 2, 2, 2, 2, 2, 2, 2, 2, 2, 2, 2, 2, 2, 2, 2, 2, 2, 2, 2, 2, 2, 2, 2, 2, 2, 2, 2, 2, 2, 2, 2, 2, 2, 2, 2, 2, 2, 2, 2, 2, 2, 2, 2, 2, 2, 2, 2, 2, 2, 2, 2, 2, 2, 2, 2, 2, 2, 2, 2, 2, 2, 2, 2, 2, 2, 2, 2, 2, 2, 2, 2, 2, 2, 2, 2, 2, 2, 2, 2, 2, 2, 2, 2, 2, 2, 2, 2, 2, 2, 2, 2, 2, 2, 2, 2, 2, 2, 2, 2, 2, 2, 2, 2, 2, 2, 2, 2, 2, 2, 2, 2, 2, 2, 2, 2, 2, 2, 2, 2, 2, 2, 2, 2, 2, 2, 2, 2, 2, 2, 2, 2, 2, 2, 2, 2, 2, 2, 2, 2, 2, 2, 2, 2, 2, 2, 2, 2, 2, 2, 2, 2, 2, 2, 2, 2, 2, 2, 2, 2, 2, 2, 2, 2, 2, 2, 2, 2, 2, 2, 2, 2, 2, 2, 2, 2, 2, 2, 2, 2, 2, 2, 2, 2, 2, 2, 2, 2, 2, 2, 2, 2, 2, 2, 2, 2, 2, 2, 2, 2, 2, 2, 2, 2, 2, 2, 2, 2, 2, 2, 2, 2, 2, 2, 2, 2, 2, 2, 2, 2, 2, 2, 2, 2, 2, 2, 2, 2, 2, 2, 2, 2, 2, 2, 2, 2, 2, 2, 2, 2, 2, 2, 2, 2, 2, 2, 2, 2, 2, 2, 2, 2, 2, 2, 2, 2, 2, 2, 2, 2, 2, 2, 2, 2, 2, 2, 2, 2, 2, 2, 2, 2, 2, 2, 2, 2, 2, 2, 2, 2, 2, 2, 2, 2, 2, 2, 2, 2, 2, 2, 2, 2, 2, 2, 2, 2, 2, 2, 2, 2, 2, 2, 2, 2, 2, 2, 2, 2, 3 ),
 ( 0.000000000000000000, 1.000000000000000000 ),
 ( 0.000000000000000000, 0.002777777777777777884, 0.005555555555555555768, 0.008333333333333333218, 0.01111111111111111154, 0.01388888888888888812, 0.01666666666666666644, 0.01944444444444444475, 0.02222222222222222307, 0.02500000000000000139, 0.02777777777777777624, 0.03055555555555555455, 0.03333333333333333287, 0.03611111111111110772, 0.03888888888888888951, 0.04166666666666666435, 0.04444444444444444614, 0.04722222222222222099, 0.05000000000000000278, 0.05277777777777777762, 0.05555555555555555247, 0.05833333333333333426, 0.06111111111111110911, 0.06388888888888888395, 0.06666666666666666574, 0.06944444444444444753, 0.07222222222222221544, 0.07499999999999999722, 0.07777777777777777901, 0.08055555555555556080, 0.08333333333333332871, 0.08611111111111111049, 0.08888888888888889228, 0.09166666666666666019, 0.09444444444444444198, 0.09722222222222222376, 0.1000000000000000056, 0.1027777777777777735, 0.1055555555555555552, 0.1083333333333333370, 0.1111111111111111049, 0.1138888888888888867, 0.1166666666666666685, 0.1194444444444444503, 0.1222222222222222182, 0.1250000000000000000, 0.1277777777777777679, 0.1305555555555555636, 0.1333333333333333315, 0.1361111111111110994, 0.1388888888888888951, 0.1416666666666666630, 0.1444444444444444309, 0.1472222222222222265, 0.1499999999999999944, 0.1527777777777777901, 0.1555555555555555580, 0.1583333333333333259, 0.1611111111111111216, 0.1638888888888888895, 0.1666666666666666574, 0.1694444444444444531, 0.1722222222222222210, 0.1749999999999999889, 0.1777777777777777846, 0.1805555555555555525, 0.1833333333333333204, 0.1861111111111111160, 0.1888888888888888840, 0.1916666666666666796, 0.1944444444444444475, 0.1972222222222222154, 0.2000000000000000111, 0.2027777777777777790, 0.2055555555555555469, 0.2083333333333333426, 0.2111111111111111105, 0.2138888888888888784, 0.2166666666666666741, 0.2194444444444444420, 0.2222222222222222099, 0.2250000000000000056, 0.2277777777777777735, 0.2305555555555555691, 0.2333333333333333370, 0.2361111111111111049, 0.2388888888888889006, 0.2416666666666666685, 0.2444444444444444364, 0.2472222222222222321, 0.2500000000000000000, 0.2527777777777777679, 0.2555555555555555358, 0.2583333333333333592, 0.2611111111111111271, 0.2638888888888888951, 0.2666666666666666630, 0.2694444444444444309, 0.2722222222222221988, 0.2750000000000000222, 0.2777777777777777901, 0.2805555555555555580, 0.2833333333333333259, 0.2861111111111110938, 0.2888888888888888618, 0.2916666666666666852, 0.2944444444444444531, 0.2972222222222222210, 0.2999999999999999889, 0.3027777777777777568, 0.3055555555555555802, 0.3083333333333333481, 0.3111111111111111160, 0.3138888888888888840, 0.3166666666666666519, 0.3194444444444444198, 0.3222222222222222432, 0.3250000000000000111, 0.3277777777777777790, 0.3305555555555555469, 0.3333333333333333148, 0.3361111111111111382, 0.3388888888888889062, 0.3416666666666666741, 0.3444444444444444420, 0.3472222222222222099, 0.3499999999999999778, 0.3527777777777778012, 0.3555555555555555691, 0.3583333333333333370, 0.3611111111111111049, 0.3638888888888888729, 0.3666666666666666408, 0.3694444444444444642, 0.3722222222222222321, 0.3750000000000000000, 0.3777777777777777679, 0.3805555555555555358, 0.3833333333333333592, 0.3861111111111111271, 0.3888888888888888951, 0.3916666666666666630, 0.3944444444444444309, 0.3972222222222221988, 0.4000000000000000222, 0.4027777777777777901, 0.4055555555555555580, 0.4083333333333333259, 0.4111111111111110938, 0.4138888888888888618, 0.4166666666666666852, 0.4194444444444444531, 0.4222222222222222210, 0.4249999999999999889, 0.4277777777777777568, 0.4305555555555555802, 0.4333333333333333481, 0.4361111111111111160, 0.4388888888888888840, 0.4416666666666666519, 0.4444444444444444198, 0.4472222222222222432, 0.4500000000000000111, 0.4527777777777777790, 0.4555555555555555469, 0.4583333333333333148, 0.4611111111111111382, 0.4638888888888889062, 0.4666666666666666741, 0.4694444444444444420, 0.4722222222222222099, 0.4749999999999999778, 0.4777777777777778012, 0.4805555555555555691, 0.4833333333333333370, 0.4861111111111111049, 0.4888888888888888729, 0.4916666666666666408, 0.4944444444444444642, 0.4972222222222222321, 0.5000000000000000000, 0.5027777777777777679, 0.5055555555555555358, 0.5083333333333333037, 0.5111111111111110716, 0.5138888888888888395, 0.5166666666666667185, 0.5194444444444444864, 0.5222222222222222543, 0.5250000000000000222, 0.5277777777777777901, 0.5305555555555555580, 0.5333333333333333259, 0.5361111111111110938, 0.5388888888888888618, 0.5416666666666666297, 0.5444444444444443976, 0.5472222222222222765, 0.5500000000000000444, 0.5527777777777778123, 0.5555555555555555802, 0.5583333333333333481, 0.5611111111111111160, 0.5638888888888888840, 0.5666666666666666519, 0.5694444444444444198, 0.5722222222222221877, 0.5749999999999999556, 0.5777777777777777235, 0.5805555555555556024, 0.5833333333333333703, 0.5861111111111111382, 0.5888888888888889062, 0.5916666666666666741, 0.5944444444444444420, 0.5972222222222222099, 0.5999999999999999778, 0.6027777777777777457, 0.6055555555555555136, 0.6083333333333332815, 0.6111111111111111605, 0.6138888888888889284, 0.6166666666666666963, 0.6194444444444444642, 0.6222222222222222321, 0.6250000000000000000, 0.6277777777777777679, 0.6305555555555555358, 0.6333333333333333037, 0.6361111111111110716, 0.6388888888888888395, 0.6416666666666667185, 0.6444444444444444864, 0.6472222222222222543, 0.6500000000000000222, 0.6527777777777777901, 0.6555555555555555580, 0.6583333333333333259, 0.6611111111111110938, 0.6638888888888888618, 0.6666666666666666297, 0.6694444444444443976, 0.6722222222222222765, 0.6750000000000000444, 0.6777777777777778123, 0.6805555555555555802, 0.6833333333333333481, 0.6861111111111111160, 0.6888888888888888840, 0.6916666666666666519, 0.6944444444444444198, 0.6972222222222221877, 0.6999999999999999556, 0.7027777777777777235, 0.7055555555555556024, 0.7083333333333333703, 0.7111111111111111382, 0.7138888888888889062, 0.7166666666666666741, 0.7194444444444444420, 0.7222222222222222099, 0.7249999999999999778, 0.7277777777777777457, 0.7305555555555555136, 0.7333333333333332815, 0.7361111111111111605, 0.7388888888888889284, 0.7416666666666666963, 0.7444444444444444642, 0.7472222222222222321, 0.7500000000000000000, 0.7527777777777777679, 0.7555555555555555358, 0.7583333333333333037, 0.7611111111111110716, 0.7638888888888888395, 0.7666666666666667185, 0.7694444444444444864, 0.7722222222222222543, 0.7750000000000000222, 0.7777777777777777901, 0.7805555555555555580, 0.7833333333333333259, 0.7861111111111110938, 0.7888888888888888618, 0.7916666666666666297, 0.7944444444444443976, 0.7972222222222222765, 0.8000000000000000444, 0.8027777777777778123, 0.8055555555555555802, 0.8083333333333333481, 0.8111111111111111160, 0.8138888888888888840, 0.8166666666666666519, 0.8194444444444444198, 0.8222222222222221877, 0.8249999999999999556, 0.8277777777777777235, 0.8305555555555556024, 0.8333333333333333703, 0.8361111111111111382, 0.8388888888888889062, 0.8416666666666666741, 0.8444444444444444420, 0.8472222222222222099, 0.8499999999999999778, 0.8527777777777777457, 0.8555555555555555136, 0.8583333333333332815, 0.8611111111111111605, 0.8638888888888889284, 0.8666666666666666963, 0.8694444444444444642, 0.8722222222222222321, 0.8750000000000000000, 0.8777777777777777679, 0.8805555555555555358, 0.8833333333333333037, 0.8861111111111110716, 0.8888888888888888395, 0.8916666666666667185, 0.8944444444444444864, 0.8972222222222222543, 0.9000000000000000222, 0.9027777777777777901, 0.9055555555555555580, 0.9083333333333333259, 0.9111111111111110938, 0.9138888888888888618, 0.9166666666666666297, 0.9194444444444443976, 0.9222222222222222765, 0.9250000000000000444, 0.9277777777777778123, 0.9305555555555555802, 0.9333333333333333481, 0.9361111111111111160, 0.9388888888888888840, 0.9416666666666666519, 0.9444444444444444198, 0.9472222222222221877, 0.9499999999999999556, 0.9527777777777777235, 0.9555555555555556024, 0.9583333333333333703, 0.9611111111111111382, 0.9638888888888889062, 0.9666666666666666741, 0.9694444444444444420, 0.9722222222222222099, 0.9749999999999999778, 0.9777777777777777457, 0.9805555555555555136, 0.9833333333333332815, 0.9861111111111111605, 0.9888888888888889284, 0.9916666666666666963, 0.9944444444444444642, 0.9972222222222222321, 1.000000000000000000 ),
 .UNSPECIFIED. ) 
 GEOMETRIC_REPRESENTATION_ITEM ( )  RATIONAL_B_SPLINE_SURFACE ( (
 ( 1.000000000000000000, 0.8660254037844387076, 1.000000000000000000, 0.8660254037844387076, 1.000000000000000000, 0.8660254037844387076, 1.000000000000000000, 0.8660254037844387076, 1.000000000000000000, 0.8660254037844387076, 1.000000000000000000, 0.8660254037844387076, 1.000000000000000000, 0.8660254037844387076, 1.000000000000000000, 0.8660254037844387076, 1.000000000000000000, 0.8660254037844387076, 1.000000000000000000, 0.8660254037844387076, 1.000000000000000000, 0.8660254037844387076, 1.000000000000000000, 0.8660254037844387076, 1.000000000000000000, 0.8660254037844387076, 1.000000000000000000, 0.8660254037844387076, 1.000000000000000000, 0.8660254037844387076, 1.000000000000000000, 0.8660254037844387076, 1.000000000000000000, 0.8660254037844387076, 1.000000000000000000, 0.8660254037844387076, 1.000000000000000000, 0.8660254037844387076, 1.000000000000000000, 0.8660254037844387076, 1.000000000000000000, 0.8660254037844387076, 1.000000000000000000, 0.8660254037844387076, 1.000000000000000000, 0.8660254037844387076, 1.000000000000000000, 0.8660254037844387076, 1.000000000000000000, 0.8660254037844387076, 1.000000000000000000, 0.8660254037844387076, 1.000000000000000000, 0.8660254037844387076, 1.000000000000000000, 0.8660254037844387076, 1.000000000000000000, 0.8660254037844387076, 1.000000000000000000, 0.8660254037844387076, 1.000000000000000000, 0.8660254037844387076, 1.000000000000000000, 0.8660254037844387076, 1.000000000000000000, 0.8660254037844387076, 1.000000000000000000, 0.8660254037844387076, 1.000000000000000000, 0.8660254037844387076, 1.000000000000000000, 0.8660254037844387076, 1.000000000000000000, 0.8660254037844387076, 1.000000000000000000, 0.8660254037844387076, 1.000000000000000000, 0.8660254037844387076, 1.000000000000000000, 0.8660254037844387076, 1.000000000000000000, 0.8660254037844387076, 1.000000000000000000, 0.8660254037844387076, 1.000000000000000000, 0.8660254037844387076, 1.000000000000000000, 0.8660254037844387076, 1.000000000000000000, 0.8660254037844387076, 1.000000000000000000, 0.8660254037844387076, 1.000000000000000000, 0.8660254037844387076, 1.000000000000000000, 0.8660254037844387076, 1.000000000000000000, 0.8660254037844387076, 1.000000000000000000, 0.8660254037844387076, 1.000000000000000000, 0.8660254037844387076, 1.000000000000000000, 0.8660254037844387076, 1.000000000000000000, 0.8660254037844387076, 1.000000000000000000, 0.8660254037844387076, 1.000000000000000000, 0.8660254037844387076, 1.000000000000000000, 0.8660254037844387076, 1.000000000000000000, 0.8660254037844387076, 1.000000000000000000, 0.8660254037844387076, 1.000000000000000000, 0.8660254037844387076, 1.000000000000000000, 0.8660254037844387076, 1.000000000000000000, 0.8660254037844387076, 1.000000000000000000, 0.8660254037844387076, 1.000000000000000000, 0.8660254037844387076, 1.000000000000000000, 0.8660254037844387076, 1.000000000000000000, 0.8660254037844387076, 1.000000000000000000, 0.8660254037844387076, 1.000000000000000000, 0.8660254037844387076, 1.000000000000000000, 0.8660254037844387076, 1.000000000000000000, 0.8660254037844387076, 1.000000000000000000, 0.8660254037844387076, 1.000000000000000000, 0.8660254037844387076, 1.000000000000000000, 0.8660254037844387076, 1.000000000000000000, 0.8660254037844387076, 1.000000000000000000, 0.8660254037844387076, 1.000000000000000000, 0.8660254037844387076, 1.000000000000000000, 0.8660254037844387076, 1.000000000000000000, 0.8660254037844387076, 1.000000000000000000, 0.8660254037844387076, 1.000000000000000000, 0.8660254037844387076, 1.000000000000000000, 0.8660254037844387076, 1.000000000000000000, 0.8660254037844387076, 1.000000000000000000, 0.8660254037844387076, 1.000000000000000000, 0.8660254037844387076, 1.000000000000000000, 0.8660254037844387076, 1.000000000000000000, 0.8660254037844387076, 1.000000000000000000, 0.8660254037844387076, 1.000000000000000000, 0.8660254037844387076, 1.000000000000000000, 0.8660254037844387076, 1.000000000000000000, 0.8660254037844387076, 1.000000000000000000, 0.8660254037844387076, 1.000000000000000000, 0.8660254037844387076, 1.000000000000000000, 0.8660254037844387076, 1.000000000000000000, 0.8660254037844387076, 1.000000000000000000, 0.8660254037844387076, 1.000000000000000000, 0.8660254037844387076, 1.000000000000000000, 0.8660254037844387076, 1.000000000000000000, 0.8660254037844387076, 1.000000000000000000, 0.8660254037844387076, 1.000000000000000000, 0.8660254037844387076, 1.000000000000000000, 0.8660254037844387076, 1.000000000000000000, 0.8660254037844387076, 1.000000000000000000, 0.8660254037844387076, 1.000000000000000000, 0.8660254037844387076, 1.000000000000000000, 0.8660254037844387076, 1.000000000000000000, 0.8660254037844387076, 1.000000000000000000, 0.8660254037844387076, 1.000000000000000000, 0.8660254037844387076, 1.000000000000000000, 0.8660254037844387076, 1.000000000000000000, 0.8660254037844387076, 1.000000000000000000, 0.8660254037844387076, 1.000000000000000000, 0.8660254037844387076, 1.000000000000000000, 0.8660254037844387076, 1.000000000000000000, 0.8660254037844387076, 1.000000000000000000, 0.8660254037844387076, 1.000000000000000000, 0.8660254037844387076, 1.000000000000000000, 0.8660254037844387076, 1.000000000000000000, 0.8660254037844387076, 1.000000000000000000, 0.8660254037844387076, 1.000000000000000000, 0.8660254037844387076, 1.000000000000000000, 0.8660254037844387076, 1.000000000000000000, 0.8660254037844387076, 1.000000000000000000, 0.8660254037844387076, 1.000000000000000000, 0.8660254037844387076, 1.000000000000000000, 0.8660254037844387076, 1.000000000000000000, 0.8660254037844387076, 1.000000000000000000, 0.8660254037844387076, 1.000000000000000000, 0.8660254037844387076, 1.000000000000000000, 0.8660254037844387076, 1.000000000000000000, 0.8660254037844387076, 1.000000000000000000, 0.8660254037844387076, 1.000000000000000000, 0.8660254037844387076, 1.000000000000000000, 0.8660254037844387076, 1.000000000000000000, 0.8660254037844387076, 1.000000000000000000, 0.8660254037844387076, 1.000000000000000000, 0.8660254037844387076, 1.000000000000000000, 0.8660254037844387076, 1.000000000000000000, 0.8660254037844387076, 1.000000000000000000, 0.8660254037844387076, 1.000000000000000000, 0.8660254037844387076, 1.000000000000000000, 0.8660254037844387076, 1.000000000000000000, 0.8660254037844387076, 1.000000000000000000, 0.8660254037844387076, 1.000000000000000000, 0.8660254037844387076, 1.000000000000000000, 0.8660254037844387076, 1.000000000000000000, 0.8660254037844387076, 1.000000000000000000, 0.8660254037844387076, 1.000000000000000000, 0.8660254037844387076, 1.000000000000000000, 0.8660254037844387076, 1.000000000000000000, 0.8660254037844387076, 1.000000000000000000, 0.8660254037844387076, 1.000000000000000000, 0.8660254037844387076, 1.000000000000000000, 0.8660254037844387076, 1.000000000000000000, 0.8660254037844387076, 1.000000000000000000, 0.8660254037844387076, 1.000000000000000000, 0.8660254037844387076, 1.000000000000000000, 0.8660254037844387076, 1.000000000000000000, 0.8660254037844387076, 1.000000000000000000, 0.8660254037844387076, 1.000000000000000000, 0.8660254037844387076, 1.000000000000000000, 0.8660254037844387076, 1.000000000000000000, 0.8660254037844387076, 1.000000000000000000, 0.8660254037844387076, 1.000000000000000000, 0.8660254037844387076, 1.000000000000000000, 0.8660254037844387076, 1.000000000000000000, 0.8660254037844387076, 1.000000000000000000, 0.8660254037844387076, 1.000000000000000000, 0.8660254037844387076, 1.000000000000000000, 0.8660254037844387076, 1.000000000000000000, 0.8660254037844387076, 1.000000000000000000, 0.8660254037844387076, 1.000000000000000000, 0.8660254037844387076, 1.000000000000000000, 0.8660254037844387076, 1.000000000000000000, 0.8660254037844387076, 1.000000000000000000, 0.8660254037844387076, 1.000000000000000000, 0.8660254037844387076, 1.000000000000000000, 0.8660254037844387076, 1.000000000000000000, 0.8660254037844387076, 1.000000000000000000, 0.8660254037844387076, 1.000000000000000000, 0.8660254037844387076, 1.000000000000000000, 0.8660254037844387076, 1.000000000000000000, 0.8660254037844387076, 1.000000000000000000, 0.8660254037844387076, 1.000000000000000000, 0.8660254037844387076, 1.000000000000000000, 0.8660254037844387076, 1.000000000000000000, 0.8660254037844387076, 1.000000000000000000, 0.8660254037844387076, 1.000000000000000000, 0.8660254037844387076, 1.000000000000000000, 0.8660254037844387076, 1.000000000000000000, 0.8660254037844387076, 1.000000000000000000, 0.8660254037844387076, 1.000000000000000000, 0.8660254037844387076, 1.000000000000000000, 0.8660254037844387076, 1.000000000000000000, 0.8660254037844387076, 1.000000000000000000, 0.8660254037844387076, 1.000000000000000000, 0.8660254037844387076, 1.000000000000000000, 0.8660254037844387076, 1.000000000000000000, 0.8660254037844387076, 1.000000000000000000, 0.8660254037844387076, 1.000000000000000000, 0.8660254037844387076, 1.000000000000000000, 0.8660254037844387076, 1.000000000000000000, 0.8660254037844387076, 1.000000000000000000, 0.8660254037844387076, 1.000000000000000000, 0.8660254037844387076, 1.000000000000000000, 0.8660254037844387076, 1.000000000000000000, 0.8660254037844387076, 1.000000000000000000, 0.8660254037844387076, 1.000000000000000000, 0.8660254037844387076, 1.000000000000000000, 0.8660254037844387076, 1.000000000000000000, 0.8660254037844387076, 1.000000000000000000, 0.8660254037844387076, 1.000000000000000000, 0.8660254037844387076, 1.000000000000000000, 0.8660254037844387076, 1.000000000000000000, 0.8660254037844387076, 1.000000000000000000, 0.8660254037844387076, 1.000000000000000000, 0.8660254037844387076, 1.000000000000000000, 0.8660254037844387076, 1.000000000000000000, 0.8660254037844387076, 1.000000000000000000, 0.8660254037844387076, 1.000000000000000000, 0.8660254037844387076, 1.000000000000000000, 0.8660254037844387076, 1.000000000000000000, 0.8660254037844387076, 1.000000000000000000, 0.8660254037844387076, 1.000000000000000000, 0.8660254037844387076, 1.000000000000000000, 0.8660254037844387076, 1.000000000000000000, 0.8660254037844387076, 1.000000000000000000, 0.8660254037844387076, 1.000000000000000000, 0.8660254037844387076, 1.000000000000000000, 0.8660254037844387076, 1.000000000000000000, 0.8660254037844387076, 1.000000000000000000, 0.8660254037844387076, 1.000000000000000000, 0.8660254037844387076, 1.000000000000000000, 0.8660254037844387076, 1.000000000000000000, 0.8660254037844387076, 1.000000000000000000, 0.8660254037844387076, 1.000000000000000000, 0.8660254037844387076, 1.000000000000000000, 0.8660254037844387076, 1.000000000000000000, 0.8660254037844387076, 1.000000000000000000, 0.8660254037844387076, 1.000000000000000000, 0.8660254037844387076, 1.000000000000000000, 0.8660254037844387076, 1.000000000000000000, 0.8660254037844387076, 1.000000000000000000, 0.8660254037844387076, 1.000000000000000000, 0.8660254037844387076, 1.000000000000000000, 0.8660254037844387076, 1.000000000000000000, 0.8660254037844387076, 1.000000000000000000, 0.8660254037844387076, 1.000000000000000000, 0.8660254037844387076, 1.000000000000000000, 0.8660254037844387076, 1.000000000000000000, 0.8660254037844387076, 1.000000000000000000, 0.8660254037844387076, 1.000000000000000000, 0.8660254037844387076, 1.000000000000000000, 0.8660254037844387076, 1.000000000000000000, 0.8660254037844387076, 1.000000000000000000, 0.8660254037844387076, 1.000000000000000000, 0.8660254037844387076, 1.000000000000000000, 0.8660254037844387076, 1.000000000000000000, 0.8660254037844387076, 1.000000000000000000, 0.8660254037844387076, 1.000000000000000000, 0.8660254037844387076, 1.000000000000000000, 0.8660254037844387076, 1.000000000000000000, 0.8660254037844387076, 1.000000000000000000, 0.8660254037844387076, 1.000000000000000000, 0.8660254037844387076, 1.000000000000000000, 0.8660254037844387076, 1.000000000000000000, 0.8660254037844387076, 1.000000000000000000, 0.8660254037844387076, 1.000000000000000000, 0.8660254037844387076, 1.000000000000000000, 0.8660254037844387076, 1.000000000000000000, 0.8660254037844387076, 1.000000000000000000, 0.8660254037844387076, 1.000000000000000000, 0.8660254037844387076, 1.000000000000000000, 0.8660254037844387076, 1.000000000000000000, 0.8660254037844387076, 1.000000000000000000, 0.8660254037844387076, 1.000000000000000000, 0.8660254037844387076, 1.000000000000000000, 0.8660254037844387076, 1.000000000000000000, 0.8660254037844387076, 1.000000000000000000, 0.8660254037844387076, 1.000000000000000000, 0.8660254037844387076, 1.000000000000000000, 0.8660254037844387076, 1.000000000000000000, 0.8660254037844387076, 1.000000000000000000, 0.8660254037844387076, 1.000000000000000000, 0.8660254037844387076, 1.000000000000000000, 0.8660254037844387076, 1.000000000000000000, 0.8660254037844387076, 1.000000000000000000, 0.8660254037844387076, 1.000000000000000000, 0.8660254037844387076, 1.000000000000000000, 0.8660254037844387076, 1.000000000000000000, 0.8660254037844387076, 1.000000000000000000, 0.8660254037844387076, 1.000000000000000000, 0.8660254037844387076, 1.000000000000000000, 0.8660254037844387076, 1.000000000000000000, 0.8660254037844387076, 1.000000000000000000, 0.8660254037844387076, 1.000000000000000000, 0.8660254037844387076, 1.000000000000000000, 0.8660254037844387076, 1.000000000000000000, 0.8660254037844387076, 1.000000000000000000, 0.8660254037844387076, 1.000000000000000000, 0.8660254037844387076, 1.000000000000000000, 0.8660254037844387076, 1.000000000000000000, 0.8660254037844387076, 1.000000000000000000, 0.8660254037844387076, 1.000000000000000000, 0.8660254037844387076, 1.000000000000000000, 0.8660254037844387076, 1.000000000000000000, 0.8660254037844387076, 1.000000000000000000, 0.8660254037844387076, 1.000000000000000000, 0.8660254037844387076, 1.000000000000000000, 0.8660254037844387076, 1.000000000000000000, 0.8660254037844387076, 1.000000000000000000, 0.8660254037844387076, 1.000000000000000000, 0.8660254037844387076, 1.000000000000000000, 0.8660254037844387076, 1.000000000000000000, 0.8660254037844387076, 1.000000000000000000, 0.8660254037844387076, 1.000000000000000000, 0.8660254037844387076, 1.000000000000000000, 0.8660254037844387076, 1.000000000000000000, 0.8660254037844387076, 1.000000000000000000, 0.8660254037844387076, 1.000000000000000000, 0.8660254037844387076, 1.000000000000000000, 0.8660254037844387076, 1.000000000000000000, 0.8660254037844387076, 1.000000000000000000, 0.8660254037844387076, 1.000000000000000000, 0.8660254037844387076, 1.000000000000000000, 0.8660254037844387076, 1.000000000000000000, 0.8660254037844387076, 1.000000000000000000, 0.8660254037844387076, 1.000000000000000000, 0.8660254037844387076, 1.000000000000000000, 0.8660254037844387076, 1.000000000000000000, 0.8660254037844387076, 1.000000000000000000, 0.8660254037844387076, 1.000000000000000000, 0.8660254037844387076, 1.000000000000000000, 0.8660254037844387076, 1.000000000000000000, 0.8660254037844387076, 1.000000000000000000, 0.8660254037844387076, 1.000000000000000000, 0.8660254037844387076, 1.000000000000000000, 0.8660254037844387076, 1.000000000000000000, 0.8660254037844387076, 1.000000000000000000, 0.8660254037844387076, 1.000000000000000000, 0.8660254037844387076, 1.000000000000000000, 0.8660254037844387076, 1.000000000000000000, 0.8660254037844387076, 1.000000000000000000, 0.8660254037844387076, 1.000000000000000000, 0.8660254037844387076, 1.000000000000000000, 0.8660254037844387076, 1.000000000000000000, 0.8660254037844387076, 1.000000000000000000, 0.8660254037844387076, 1.000000000000000000, 0.8660254037844387076, 1.000000000000000000, 0.8660254037844387076, 1.000000000000000000, 0.8660254037844387076, 1.000000000000000000, 0.8660254037844387076, 1.000000000000000000, 0.8660254037844387076, 1.000000000000000000, 0.8660254037844387076, 1.000000000000000000, 0.8660254037844387076, 1.000000000000000000, 0.8660254037844387076, 1.000000000000000000, 0.8660254037844387076, 1.000000000000000000, 0.8660254037844387076, 1.000000000000000000, 0.8660254037844387076, 1.000000000000000000, 0.8660254037844387076, 1.000000000000000000, 0.8660254037844387076, 1.000000000000000000, 0.8660254037844387076, 1.000000000000000000),
 ( 1.000000000000000000, 0.8660254037844387076, 1.000000000000000000, 0.8660254037844387076, 1.000000000000000000, 0.8660254037844387076, 1.000000000000000000, 0.8660254037844387076, 1.000000000000000000, 0.8660254037844387076, 1.000000000000000000, 0.8660254037844387076, 1.000000000000000000, 0.8660254037844387076, 1.000000000000000000, 0.8660254037844387076, 1.000000000000000000, 0.8660254037844387076, 1.000000000000000000, 0.8660254037844387076, 1.000000000000000000, 0.8660254037844387076, 1.000000000000000000, 0.8660254037844387076, 1.000000000000000000, 0.8660254037844387076, 1.000000000000000000, 0.8660254037844387076, 1.000000000000000000, 0.8660254037844387076, 1.000000000000000000, 0.8660254037844387076, 1.000000000000000000, 0.8660254037844387076, 1.000000000000000000, 0.8660254037844387076, 1.000000000000000000, 0.8660254037844387076, 1.000000000000000000, 0.8660254037844387076, 1.000000000000000000, 0.8660254037844387076, 1.000000000000000000, 0.8660254037844387076, 1.000000000000000000, 0.8660254037844387076, 1.000000000000000000, 0.8660254037844387076, 1.000000000000000000, 0.8660254037844387076, 1.000000000000000000, 0.8660254037844387076, 1.000000000000000000, 0.8660254037844387076, 1.000000000000000000, 0.8660254037844387076, 1.000000000000000000, 0.8660254037844387076, 1.000000000000000000, 0.8660254037844387076, 1.000000000000000000, 0.8660254037844387076, 1.000000000000000000, 0.8660254037844387076, 1.000000000000000000, 0.8660254037844387076, 1.000000000000000000, 0.8660254037844387076, 1.000000000000000000, 0.8660254037844387076, 1.000000000000000000, 0.8660254037844387076, 1.000000000000000000, 0.8660254037844387076, 1.000000000000000000, 0.8660254037844387076, 1.000000000000000000, 0.8660254037844387076, 1.000000000000000000, 0.8660254037844387076, 1.000000000000000000, 0.8660254037844387076, 1.000000000000000000, 0.8660254037844387076, 1.000000000000000000, 0.8660254037844387076, 1.000000000000000000, 0.8660254037844387076, 1.000000000000000000, 0.8660254037844387076, 1.000000000000000000, 0.8660254037844387076, 1.000000000000000000, 0.8660254037844387076, 1.000000000000000000, 0.8660254037844387076, 1.000000000000000000, 0.8660254037844387076, 1.000000000000000000, 0.8660254037844387076, 1.000000000000000000, 0.8660254037844387076, 1.000000000000000000, 0.8660254037844387076, 1.000000000000000000, 0.8660254037844387076, 1.000000000000000000, 0.8660254037844387076, 1.000000000000000000, 0.8660254037844387076, 1.000000000000000000, 0.8660254037844387076, 1.000000000000000000, 0.8660254037844387076, 1.000000000000000000, 0.8660254037844387076, 1.000000000000000000, 0.8660254037844387076, 1.000000000000000000, 0.8660254037844387076, 1.000000000000000000, 0.8660254037844387076, 1.000000000000000000, 0.8660254037844387076, 1.000000000000000000, 0.8660254037844387076, 1.000000000000000000, 0.8660254037844387076, 1.000000000000000000, 0.8660254037844387076, 1.000000000000000000, 0.8660254037844387076, 1.000000000000000000, 0.8660254037844387076, 1.000000000000000000, 0.8660254037844387076, 1.000000000000000000, 0.8660254037844387076, 1.000000000000000000, 0.8660254037844387076, 1.000000000000000000, 0.8660254037844387076, 1.000000000000000000, 0.8660254037844387076, 1.000000000000000000, 0.8660254037844387076, 1.000000000000000000, 0.8660254037844387076, 1.000000000000000000, 0.8660254037844387076, 1.000000000000000000, 0.8660254037844387076, 1.000000000000000000, 0.8660254037844387076, 1.000000000000000000, 0.8660254037844387076, 1.000000000000000000, 0.8660254037844387076, 1.000000000000000000, 0.8660254037844387076, 1.000000000000000000, 0.8660254037844387076, 1.000000000000000000, 0.8660254037844387076, 1.000000000000000000, 0.8660254037844387076, 1.000000000000000000, 0.8660254037844387076, 1.000000000000000000, 0.8660254037844387076, 1.000000000000000000, 0.8660254037844387076, 1.000000000000000000, 0.8660254037844387076, 1.000000000000000000, 0.8660254037844387076, 1.000000000000000000, 0.8660254037844387076, 1.000000000000000000, 0.8660254037844387076, 1.000000000000000000, 0.8660254037844387076, 1.000000000000000000, 0.8660254037844387076, 1.000000000000000000, 0.8660254037844387076, 1.000000000000000000, 0.8660254037844387076, 1.000000000000000000, 0.8660254037844387076, 1.000000000000000000, 0.8660254037844387076, 1.000000000000000000, 0.8660254037844387076, 1.000000000000000000, 0.8660254037844387076, 1.000000000000000000, 0.8660254037844387076, 1.000000000000000000, 0.8660254037844387076, 1.000000000000000000, 0.8660254037844387076, 1.000000000000000000, 0.8660254037844387076, 1.000000000000000000, 0.8660254037844387076, 1.000000000000000000, 0.8660254037844387076, 1.000000000000000000, 0.8660254037844387076, 1.000000000000000000, 0.8660254037844387076, 1.000000000000000000, 0.8660254037844387076, 1.000000000000000000, 0.8660254037844387076, 1.000000000000000000, 0.8660254037844387076, 1.000000000000000000, 0.8660254037844387076, 1.000000000000000000, 0.8660254037844387076, 1.000000000000000000, 0.8660254037844387076, 1.000000000000000000, 0.8660254037844387076, 1.000000000000000000, 0.8660254037844387076, 1.000000000000000000, 0.8660254037844387076, 1.000000000000000000, 0.8660254037844387076, 1.000000000000000000, 0.8660254037844387076, 1.000000000000000000, 0.8660254037844387076, 1.000000000000000000, 0.8660254037844387076, 1.000000000000000000, 0.8660254037844387076, 1.000000000000000000, 0.8660254037844387076, 1.000000000000000000, 0.8660254037844387076, 1.000000000000000000, 0.8660254037844387076, 1.000000000000000000, 0.8660254037844387076, 1.000000000000000000, 0.8660254037844387076, 1.000000000000000000, 0.8660254037844387076, 1.000000000000000000, 0.8660254037844387076, 1.000000000000000000, 0.8660254037844387076, 1.000000000000000000, 0.8660254037844387076, 1.000000000000000000, 0.8660254037844387076, 1.000000000000000000, 0.8660254037844387076, 1.000000000000000000, 0.8660254037844387076, 1.000000000000000000, 0.8660254037844387076, 1.000000000000000000, 0.8660254037844387076, 1.000000000000000000, 0.8660254037844387076, 1.000000000000000000, 0.8660254037844387076, 1.000000000000000000, 0.8660254037844387076, 1.000000000000000000, 0.8660254037844387076, 1.000000000000000000, 0.8660254037844387076, 1.000000000000000000, 0.8660254037844387076, 1.000000000000000000, 0.8660254037844387076, 1.000000000000000000, 0.8660254037844387076, 1.000000000000000000, 0.8660254037844387076, 1.000000000000000000, 0.8660254037844387076, 1.000000000000000000, 0.8660254037844387076, 1.000000000000000000, 0.8660254037844387076, 1.000000000000000000, 0.8660254037844387076, 1.000000000000000000, 0.8660254037844387076, 1.000000000000000000, 0.8660254037844387076, 1.000000000000000000, 0.8660254037844387076, 1.000000000000000000, 0.8660254037844387076, 1.000000000000000000, 0.8660254037844387076, 1.000000000000000000, 0.8660254037844387076, 1.000000000000000000, 0.8660254037844387076, 1.000000000000000000, 0.8660254037844387076, 1.000000000000000000, 0.8660254037844387076, 1.000000000000000000, 0.8660254037844387076, 1.000000000000000000, 0.8660254037844387076, 1.000000000000000000, 0.8660254037844387076, 1.000000000000000000, 0.8660254037844387076, 1.000000000000000000, 0.8660254037844387076, 1.000000000000000000, 0.8660254037844387076, 1.000000000000000000, 0.8660254037844387076, 1.000000000000000000, 0.8660254037844387076, 1.000000000000000000, 0.8660254037844387076, 1.000000000000000000, 0.8660254037844387076, 1.000000000000000000, 0.8660254037844387076, 1.000000000000000000, 0.8660254037844387076, 1.000000000000000000, 0.8660254037844387076, 1.000000000000000000, 0.8660254037844387076, 1.000000000000000000, 0.8660254037844387076, 1.000000000000000000, 0.8660254037844387076, 1.000000000000000000, 0.8660254037844387076, 1.000000000000000000, 0.8660254037844387076, 1.000000000000000000, 0.8660254037844387076, 1.000000000000000000, 0.8660254037844387076, 1.000000000000000000, 0.8660254037844387076, 1.000000000000000000, 0.8660254037844387076, 1.000000000000000000, 0.8660254037844387076, 1.000000000000000000, 0.8660254037844387076, 1.000000000000000000, 0.8660254037844387076, 1.000000000000000000, 0.8660254037844387076, 1.000000000000000000, 0.8660254037844387076, 1.000000000000000000, 0.8660254037844387076, 1.000000000000000000, 0.8660254037844387076, 1.000000000000000000, 0.8660254037844387076, 1.000000000000000000, 0.8660254037844387076, 1.000000000000000000, 0.8660254037844387076, 1.000000000000000000, 0.8660254037844387076, 1.000000000000000000, 0.8660254037844387076, 1.000000000000000000, 0.8660254037844387076, 1.000000000000000000, 0.8660254037844387076, 1.000000000000000000, 0.8660254037844387076, 1.000000000000000000, 0.8660254037844387076, 1.000000000000000000, 0.8660254037844387076, 1.000000000000000000, 0.8660254037844387076, 1.000000000000000000, 0.8660254037844387076, 1.000000000000000000, 0.8660254037844387076, 1.000000000000000000, 0.8660254037844387076, 1.000000000000000000, 0.8660254037844387076, 1.000000000000000000, 0.8660254037844387076, 1.000000000000000000, 0.8660254037844387076, 1.000000000000000000, 0.8660254037844387076, 1.000000000000000000, 0.8660254037844387076, 1.000000000000000000, 0.8660254037844387076, 1.000000000000000000, 0.8660254037844387076, 1.000000000000000000, 0.8660254037844387076, 1.000000000000000000, 0.8660254037844387076, 1.000000000000000000, 0.8660254037844387076, 1.000000000000000000, 0.8660254037844387076, 1.000000000000000000, 0.8660254037844387076, 1.000000000000000000, 0.8660254037844387076, 1.000000000000000000, 0.8660254037844387076, 1.000000000000000000, 0.8660254037844387076, 1.000000000000000000, 0.8660254037844387076, 1.000000000000000000, 0.8660254037844387076, 1.000000000000000000, 0.8660254037844387076, 1.000000000000000000, 0.8660254037844387076, 1.000000000000000000, 0.8660254037844387076, 1.000000000000000000, 0.8660254037844387076, 1.000000000000000000, 0.8660254037844387076, 1.000000000000000000, 0.8660254037844387076, 1.000000000000000000, 0.8660254037844387076, 1.000000000000000000, 0.8660254037844387076, 1.000000000000000000, 0.8660254037844387076, 1.000000000000000000, 0.8660254037844387076, 1.000000000000000000, 0.8660254037844387076, 1.000000000000000000, 0.8660254037844387076, 1.000000000000000000, 0.8660254037844387076, 1.000000000000000000, 0.8660254037844387076, 1.000000000000000000, 0.8660254037844387076, 1.000000000000000000, 0.8660254037844387076, 1.000000000000000000, 0.8660254037844387076, 1.000000000000000000, 0.8660254037844387076, 1.000000000000000000, 0.8660254037844387076, 1.000000000000000000, 0.8660254037844387076, 1.000000000000000000, 0.8660254037844387076, 1.000000000000000000, 0.8660254037844387076, 1.000000000000000000, 0.8660254037844387076, 1.000000000000000000, 0.8660254037844387076, 1.000000000000000000, 0.8660254037844387076, 1.000000000000000000, 0.8660254037844387076, 1.000000000000000000, 0.8660254037844387076, 1.000000000000000000, 0.8660254037844387076, 1.000000000000000000, 0.8660254037844387076, 1.000000000000000000, 0.8660254037844387076, 1.000000000000000000, 0.8660254037844387076, 1.000000000000000000, 0.8660254037844387076, 1.000000000000000000, 0.8660254037844387076, 1.000000000000000000, 0.8660254037844387076, 1.000000000000000000, 0.8660254037844387076, 1.000000000000000000, 0.8660254037844387076, 1.000000000000000000, 0.8660254037844387076, 1.000000000000000000, 0.8660254037844387076, 1.000000000000000000, 0.8660254037844387076, 1.000000000000000000, 0.8660254037844387076, 1.000000000000000000, 0.8660254037844387076, 1.000000000000000000, 0.8660254037844387076, 1.000000000000000000, 0.8660254037844387076, 1.000000000000000000, 0.8660254037844387076, 1.000000000000000000, 0.8660254037844387076, 1.000000000000000000, 0.8660254037844387076, 1.000000000000000000, 0.8660254037844387076, 1.000000000000000000, 0.8660254037844387076, 1.000000000000000000, 0.8660254037844387076, 1.000000000000000000, 0.8660254037844387076, 1.000000000000000000, 0.8660254037844387076, 1.000000000000000000, 0.8660254037844387076, 1.000000000000000000, 0.8660254037844387076, 1.000000000000000000, 0.8660254037844387076, 1.000000000000000000, 0.8660254037844387076, 1.000000000000000000, 0.8660254037844387076, 1.000000000000000000, 0.8660254037844387076, 1.000000000000000000, 0.8660254037844387076, 1.000000000000000000, 0.8660254037844387076, 1.000000000000000000, 0.8660254037844387076, 1.000000000000000000, 0.8660254037844387076, 1.000000000000000000, 0.8660254037844387076, 1.000000000000000000, 0.8660254037844387076, 1.000000000000000000, 0.8660254037844387076, 1.000000000000000000, 0.8660254037844387076, 1.000000000000000000, 0.8660254037844387076, 1.000000000000000000, 0.8660254037844387076, 1.000000000000000000, 0.8660254037844387076, 1.000000000000000000, 0.8660254037844387076, 1.000000000000000000, 0.8660254037844387076, 1.000000000000000000, 0.8660254037844387076, 1.000000000000000000, 0.8660254037844387076, 1.000000000000000000, 0.8660254037844387076, 1.000000000000000000, 0.8660254037844387076, 1.000000000000000000, 0.8660254037844387076, 1.000000000000000000, 0.8660254037844387076, 1.000000000000000000, 0.8660254037844387076, 1.000000000000000000, 0.8660254037844387076, 1.000000000000000000, 0.8660254037844387076, 1.000000000000000000, 0.8660254037844387076, 1.000000000000000000, 0.8660254037844387076, 1.000000000000000000, 0.8660254037844387076, 1.000000000000000000, 0.8660254037844387076, 1.000000000000000000, 0.8660254037844387076, 1.000000000000000000, 0.8660254037844387076, 1.000000000000000000, 0.8660254037844387076, 1.000000000000000000, 0.8660254037844387076, 1.000000000000000000, 0.8660254037844387076, 1.000000000000000000, 0.8660254037844387076, 1.000000000000000000, 0.8660254037844387076, 1.000000000000000000, 0.8660254037844387076, 1.000000000000000000, 0.8660254037844387076, 1.000000000000000000, 0.8660254037844387076, 1.000000000000000000, 0.8660254037844387076, 1.000000000000000000, 0.8660254037844387076, 1.000000000000000000, 0.8660254037844387076, 1.000000000000000000, 0.8660254037844387076, 1.000000000000000000, 0.8660254037844387076, 1.000000000000000000, 0.8660254037844387076, 1.000000000000000000, 0.8660254037844387076, 1.000000000000000000, 0.8660254037844387076, 1.000000000000000000, 0.8660254037844387076, 1.000000000000000000, 0.8660254037844387076, 1.000000000000000000, 0.8660254037844387076, 1.000000000000000000, 0.8660254037844387076, 1.000000000000000000, 0.8660254037844387076, 1.000000000000000000, 0.8660254037844387076, 1.000000000000000000, 0.8660254037844387076, 1.000000000000000000, 0.8660254037844387076, 1.000000000000000000, 0.8660254037844387076, 1.000000000000000000, 0.8660254037844387076, 1.000000000000000000, 0.8660254037844387076, 1.000000000000000000, 0.8660254037844387076, 1.000000000000000000, 0.8660254037844387076, 1.000000000000000000, 0.8660254037844387076, 1.000000000000000000, 0.8660254037844387076, 1.000000000000000000, 0.8660254037844387076, 1.000000000000000000, 0.8660254037844387076, 1.000000000000000000, 0.8660254037844387076, 1.000000000000000000, 0.8660254037844387076, 1.000000000000000000, 0.8660254037844387076, 1.000000000000000000, 0.8660254037844387076, 1.000000000000000000, 0.8660254037844387076, 1.000000000000000000, 0.8660254037844387076, 1.000000000000000000, 0.8660254037844387076, 1.000000000000000000, 0.8660254037844387076, 1.000000000000000000, 0.8660254037844387076, 1.000000000000000000, 0.8660254037844387076, 1.000000000000000000, 0.8660254037844387076, 1.000000000000000000, 0.8660254037844387076, 1.000000000000000000, 0.8660254037844387076, 1.000000000000000000, 0.8660254037844387076, 1.000000000000000000, 0.8660254037844387076, 1.000000000000000000, 0.8660254037844387076, 1.000000000000000000, 0.8660254037844387076, 1.000000000000000000, 0.8660254037844387076, 1.000000000000000000, 0.8660254037844387076, 1.000000000000000000, 0.8660254037844387076, 1.000000000000000000, 0.8660254037844387076, 1.000000000000000000, 0.8660254037844387076, 1.000000000000000000, 0.8660254037844387076, 1.000000000000000000, 0.8660254037844387076, 1.000000000000000000, 0.8660254037844387076, 1.000000000000000000, 0.8660254037844387076, 1.000000000000000000) ) ) 
 REPRESENTATION_ITEM ( '' )  SURFACE ( )  );
#55766 = CARTESIAN_POINT ( 'NONE',  ( 8.775000000000002132, 4.330127018922191873, 2.499999999999999556 ) ) ;
#55767 = CARTESIAN_POINT ( 'NONE',  ( 7.771875000614516971, 3.027376345333611329, 5.243569643749999010 ) ) ;
#55768 = CARTESIAN_POINT ( 'NONE',  ( 6.262500001229034829, 0.000000000000000000, 4.999999999999998224 ) ) ;
#55769 = CARTESIAN_POINT ( 'NONE',  ( 12.64687500061451608, 6.054752690667223547, 3.707466751127219781E-16 ) ) ;
#55770 = CARTESIAN_POINT ( 'NONE',  ( 12.03750000122903430, 4.330127018922191873, 2.499999999999999556 ) ) ;
#55771 = CARTESIAN_POINT ( 'NONE',  ( 4.359375000614517326, -4.541064518000417216, -2.621784821875001281 ) ) ;
#55772 = CARTESIAN_POINT ( 'NONE',  ( 28.19999999999999929, 0.000000000000000000, 4.999999999999998224 ) ) ;
#55773 = DIRECTION ( 'NONE',  ( -1.000000000000000000, -0.000000000000000000, -0.000000000000000000 ) ) ;
#55774 = CARTESIAN_POINT ( 'NONE',  ( 9.121875000614517504, 3.027376345333611329, 5.243569643749999010 ) ) ;
#55775 = CARTESIAN_POINT ( 'NONE',  ( 3.600000000000002309, -4.330127018922190985, -2.500000000000001332 ) ) ;
#55776 = CARTESIAN_POINT ( 'NONE',  ( 19.30312500061451786, 4.541064518000418104, -2.621784821874998173 ) ) ;
#55777 = DIRECTION ( 'NONE',  ( 0.000000000000000000, 0.000000000000000000, -1.000000000000000000 ) ) ;
#55778 = CARTESIAN_POINT ( 'NONE',  ( -2.121784821874999949, 18.37812500061459531, 26.32496088578401938 ) ) ;
#55779 = CARTESIAN_POINT ( 'NONE',  ( 22.95937500061451431, 4.541064518000418104, -2.621784821874998173 ) ) ;
#55780 = CARTESIAN_POINT ( 'NONE',  ( -5.810221930991193690E-16, 13.70000000122903394, -34.00000000000000000 ) ) ;
#55781 =( BOUNDED_SURFACE ( )  B_SPLINE_SURFACE ( 1, 2, ( 
 ( #58888, #24913, #69275, #30101, #63359, #40841, #53735, #8298, #52998, #12743, #47826, #1678, #30828, #35639, #69631, #42283, #70356, #68910, #18268, #46741, #58161, #35279, #36732, #8662, #57801, #64807, #7565, #36002, #47456, #69989, #59254, #41555, #31193, #13454, #58521, #64441, #52636, #3128, #7931, #53361, #7210, #19359, #2042, #2758, #13101, #52276, #18637, #14197, #41201, #63709, #24553, #41916, #47099, #13833, #4957, #48193, #3502, #37470, #70716, #16025, #61097, #37096, #4596, #59990, #15292, #9760, #26763, #38573, #71459, #10495, #65912, #37831, #43751, #9400, #55561, #60351, #32662, #33023, #32294, #14930, #60720, #65543, #20091, #66276, #15654, #54829, #38193, #55203, #4236, #42648, #10130, #14563, #26021, #31930, #59621, #49295, #48560, #27126, #54467, #71828, #48930, #49660, #3865, #43388, #26388, #21199, #65172, #72188, #21567, #44121, #66648, #20835, #9035, #31565, #54104, #71086, #20460, #43014, #40031, #72916, #39671, #22656, #22298, #6038, #34104, #21936, #67739, #56643, #11223, #28572, #51109, #68105, #50747, #506, #44492, #44850, #40382, #61818, #45206, #5682, #72549, #10852, #11587, #16748, #23016, #17471, #39305, #150, #67386, #27860, #45574, #33747, #62544, #6401, #28933, #50024, #11941, #17112, #67025, #62191, #61458, #68459, #50391, #27490, #34466, #56994, #51469, #56292, #28218, #16385, #38940, #12296, #872, #23379, #45927, #34831, #17821, #33386, #62901, #55922, #57357, #5318, #29652, #7848, #2671, #69549, #25188, #1959, #69190, #46284, #36288, #13370, #35912, #69904, #13015, #52553, #63625, #36646, #30741, #47731, #70270, #18908, #58437, #52913, #18182, #19642, #53273, #23736, #41824, #18550, #24466, #42198, #58072, #41469, #19270 ),
 ( #63988, #1592, #8212, #1230, #68825, #64722, #64356, #52190, #7482, #13747, #47373, #6763, #2311, #14106, #58802, #47014, #30010, #29297, #35553, #30384, #24826, #51827, #40751, #63266, #12658, #35193, #57718, #7123, #24102, #41115, #46650, #65823, #21114, #15205, #60631, #37011, #25936, #54744, #54020, #3036, #37743, #66555, #26302, #20745, #20006, #9312, #10043, #60263, #15567, #9677, #31846, #3777, #8576, #53644, #42927, #44033, #59168, #43667, #14477, #4146, #48476, #43303, #31104, #65451, #38110, #54382, #48839, #59534, #15935, #8946, #25567, #71744, #26678, #65086, #71370, #71000, #31478, #32210, #72096, #49210, #66189, #59907, #32577, #3416, #55115, #20376, #4514, #21480, #27043, #49574, #48108, #70631, #14843, #42559, #37384, #51020, #45840, #50309, #61731, #416, #10769, #50662, #33659, #33302, #17021, #45120, #32939, #5597, #67655, #22214, #39580, #62103, #5950, #11132, #11497, #55477, #55840, #51381, #72831, #56204, #16661, #10407, #21845, #22572, #27769, #34019, #28483, #44768, #28134, #5227, #38857, #56556, #67303, #22925, #17387, #39945, #61008, #45483, #66, #4869, #68015, #72460, #6313, #61372, #38484, #62458, #11856, #34375, #39219, #56908, #27405, #49935, #23292, #28842, #783, #44408, #68377, #66934, #16303, #57632, #18466, #64267, #19186, #47647, #17738, #46199, #7038, #40297, #58716, #30655, #6681, #47286, #29567, #57988, #52466, #69465, #8128, #41029, #53187, #35466, #7398, #13288, #52104, #25103, #29926, #2229, #2584, #1873, #1509, #30295, #35108, #62819, #35825, #58348, #24379, #7759, #24742, #46927, #12211, #52827, #57269, #68740, #24013, #29209, #18823, #18098, #69820, #46562, #41386, #41739, #23655, #63545, #69104, #40659, #63898 ) ),
 .UNSPECIFIED., .F., .F., .T. ) 
 B_SPLINE_SURFACE_WITH_KNOTS ( ( 2, 2 ),
 ( 3, 2, 2, 2, 2, 2, 2, 2, 2, 2, 2, 2, 2, 2, 2, 2, 2, 2, 2, 2, 2, 2, 2, 2, 2, 2, 2, 2, 2, 2, 2, 2, 2, 2, 2, 2, 2, 2, 2, 2, 2, 2, 2, 2, 2, 2, 2, 2, 2, 2, 2, 2, 2, 2, 2, 2, 2, 2, 2, 2, 2, 2, 2, 2, 2, 2, 2, 2, 2, 2, 2, 2, 2, 2, 2, 2, 2, 2, 2, 2, 2, 2, 2, 2, 2, 2, 2, 2, 2, 2, 2, 2, 2, 2, 2, 2, 2, 2, 2, 2, 2, 2, 2, 2, 2, 2, 2, 3 ),
 ( 0.000000000000000000, 1.000000000000000000 ),
 ( 0.000000000000000000, 0.009259259259259258745, 0.01851851851851851749, 0.02777777777777777624, 0.03703703703703703498, 0.04629629629629629373, 0.05555555555555555247, 0.06481481481481481122, 0.07407407407407406996, 0.08333333333333332871, 0.09259259259259258745, 0.1018518518518518462, 0.1111111111111111049, 0.1203703703703703637, 0.1296296296296296224, 0.1388888888888888951, 0.1481481481481481399, 0.1574074074074074125, 0.1666666666666666574, 0.1759259259259259300, 0.1851851851851851749, 0.1944444444444444475, 0.2037037037037036924, 0.2129629629629629650, 0.2222222222222222099, 0.2314814814814814825, 0.2407407407407407274, 0.2500000000000000000, 0.2592592592592592449, 0.2685185185185185452, 0.2777777777777777901, 0.2870370370370370350, 0.2962962962962962798, 0.3055555555555555802, 0.3148148148148148251, 0.3240740740740740700, 0.3333333333333333148, 0.3425925925925926152, 0.3518518518518518601, 0.3611111111111111049, 0.3703703703703703498, 0.3796296296296296502, 0.3888888888888888951, 0.3981481481481481399, 0.4074074074074073848, 0.4166666666666666852, 0.4259259259259259300, 0.4351851851851851749, 0.4444444444444444198, 0.4537037037037037202, 0.4629629629629629650, 0.4722222222222222099, 0.4814814814814814548, 0.4907407407407407551, 0.5000000000000000000, 0.5092592592592593004, 0.5185185185185184897, 0.5277777777777777901, 0.5370370370370370905, 0.5462962962962962798, 0.5555555555555555802, 0.5648148148148147696, 0.5740740740740740700, 0.5833333333333333703, 0.5925925925925925597, 0.6018518518518518601, 0.6111111111111111605, 0.6203703703703703498, 0.6296296296296296502, 0.6388888888888888395, 0.6481481481481481399, 0.6574074074074074403, 0.6666666666666666297, 0.6759259259259259300, 0.6851851851851852304, 0.6944444444444444198, 0.7037037037037037202, 0.7129629629629629095, 0.7222222222222222099, 0.7314814814814815103, 0.7407407407407406996, 0.7500000000000000000, 0.7592592592592593004, 0.7685185185185184897, 0.7777777777777777901, 0.7870370370370370905, 0.7962962962962962798, 0.8055555555555555802, 0.8148148148148147696, 0.8240740740740740700, 0.8333333333333333703, 0.8425925925925925597, 0.8518518518518518601, 0.8611111111111111605, 0.8703703703703703498, 0.8796296296296296502, 0.8888888888888888395, 0.8981481481481481399, 0.9074074074074074403, 0.9166666666666666297, 0.9259259259259259300, 0.9351851851851852304, 0.9444444444444444198, 0.9537037037037037202, 0.9629629629629629095, 0.9722222222222222099, 0.9814814814814815103, 0.9876227255986288478 ),
 .UNSPECIFIED. ) 
 GEOMETRIC_REPRESENTATION_ITEM ( )  RATIONAL_B_SPLINE_SURFACE ( (
 ( 1.000000000000000000, 0.8660254037844387076, 1.000000000000000000, 0.8660254037844387076, 1.000000000000000000, 0.8660254037844387076, 1.000000000000000000, 0.8660254037844387076, 1.000000000000000000, 0.8660254037844387076, 1.000000000000000000, 0.8660254037844387076, 1.000000000000000000, 0.8660254037844387076, 1.000000000000000000, 0.8660254037844387076, 1.000000000000000000, 0.8660254037844387076, 1.000000000000000000, 0.8660254037844387076, 1.000000000000000000, 0.8660254037844387076, 1.000000000000000000, 0.8660254037844387076, 1.000000000000000000, 0.8660254037844387076, 1.000000000000000000, 0.8660254037844387076, 1.000000000000000000, 0.8660254037844387076, 1.000000000000000000, 0.8660254037844387076, 1.000000000000000000, 0.8660254037844387076, 1.000000000000000000, 0.8660254037844387076, 1.000000000000000000, 0.8660254037844387076, 1.000000000000000000, 0.8660254037844387076, 1.000000000000000000, 0.8660254037844387076, 1.000000000000000000, 0.8660254037844387076, 1.000000000000000000, 0.8660254037844387076, 1.000000000000000000, 0.8660254037844387076, 1.000000000000000000, 0.8660254037844387076, 1.000000000000000000, 0.8660254037844387076, 1.000000000000000000, 0.8660254037844387076, 1.000000000000000000, 0.8660254037844387076, 1.000000000000000000, 0.8660254037844387076, 1.000000000000000000, 0.8660254037844387076, 1.000000000000000000, 0.8660254037844387076, 1.000000000000000000, 0.8660254037844387076, 1.000000000000000000, 0.8660254037844387076, 1.000000000000000000, 0.8660254037844387076, 1.000000000000000000, 0.8660254037844387076, 1.000000000000000000, 0.8660254037844387076, 1.000000000000000000, 0.8660254037844387076, 1.000000000000000000, 0.8660254037844387076, 1.000000000000000000, 0.8660254037844387076, 1.000000000000000000, 0.8660254037844387076, 1.000000000000000000, 0.8660254037844387076, 1.000000000000000000, 0.8660254037844387076, 1.000000000000000000, 0.8660254037844387076, 1.000000000000000000, 0.8660254037844387076, 1.000000000000000000, 0.8660254037844387076, 1.000000000000000000, 0.8660254037844387076, 1.000000000000000000, 0.8660254037844387076, 1.000000000000000000, 0.8660254037844387076, 1.000000000000000000, 0.8660254037844387076, 1.000000000000000000, 0.8660254037844387076, 1.000000000000000000, 0.8660254037844387076, 1.000000000000000000, 0.8660254037844387076, 1.000000000000000000, 0.8660254037844387076, 1.000000000000000000, 0.8660254037844387076, 1.000000000000000000, 0.8660254037844387076, 1.000000000000000000, 0.8660254037844387076, 1.000000000000000000, 0.8660254037844387076, 1.000000000000000000, 0.8660254037844387076, 1.000000000000000000, 0.8660254037844387076, 1.000000000000000000, 0.8660254037844387076, 1.000000000000000000, 0.8660254037844387076, 1.000000000000000000, 0.8660254037844387076, 1.000000000000000000, 0.8660254037844387076, 1.000000000000000000, 0.8660254037844387076, 1.000000000000000000, 0.8660254037844387076, 1.000000000000000000, 0.8660254037844387076, 1.000000000000000000, 0.8660254037844387076, 1.000000000000000000, 0.8660254037844387076, 1.000000000000000000, 0.8660254037844387076, 1.000000000000000000, 0.8660254037844387076, 1.000000000000000000, 0.8660254037844387076, 1.000000000000000000, 0.8660254037844387076, 1.000000000000000000, 0.8660254037844387076, 1.000000000000000000, 0.8660254037844387076, 1.000000000000000000, 0.8660254037844387076, 1.000000000000000000, 0.8660254037844387076, 1.000000000000000000, 0.8660254037844387076, 1.000000000000000000, 0.8660254037844387076, 1.000000000000000000, 0.8660254037844387076, 1.000000000000000000, 0.8660254037844387076, 1.000000000000000000, 0.8660254037844387076, 1.000000000000000000, 0.8660254037844387076, 1.000000000000000000, 0.8660254037844387076, 1.000000000000000000, 0.8660254037844387076, 1.000000000000000000, 0.8660254037844387076, 1.000000000000000000, 0.8660254037844387076, 1.000000000000000000, 0.8660254037844387076, 1.000000000000000000, 0.8660254037844387076, 1.000000000000000000, 0.8660254037844387076, 1.000000000000000000, 0.8660254037844387076, 1.000000000000000000, 0.8660254037844387076, 1.000000000000000000, 0.8660254037844387076, 1.000000000000000000, 0.8660254037844387076, 1.000000000000000000, 0.8660254037844387076, 1.000000000000000000, 0.8660254037844387076, 1.000000000000000000, 0.8660254037844387076, 1.000000000000000000, 0.8660254037844387076, 1.000000000000000000, 0.8660254037844387076, 1.000000000000000000, 0.8660254037844387076, 1.000000000000000000, 0.8660254037844387076, 1.000000000000000000, 0.8660254037844387076, 1.000000000000000000, 0.8660254037844387076, 1.000000000000000000, 0.8660254037844387076, 1.000000000000000000, 0.8660254037844387076, 1.000000000000000000, 0.8660254037844387076, 1.000000000000000000, 0.8660254037844387076, 1.000000000000000000, 0.9111407643075507545, 0.9401540804404022733),
 ( 1.000000000000000000, 0.8660254037844387076, 1.000000000000000000, 0.8660254037844387076, 1.000000000000000000, 0.8660254037844387076, 1.000000000000000000, 0.8660254037844387076, 1.000000000000000000, 0.8660254037844387076, 1.000000000000000000, 0.8660254037844387076, 1.000000000000000000, 0.8660254037844387076, 1.000000000000000000, 0.8660254037844387076, 1.000000000000000000, 0.8660254037844387076, 1.000000000000000000, 0.8660254037844387076, 1.000000000000000000, 0.8660254037844387076, 1.000000000000000000, 0.8660254037844387076, 1.000000000000000000, 0.8660254037844387076, 1.000000000000000000, 0.8660254037844387076, 1.000000000000000000, 0.8660254037844387076, 1.000000000000000000, 0.8660254037844387076, 1.000000000000000000, 0.8660254037844387076, 1.000000000000000000, 0.8660254037844387076, 1.000000000000000000, 0.8660254037844387076, 1.000000000000000000, 0.8660254037844387076, 1.000000000000000000, 0.8660254037844387076, 1.000000000000000000, 0.8660254037844387076, 1.000000000000000000, 0.8660254037844387076, 1.000000000000000000, 0.8660254037844387076, 1.000000000000000000, 0.8660254037844387076, 1.000000000000000000, 0.8660254037844387076, 1.000000000000000000, 0.8660254037844387076, 1.000000000000000000, 0.8660254037844387076, 1.000000000000000000, 0.8660254037844387076, 1.000000000000000000, 0.8660254037844387076, 1.000000000000000000, 0.8660254037844387076, 1.000000000000000000, 0.8660254037844387076, 1.000000000000000000, 0.8660254037844387076, 1.000000000000000000, 0.8660254037844387076, 1.000000000000000000, 0.8660254037844387076, 1.000000000000000000, 0.8660254037844387076, 1.000000000000000000, 0.8660254037844387076, 1.000000000000000000, 0.8660254037844387076, 1.000000000000000000, 0.8660254037844387076, 1.000000000000000000, 0.8660254037844387076, 1.000000000000000000, 0.8660254037844387076, 1.000000000000000000, 0.8660254037844387076, 1.000000000000000000, 0.8660254037844387076, 1.000000000000000000, 0.8660254037844387076, 1.000000000000000000, 0.8660254037844387076, 1.000000000000000000, 0.8660254037844387076, 1.000000000000000000, 0.8660254037844387076, 1.000000000000000000, 0.8660254037844387076, 1.000000000000000000, 0.8660254037844387076, 1.000000000000000000, 0.8660254037844387076, 1.000000000000000000, 0.8660254037844387076, 1.000000000000000000, 0.8660254037844387076, 1.000000000000000000, 0.8660254037844387076, 1.000000000000000000, 0.8660254037844387076, 1.000000000000000000, 0.8660254037844387076, 1.000000000000000000, 0.8660254037844387076, 1.000000000000000000, 0.8660254037844387076, 1.000000000000000000, 0.8660254037844387076, 1.000000000000000000, 0.8660254037844387076, 1.000000000000000000, 0.8660254037844387076, 1.000000000000000000, 0.8660254037844387076, 1.000000000000000000, 0.8660254037844387076, 1.000000000000000000, 0.8660254037844387076, 1.000000000000000000, 0.8660254037844387076, 1.000000000000000000, 0.8660254037844387076, 1.000000000000000000, 0.8660254037844387076, 1.000000000000000000, 0.8660254037844387076, 1.000000000000000000, 0.8660254037844387076, 1.000000000000000000, 0.8660254037844387076, 1.000000000000000000, 0.8660254037844387076, 1.000000000000000000, 0.8660254037844387076, 1.000000000000000000, 0.8660254037844387076, 1.000000000000000000, 0.8660254037844387076, 1.000000000000000000, 0.8660254037844387076, 1.000000000000000000, 0.8660254037844387076, 1.000000000000000000, 0.8660254037844387076, 1.000000000000000000, 0.8660254037844387076, 1.000000000000000000, 0.8660254037844387076, 1.000000000000000000, 0.8660254037844387076, 1.000000000000000000, 0.8660254037844387076, 1.000000000000000000, 0.8660254037844387076, 1.000000000000000000, 0.8660254037844387076, 1.000000000000000000, 0.8660254037844387076, 1.000000000000000000, 0.8660254037844387076, 1.000000000000000000, 0.8660254037844387076, 1.000000000000000000, 0.8660254037844387076, 1.000000000000000000, 0.8660254037844387076, 1.000000000000000000, 0.8660254037844387076, 1.000000000000000000, 0.8660254037844387076, 1.000000000000000000, 0.8660254037844387076, 1.000000000000000000, 0.8660254037844387076, 1.000000000000000000, 0.8660254037844387076, 1.000000000000000000, 0.8660254037844387076, 1.000000000000000000, 0.8660254037844387076, 1.000000000000000000, 0.8660254037844387076, 1.000000000000000000, 0.8660254037844387076, 1.000000000000000000, 0.8660254037844387076, 1.000000000000000000, 0.8660254037844387076, 1.000000000000000000, 0.8660254037844387076, 1.000000000000000000, 0.8660254037844387076, 1.000000000000000000, 0.8660254037844387076, 1.000000000000000000, 0.8660254037844387076, 1.000000000000000000, 0.8660254037844387076, 1.000000000000000000, 0.8660254037844387076, 1.000000000000000000, 0.8660254037844387076, 1.000000000000000000, 0.8660254037844387076, 1.000000000000000000, 0.9111407643075507545, 0.9401540804404022733) ) ) 
 REPRESENTATION_ITEM ( '' )  SURFACE ( )  );
#55782 = CARTESIAN_POINT ( 'NONE',  ( 28.91250000122903074, -4.330127018922190985, -2.500000000000001332 ) ) ;
#55783 = CARTESIAN_POINT ( 'NONE',  ( 20.48437500061451644, -2.746126346562642428, -4.756430356249999214 ) ) ;
#55784 = CARTESIAN_POINT ( 'NONE',  ( 25.22812500061451502, 4.541064518000418104, 2.621784821874999949 ) ) ;
#55785 = CARTESIAN_POINT ( 'NONE',  ( 16.34062500061451573, -3.027376345333614438, 5.243569643749998122 ) ) ;
#55786 = CARTESIAN_POINT ( 'NONE',  ( 13.36875000122903145, 2.886751345948126879, 4.999999999999999112 ) ) ;
#55787 = CARTESIAN_POINT ( 'NONE',  ( 13.88437500061451679, 6.421520780324663323E-16, -5.243569643749999010 ) ) ;
#55788 = CARTESIAN_POINT ( 'NONE',  ( 26.21250000122903501, -4.330127018922190985, -2.500000000000001332 ) ) ;
#55789 = CARTESIAN_POINT ( 'NONE',  ( 25.50000000122903288, 5.773502691896255534, 3.535250795749688894E-16 ) ) ;
#55790 = CARTESIAN_POINT ( 'NONE',  ( 4.359375000614517326, -4.541064518000417216, -2.621784821875001281 ) ) ;
#55791 = CARTESIAN_POINT ( 'NONE',  ( 13.20937500061451786, 0.000000000000000000, 5.243569643749999010 ) ) ;
#55792 = CARTESIAN_POINT ( 'NONE',  ( -3.999999999999999112, 11.86249999999999893, 27.69059892324149885 ) ) ;
#55793 = CARTESIAN_POINT ( 'NONE',  ( 29.85937500061451644, 0.000000000000000000, 5.243569643749999010 ) ) ;
#55794 = DIRECTION ( 'NONE',  ( -1.000000000000000000, -0.000000000000000000, -0.000000000000000000 ) ) ;
#55795 = CARTESIAN_POINT ( 'NONE',  ( 24.94687500061451502, -3.027376345333614438, 5.243569643749998122 ) ) ;
#55796 = CARTESIAN_POINT ( 'NONE',  ( 17.44687500061451857, -3.027376345333610441, -5.243569643749999898 ) ) ;
#55797 = CARTESIAN_POINT ( 'NONE',  ( -7.967954043666661671E-16, 15.79062499938548392, 34.33755215474603517 ) ) ;
#55798 = CARTESIAN_POINT ( 'NONE',  ( 28.98750000000000071, 5.773502691896255534, 3.535250795749688894E-16 ) ) ;
#55799 = CARTESIAN_POINT ( 'NONE',  ( 3.450000001229036162, 5.773502691896255534, 3.535250795749688894E-16 ) ) ;
#55800 = CARTESIAN_POINT ( 'NONE',  ( 4.462500000000001243, -5.773502691896255534, -1.060575238724906372E-15 ) ) ;
#55801 = CARTESIAN_POINT ( 'NONE',  ( 29.78437500061451715, 4.119189519843966529, 2.378215178124999607 ) ) ;
#55802 = CARTESIAN_POINT ( 'NONE',  ( 18.66562500061451146, -6.054752690667223547, -1.112240025338166033E-15 ) ) ;
#55803 = CARTESIAN_POINT ( 'NONE',  ( 8.550000000000002487, -4.330127018922190985, -2.500000000000001332 ) ) ;
#55804 = CARTESIAN_POINT ( 'NONE',  ( 15.41250000000000142, 2.886751345948129099, -4.999999999999997335 ) ) ;
#55805 = CARTESIAN_POINT ( 'NONE',  ( 17.51249999999999929, -5.773502691896255534, -1.060575238724906372E-15 ) ) ;
#55806 = CARTESIAN_POINT ( 'NONE',  ( 25.05000000000000071, 0.000000000000000000, 4.999999999999998224 ) ) ;
#55807 = CARTESIAN_POINT ( 'NONE',  ( 19.98750000122903359, 6.123233995736764310E-16, -4.999999999999998224 ) ) ;
#55808 = CARTESIAN_POINT ( 'NONE',  ( 5.603843221884249104, 8.282830004121999323, 32.15295242426309130 ) ) ;
#55809 =( BOUNDED_CURVE ( )  B_SPLINE_CURVE ( 2, ( #239, #61913, #61546, #62282, #23107, #38669, #17560, #27584, #16117 ),
 .UNSPECIFIED., .F., .F. ) 
 B_SPLINE_CURVE_WITH_KNOTS ( ( 3, 2, 2, 2, 3 ),
 ( 0.6195652173913043237, 0.6231884057971014412, 0.6304347826086956763, 0.6376811594202898004, 0.6413043478260869179 ),
 .UNSPECIFIED. ) 
 CURVE ( )  GEOMETRIC_REPRESENTATION_ITEM ( )  RATIONAL_B_SPLINE_CURVE ( ( 0.9330127018922194093, 0.9330127018922194093, 1.000000000000000000, 0.8660254037844387076, 1.000000000000000000, 0.8660254037844387076, 1.000000000000000000, 0.9330127018922194093, 0.9330127018922194093 ) ) 
 REPRESENTATION_ITEM ( '' )  );
#55810 = CARTESIAN_POINT ( 'NONE',  ( 28.05937500061451573, 0.000000000000000000, 5.243569643749999010 ) ) ;
#55811 = ORIENTED_EDGE ( 'NONE', *, *, #44062, .F. ) ;
#55812 = CARTESIAN_POINT ( 'NONE',  ( 16.86562500061451786, -6.054752690667223547, -1.112240025338166033E-15 ) ) ;
#55813 = CARTESIAN_POINT ( 'NONE',  ( 23.65312500061451573, -4.541064518000417216, -2.621784821875001281 ) ) ;
#55814 = CARTESIAN_POINT ( 'NONE',  ( 23.10937500061451644, 0.000000000000000000, 5.243569643749999010 ) ) ;
#55815 = CARTESIAN_POINT ( 'NONE',  ( 5.587500000000003020, 5.773502691896255534, 3.535250795749688894E-16 ) ) ;
#55816 = CARTESIAN_POINT ( 'NONE',  ( 8.728125000614518569, -4.541064518000419881, 2.621784821874995952 ) ) ;
#55817 = CARTESIAN_POINT ( 'NONE',  ( 24.55312500061451786, -4.541064518000417216, -2.621784821875001281 ) ) ;
#55818 = CARTESIAN_POINT ( 'NONE',  ( 15.49687500061451750, -3.027376345333614438, 5.243569643749998122 ) ) ;
#55819 = CARTESIAN_POINT ( 'NONE',  ( 20.07187500061451857, -6.054752690667223547, -1.112240025338166033E-15 ) ) ;
#55820 = CARTESIAN_POINT ( 'NONE',  ( 2.121784821874999061, 10.25937500061451857, 26.32496088578401583 ) ) ;
#55821 = CARTESIAN_POINT ( 'NONE',  ( 21.86250000122903003, 4.330127018922192761, -2.499999999999997780 ) ) ;
#55822 = CARTESIAN_POINT ( 'NONE',  ( 16.35937500061451644, 0.000000000000000000, 4.756430356249998326 ) ) ;
#55823 = CARTESIAN_POINT ( 'NONE',  ( 12.44062500061451537, -3.027376345333610441, -5.243569643749999898 ) ) ;
#55824 = CARTESIAN_POINT ( 'NONE',  ( 7.246875000614518392, 6.054752690667223547, 3.707466751127219781E-16 ) ) ;
#55825 = CARTESIAN_POINT ( 'NONE',  ( 7.434375000614519280, -4.541064518000419881, 2.621784821874995952 ) ) ;
#55826 = EDGE_LOOP ( 'NONE', ( #19445, #12359, #62953, #52101 ) ) ;
#55827 = CARTESIAN_POINT ( 'NONE',  ( 27.27187500061451431, -6.054752690667223547, -1.112240025338166033E-15 ) ) ;
#55828 = CARTESIAN_POINT ( 'NONE',  ( 19.64062500061451644, -3.027376345333610441, -5.243569643749999898 ) ) ;
#55829 = CARTESIAN_POINT ( 'NONE',  ( 28.98750000122903359, 6.123233995736764310E-16, -4.999999999999998224 ) ) ;
#55830 = EDGE_CURVE ( 'NONE', #30395, #33359, #48396, .T. ) ;
#55831 = CARTESIAN_POINT ( 'NONE',  ( 28.56562500061451715, -6.054752690667223547, -1.112240025338166033E-15 ) ) ;
#55832 = CARTESIAN_POINT ( 'NONE',  ( 24.27187500061452141, 3.027376345333613106, -5.243569643749998122 ) ) ;
#55833 = CARTESIAN_POINT ( 'NONE',  ( 18.62812500061451715, -4.541064518000419881, 2.621784821874995952 ) ) ;
#55834 = CARTESIAN_POINT ( 'NONE',  ( -3.999999999999997335, 10.13750000000000284, 32.30940107675850470 ) ) ;
#55835 = CARTESIAN_POINT ( 'NONE',  ( 24.81562500061451715, 3.027376345333611329, 5.243569643749999010 ) ) ;
#55836 = CARTESIAN_POINT ( 'NONE',  ( 5.512500001229033941, -4.330127018922190985, -2.500000000000001332 ) ) ;
#55837 = ORIENTED_EDGE ( 'NONE', *, *, #58697, .T. ) ;
#55838 = CARTESIAN_POINT ( 'NONE',  ( 28.23750000000000426, -2.886751345948129988, 4.999999999999997335 ) ) ;
#55839 = CARTESIAN_POINT ( 'NONE',  ( -1.999999999999997113, 16.02500000000000213, -26.53589838486224295 ) ) ;
#55840 = CARTESIAN_POINT ( 'NONE',  ( -1.878215178125001827, 17.10312499938548214, 33.25316411605952283 ) ) ;
#55841 = CARTESIAN_POINT ( 'NONE',  ( 5.146875000614517859, -3.027376345333614438, 5.243569643749998122 ) ) ;
#55842 = CARTESIAN_POINT ( 'NONE',  ( 12.81562500061451537, -6.054752690667223547, -1.112240025338166033E-15 ) ) ;
#55843 = CARTESIAN_POINT ( 'NONE',  ( 6.309375000614517504, 4.541064518000418104, -2.621784821874998173 ) ) ;
#55844 = CARTESIAN_POINT ( 'NONE',  ( 23.77500000122903145, 2.886751345948126879, 4.999999999999999112 ) ) ;
#55845 = CARTESIAN_POINT ( 'NONE',  ( 13.95937500061451786, 4.541064518000418104, -2.621784821874998173 ) ) ;
#55846 = CARTESIAN_POINT ( 'NONE',  ( 3.046875000614519990, -3.027376345333610441, -5.243569643749999898 ) ) ;
#55847 = CARTESIAN_POINT ( 'NONE',  ( 28.12499999999999645, 4.330127018922191873, 2.499999999999999556 ) ) ;
#55848 = CARTESIAN_POINT ( 'NONE',  ( 25.62187500061451573, 3.027376345333613106, -5.243569643749998122 ) ) ;
#55849 = CARTESIAN_POINT ( 'NONE',  ( 3.478125000614517237, 6.421520780324663323E-16, -5.243569643749999010 ) ) ;
#55850 = CARTESIAN_POINT ( 'NONE',  ( 12.21562500061451573, 3.027376345333611329, 5.243569643749999010 ) ) ;
#55851 = VERTEX_POINT ( 'NONE', #21601 ) ;
#55852 = CARTESIAN_POINT ( 'NONE',  ( 9.853125000614516793, 4.541064518000418104, -2.621784821874998173 ) ) ;
#55853 = CARTESIAN_POINT ( 'NONE',  ( 7.228125000614517681, 4.541064518000418104, 2.621784821874999949 ) ) ;
#55854 = CARTESIAN_POINT ( 'NONE',  ( 18.94687500061451502, 5.492252693125287522, 3.363034840372157021E-16 ) ) ;
#55855 = ADVANCED_FACE ( 'NONE', ( #27522 ), #43785, .T. ) ;
#55856 = CARTESIAN_POINT ( 'NONE',  ( 45.00000000000000000, 0.000000000000000000, 0.000000000000000000 ) ) ;
#55857 = CARTESIAN_POINT ( 'NONE',  ( 15.56250000000000000, 2.886751345948126879, 4.999999999999999112 ) ) ;
#55858 = CARTESIAN_POINT ( 'NONE',  ( 16.47187500061452070, -6.054752690667223547, -1.112240025338166033E-15 ) ) ;
#55859 = CARTESIAN_POINT ( 'NONE',  ( 12.78750000122903430, 6.123233995736764310E-16, -4.999999999999998224 ) ) ;
#55860 = CARTESIAN_POINT ( 'NONE',  ( 20.54999999999999716, 0.000000000000000000, 4.999999999999998224 ) ) ;
#55861 = CARTESIAN_POINT ( 'NONE',  ( 20.07187500061451857, -6.054752690667223547, -1.112240025338166033E-15 ) ) ;
#55862 = CARTESIAN_POINT ( 'NONE',  ( 2.121784821875001281, 13.20312500061451821, -26.32496088578401938 ) ) ;
#55863 = CARTESIAN_POINT ( 'NONE',  ( 21.89999999999999858, 0.000000000000000000, 4.999999999999998224 ) ) ;
#55864 = CARTESIAN_POINT ( 'NONE',  ( 25.17187500061451644, 4.119189519843966529, 2.378215178124999607 ) ) ;
#55865 = CARTESIAN_POINT ( 'NONE',  ( 14.49375000122903145, -2.886751345948126435, -5.000000000000000000 ) ) ;
#55866 = CARTESIAN_POINT ( 'NONE',  ( 28.00312500061451715, 0.000000000000000000, 5.243569643749999010 ) ) ;
#55867 = EDGE_CURVE ( 'NONE', #54755, #55534, #55944, .T. ) ;
#55868 = PLANE ( 'NONE',  #31588 ) ;
#55869 = DIRECTION ( 'NONE',  ( 0.000000000000000000, 0.000000000000000000, 1.000000000000000000 ) ) ;
#55870 = CARTESIAN_POINT ( 'NONE',  ( 26.25000000000000000, 4.330127018922192761, -2.499999999999997780 ) ) ;
#55871 = CARTESIAN_POINT ( 'NONE',  ( 8.653125000614515727, 0.000000000000000000, 5.243569643749999010 ) ) ;
#55872 = CARTESIAN_POINT ( 'NONE',  ( 26.55937500061451217, 2.746126346562643317, 4.756430356249998326 ) ) ;
#55873 = CARTESIAN_POINT ( 'NONE',  ( 20.93437500061451573, -4.541064518000419881, 2.621784821874995952 ) ) ;
#55874 = CARTESIAN_POINT ( 'NONE',  ( 13.54687500061451466, 0.000000000000000000, 4.756430356249998326 ) ) ;
#55875 = CARTESIAN_POINT ( 'NONE',  ( 4.378125000614518925, 6.421520780324663323E-16, -5.243569643749999010 ) ) ;
#55876 = CARTESIAN_POINT ( 'NONE',  ( 11.89687500061451608, -3.027376345333614438, 5.243569643749998122 ) ) ;
#55877 = ORIENTED_EDGE ( 'NONE', *, *, #13034, .T. ) ;
#55878 = CARTESIAN_POINT ( 'NONE',  ( 20.78437500061451715, 4.541064518000418104, 2.621784821874999949 ) ) ;
#55879 = CARTESIAN_POINT ( 'NONE',  ( 3.992981257374419890, 3.009426956198102854, -29.72584546141768769 ) ) ;
#55880 = CARTESIAN_POINT ( 'NONE',  ( 28.53749999999999787, 5.773502691896255534, 3.535250795749688894E-16 ) ) ;
#55881 = CARTESIAN_POINT ( 'NONE',  ( 6.187500000000002665, -2.886751345948129988, 4.999999999999997335 ) ) ;
#55882 = CARTESIAN_POINT ( 'NONE',  ( 13.80000000122903181, 5.773502691896255534, 3.535250795749688894E-16 ) ) ;
#55883 = CARTESIAN_POINT ( 'NONE',  ( -1.487416814333745711E-14, 15.16250000000000142, -26.00000000000000000 ) ) ;
#55884 = DIRECTION ( 'NONE',  ( -0.000000000000000000, -1.000000000000000000, -0.000000000000000000 ) ) ;
#55885 = VERTEX_POINT ( 'NONE', #39705 ) ;
#55886 = CARTESIAN_POINT ( 'NONE',  ( 12.07499999999999929, -4.330127018922194537, 2.499999999999995559 ) ) ;
#55887 = CARTESIAN_POINT ( 'NONE',  ( 17.10000000000000142, -4.330127018922190985, -2.500000000000001332 ) ) ;
#55888 = CARTESIAN_POINT ( 'NONE',  ( 12.15000000122903501, -2.886751345948129988, 4.999999999999997335 ) ) ;
#55889 = CARTESIAN_POINT ( 'NONE',  ( 12.55312500061451786, 4.541064518000418104, -2.621784821874998173 ) ) ;
#55890 = CARTESIAN_POINT ( 'NONE',  ( 8.812500000000000000, 2.886751345948126879, 4.999999999999999112 ) ) ;
#55891 = CARTESIAN_POINT ( 'NONE',  ( -2.000000000000000000, 15.53750000122903430, 26.53589838486224650 ) ) ;
#55892 = CARTESIAN_POINT ( 'NONE',  ( 4.243569643749999898, 15.13437500061451679, -30.00000000000000000 ) ) ;
#55893 = CARTESIAN_POINT ( 'NONE',  ( 27.26250000122903216, 4.330127018922192761, -2.499999999999997780 ) ) ;
#55894 = CARTESIAN_POINT ( 'NONE',  ( 2.655984681222220721E-16, 14.10312499938548392, 25.66244784525396483 ) ) ;
#55895 = CARTESIAN_POINT ( 'NONE',  ( 8.512499999999999289, -5.773502691896255534, -1.060575238724906372E-15 ) ) ;
#55896 = ORIENTED_EDGE ( 'NONE', *, *, #5848, .F. ) ;
#55897 = CARTESIAN_POINT ( 'NONE',  ( 23.72812500061451502, 6.421520780324663323E-16, -5.243569643749999010 ) ) ;
#55898 = DIRECTION ( 'NONE',  ( 0.000000000000000000, 0.000000000000000000, -1.000000000000000000 ) ) ;
#55899 = CARTESIAN_POINT ( 'NONE',  ( 29.03437500061451715, -4.541064518000419881, 2.621784821874995952 ) ) ;
#55900 = CARTESIAN_POINT ( 'NONE',  ( 20.85937500061451644, 0.000000000000000000, 5.243569643749999010 ) ) ;
#55901 = CARTESIAN_POINT ( 'NONE',  ( 16.07812500061451289, 6.421520780324663323E-16, -5.243569643749999010 ) ) ;
#55902 = CARTESIAN_POINT ( 'NONE',  ( -4.243569643749999898, 11.66562500061459495, -32.45002607614398471 ) ) ;
#55903 = CARTESIAN_POINT ( 'NONE',  ( 6.815625000614517148, 3.027376345333611329, 5.243569643749999010 ) ) ;
#55904 = CARTESIAN_POINT ( 'NONE',  ( 28.98750000122903359, 6.123233995736764310E-16, -4.999999999999998224 ) ) ;
#55905 = CARTESIAN_POINT ( 'NONE',  ( 25.32187500061451857, 2.746126346562643317, 4.756430356249998326 ) ) ;
#55906 = CARTESIAN_POINT ( 'NONE',  ( 19.79062500061451502, 6.054752690667223547, 3.707466751127219781E-16 ) ) ;
#55907 = CARTESIAN_POINT ( 'NONE',  ( 45.00000000000000000, 6.363961030678916053, -6.363961030678939146 ) ) ;
#55908 = CARTESIAN_POINT ( 'NONE',  ( 3.756430356250000546, 19.42812499938548143, 27.83122392262697886 ) ) ;
#55909 = CARTESIAN_POINT ( 'NONE',  ( 15.57187500061451679, -6.054752690667223547, -1.112240025338166033E-15 ) ) ;
#55910 = CARTESIAN_POINT ( 'NONE',  ( 13.95937500061451786, 4.541064518000418104, -2.621784821874998173 ) ) ;
#55911 = CARTESIAN_POINT ( 'NONE',  ( 22.69687500061451857, -3.027376345333614438, 5.243569643749998122 ) ) ;
#55912 = VERTEX_POINT ( 'NONE', #21968 ) ;
#55913 = CARTESIAN_POINT ( 'NONE',  ( 3.215625000614518836, 3.027376345333611329, 5.243569643749999010 ) ) ;
#55914 = CARTESIAN_POINT ( 'NONE',  ( 26.76562500061451644, -6.054752690667223547, -1.112240025338166033E-15 ) ) ;
#55915 = CARTESIAN_POINT ( 'NONE',  ( 26.20312500061451644, 0.000000000000000000, 5.243569643749999010 ) ) ;
#55916 = CARTESIAN_POINT ( 'NONE',  ( 7.668750001229033053, -5.773502691896255534, -1.060575238724906372E-15 ) ) ;
#55917 = CARTESIAN_POINT ( 'NONE',  ( 3.999999999999999112, 17.52499999999999858, 30.00000000000000000 ) ) ;
#55918 = CARTESIAN_POINT ( 'NONE',  ( 5.259375000614518569, -4.541064518000417216, -2.621784821875001281 ) ) ;
#55919 = CARTESIAN_POINT ( 'NONE',  ( 11.10000000122903252, 5.773502691896255534, 3.535250795749688894E-16 ) ) ;
#55920 = CARTESIAN_POINT ( 'NONE',  ( 7.162500001229032520, 0.000000000000000000, 4.999999999999998224 ) ) ;
#55921 = CARTESIAN_POINT ( 'NONE',  ( 2.953125000614516438, -4.541064518000417216, -2.621784821875001281 ) ) ;
#55922 = CARTESIAN_POINT ( 'NONE',  ( 3.999999999999998668, 19.60624999877096997, 32.30940107675850470 ) ) ;
#55923 = CARTESIAN_POINT ( 'NONE',  ( 17.71875000122903288, 2.886751345948129099, -4.999999999999998224 ) ) ;
#55924 = CARTESIAN_POINT ( 'NONE',  ( 11.74687500061451573, 6.054752690667223547, 3.707466751127219781E-16 ) ) ;
#55925 = CARTESIAN_POINT ( 'NONE',  ( 3.999999999999998668, 14.86250000000000071, -32.30940107675850470 ) ) ;
#55926 = VERTEX_POINT ( 'NONE', #11619 ) ;
#55927 = CARTESIAN_POINT ( 'NONE',  ( 19.52812500061451573, -4.541064518000419881, 2.621784821874995952 ) ) ;
#55928 = CARTESIAN_POINT ( 'NONE',  ( 13.13437500061451857, 4.541064518000418104, 2.621784821874999949 ) ) ;
#55929 = CARTESIAN_POINT ( 'NONE',  ( 4.453125000614517326, 4.541064518000418104, -2.621784821874998173 ) ) ;
#55930 = CARTESIAN_POINT ( 'NONE',  ( 22.95937500061451431, 4.541064518000418104, -2.621784821874998173 ) ) ;
#55931 = CARTESIAN_POINT ( 'NONE',  ( 10.99687500061451750, -3.027376345333614438, 5.243569643749998122 ) ) ;
#55932 = CARTESIAN_POINT ( 'NONE',  ( 6.328125000614515550, 4.541064518000418104, 2.621784821874999949 ) ) ;
#55933 = DIRECTION ( 'NONE',  ( 1.000000000000000000, 0.000000000000000000, 0.000000000000000000 ) ) ;
#55935 = ADVANCED_FACE ( 'NONE', ( #38608 ), #71032, .T. ) ;
#55934 = CARTESIAN_POINT ( 'NONE',  ( 6.375000001229031987, -5.773502691896255534, -1.060575238724906372E-15 ) ) ;
#55936 = CARTESIAN_POINT ( 'NONE',  ( 19.07812500061451644, -4.541064518000419881, 2.621784821874995952 ) ) ;
#55937 = CARTESIAN_POINT ( 'NONE',  ( 8.287500001229034297, 6.123233995736764310E-16, -4.999999999999998224 ) ) ;
#55938 = CARTESIAN_POINT ( 'NONE',  ( 16.11562500061451786, 3.027376345333613106, -5.243569643749998122 ) ) ;
#55939 = CARTESIAN_POINT ( 'NONE',  ( 15.06562500061451537, -6.054752690667223547, -1.112240025338166033E-15 ) ) ;
#55940 = CARTESIAN_POINT ( 'NONE',  ( 25.05937500061451573, -4.119189519843965641, -2.378215178125001383 ) ) ;
#55941 = CARTESIAN_POINT ( 'NONE',  ( 16.01249999999999929, 2.886751345948126879, 4.999999999999999112 ) ) ;
#55942 = CARTESIAN_POINT ( 'NONE',  ( 9.712500001229033231, 4.330127018922192761, -2.499999999999997780 ) ) ;
#55943 = CARTESIAN_POINT ( 'NONE',  ( 4.753125000614515372, -4.541064518000417216, -2.621784821875001281 ) ) ;
#55944 =( BOUNDED_CURVE ( )  B_SPLINE_CURVE ( 2, ( #38227, #11259, #28249, #44155, #16059, #45239, #67772 ),
 .UNSPECIFIED., .F., .F. ) 
 B_SPLINE_CURVE_WITH_KNOTS ( ( 3, 2, 2, 3 ),
 ( 0.9428132104952601233, 0.9444444444444444198, 0.9472222222222221877, 0.9486699882857303479 ),
 .UNSPECIFIED. ) 
 CURVE ( )  GEOMETRIC_REPRESENTATION_ITEM ( )  RATIONAL_B_SPLINE_CURVE ( ( 0.9350522116989212762, 0.9213241925169703972, 1.000000000000000000, 0.8660254037844387076, 1.000000000000000000, 0.9301730054416843529, 0.9331330810709438373 ) ) 
 REPRESENTATION_ITEM ( '' )  );
#55945 = CARTESIAN_POINT ( 'NONE',  ( 20.88750000122903572, 6.123233995736764310E-16, -4.999999999999998224 ) ) ;
#55946 = CARTESIAN_POINT ( 'NONE',  ( 27.86249999999999716, -5.773502691896255534, -1.060575238724906372E-15 ) ) ;
#55947 = CARTESIAN_POINT ( 'NONE',  ( 9.001249775931846008E-16, 14.57187500061451679, -25.09994784771203058 ) ) ;
#55948 = CARTESIAN_POINT ( 'NONE',  ( 21.37499999999999645, 4.330127018922191873, 2.499999999999999556 ) ) ;
#55949 = CARTESIAN_POINT ( 'NONE',  ( 3.412500001229032964, 4.330127018922192761, -2.499999999999997780 ) ) ;
#55950 = CARTESIAN_POINT ( 'NONE',  ( 4.209375000614516971, 0.000000000000000000, 5.243569643749999010 ) ) ;
#55951 = CARTESIAN_POINT ( 'NONE',  ( 20.97187500061451715, -6.054752690667223547, -1.112240025338166033E-15 ) ) ;
#55952 = CARTESIAN_POINT ( 'NONE',  ( -1.999999999999997113, 15.12500000000000000, 33.46410161513775705 ) ) ;
#55953 = CARTESIAN_POINT ( 'NONE',  ( 16.97812500061451502, 6.421520780324663323E-16, -5.243569643749999010 ) ) ;
#55954 = CARTESIAN_POINT ( 'NONE',  ( 11.04375000122903216, 5.773502691896255534, 3.535250795749688894E-16 ) ) ;
#55955 = CARTESIAN_POINT ( 'NONE',  ( -3.999999999999999112, 15.50000000000000000, -30.00000000000000000 ) ) ;
#55956 = CARTESIAN_POINT ( 'NONE',  ( -3.999999999999999112, 15.50000000000000000, 30.00000000000000000 ) ) ;
#55957 = CARTESIAN_POINT ( 'NONE',  ( 28.54687500061451644, -3.027376345333614438, 5.243569643749998122 ) ) ;
#55958 = CARTESIAN_POINT ( 'NONE',  ( 19.80937500061451217, 2.746126346562643317, 4.756430356249998326 ) ) ;
#55959 = AXIS2_PLACEMENT_3D ( 'NONE', #40943, #63457, #18012 ) ;
#55960 = CARTESIAN_POINT ( 'NONE',  ( 13.71562500061451750, -6.054752690667223547, -1.112240025338166033E-15 ) ) ;
#55961 = CARTESIAN_POINT ( 'NONE',  ( 11.22187500061451892, 3.027376345333613106, -5.243569643749998122 ) ) ;
#55962 = EDGE_LOOP ( 'NONE', ( #2046, #9501, #54511, #21618 ) ) ;
#55963 = CARTESIAN_POINT ( 'NONE',  ( 29.01562500061451644, -6.054752690667223547, -1.112240025338166033E-15 ) ) ;
#55964 = CARTESIAN_POINT ( 'NONE',  ( 23.24062500061451786, -3.027376345333610441, -5.243569643749999898 ) ) ;
#55965 = CARTESIAN_POINT ( 'NONE',  ( 3.999999999999998668, 15.42500000122903359, -32.30940107675850470 ) ) ;
#55966 = EDGE_CURVE ( 'NONE', #66904, #18961, #26230, .T. ) ;
#55967 = CARTESIAN_POINT ( 'NONE',  ( 11.55000000000000071, 0.000000000000000000, 4.999999999999998224 ) ) ;
#55968 = EDGE_CURVE ( 'NONE', #62113, #36300, #60192, .T. ) ;
#55969 = CARTESIAN_POINT ( 'NONE',  ( 22.83750000122903501, 4.330127018922191873, 2.499999999999999556 ) ) ;
#55970 = CARTESIAN_POINT ( 'NONE',  ( 17.05312500061451786, 4.541064518000418104, -2.621784821874998173 ) ) ;
#55971 = CARTESIAN_POINT ( 'NONE',  ( 11.70937500061451608, 2.746126346562643317, 4.756430356249998326 ) ) ;
#55972 = ORIENTED_EDGE ( 'NONE', *, *, #41790, .T. ) ;
#55973 = CARTESIAN_POINT ( 'NONE',  ( 19.79999999999999716, -4.330127018922190985, -2.500000000000001332 ) ) ;
#55974 = CARTESIAN_POINT ( 'NONE',  ( 22.72499999999999787, 4.330127018922191873, 2.499999999999999556 ) ) ;
#55975 = CARTESIAN_POINT ( 'NONE',  ( 20.89687500061452141, -3.027376345333614438, 5.243569643749998122 ) ) ;
#55976 = CARTESIAN_POINT ( 'NONE',  ( 26.57812500061451644, 4.541064518000418104, 2.621784821874999949 ) ) ;
#55977 = EDGE_LOOP ( 'NONE', ( #32331, #49561, #54877, #34882 ) ) ;
#55978 = FACE_OUTER_BOUND ( 'NONE', #49846, .T. ) ;
#55979 = CARTESIAN_POINT ( 'NONE',  ( 8.540625000614518569, 6.054752690667223547, 3.707466751127219781E-16 ) ) ;
#55980 = LINE ( 'NONE', #5374, #43005 ) ;
#55981 = CARTESIAN_POINT ( 'NONE',  ( 17.06250000000000000, -5.773502691896255534, -1.060575238724906372E-15 ) ) ;
#55982 = CARTESIAN_POINT ( 'NONE',  ( 24.14999999999999858, 0.000000000000000000, 4.999999999999998224 ) ) ;
#55983 = CARTESIAN_POINT ( 'NONE',  ( 7.724999999999999645, 6.123233995736764310E-16, -4.999999999999998224 ) ) ;
#55984 = CARTESIAN_POINT ( 'NONE',  ( 5.521875000614517859, 3.027376345333611329, 5.243569643749999010 ) ) ;
#55985 = CARTESIAN_POINT ( 'NONE',  ( 29.25937500061451502, 4.541064518000418104, -2.621784821874998173 ) ) ;
#55986 = VERTEX_POINT ( 'NONE', #49137 ) ;
#55987 = CARTESIAN_POINT ( 'NONE',  ( 25.00312500061451715, -4.541064518000417216, -2.621784821875001281 ) ) ;
#55988 = CARTESIAN_POINT ( 'NONE',  ( 24.27187500061452141, 3.027376345333613106, -5.243569643749998122 ) ) ;
#55989 = CARTESIAN_POINT ( 'NONE',  ( -4.243569643749998122, 18.94062500061459531, -27.54997392385601174 ) ) ;
#55990 = CARTESIAN_POINT ( 'NONE',  ( 13.08750000000000036, -2.886751345948125991, -5.000000000000000000 ) ) ;
#55991 = CARTESIAN_POINT ( 'NONE',  ( 9.553125000614517859, 0.000000000000000000, 5.243569643749999010 ) ) ;
#55992 = CARTESIAN_POINT ( 'NONE',  ( 1.626862140677534273E-15, 13.47500000122903252, -26.00000000000000355 ) ) ;
#55993 = CARTESIAN_POINT ( 'NONE',  ( -1.243387493232115393E-14, 16.60624999877096641, 26.00000000000000000 ) ) ;
#55994 = CARTESIAN_POINT ( 'NONE',  ( 25.22812500061451502, 4.541064518000418104, 2.621784821874999949 ) ) ;
#55995 = CARTESIAN_POINT ( 'NONE',  ( 8.531250001229034652, -4.330127018922194537, 2.499999999999995559 ) ) ;
#55996 = CARTESIAN_POINT ( 'NONE',  ( 15.42187500061451821, 2.746126346562643317, 4.756430356249998326 ) ) ;
#55997 = CARTESIAN_POINT ( 'NONE',  ( 3.628125000614518036, 4.541064518000418104, 2.621784821874999949 ) ) ;
#55998 = CARTESIAN_POINT ( 'NONE',  ( 19.92187500061451644, 3.027376345333611329, 5.243569643749999010 ) ) ;
#55999 = CARTESIAN_POINT ( 'NONE',  ( -4.243569643749999898, 14.87187500061451928, 27.54997392385601529 ) ) ;
#56000 = CARTESIAN_POINT ( 'NONE',  ( 21.75937500061451502, 0.000000000000000000, 5.243569643749999010 ) ) ;
#56001 = CARTESIAN_POINT ( 'NONE',  ( 29.48437500061451644, -4.541064518000419881, 2.621784821874995952 ) ) ;
#56002 = CARTESIAN_POINT ( 'NONE',  ( 4.243569643749999898, 19.14687500061451431, 32.45002607614398471 ) ) ;
#56003 = CARTESIAN_POINT ( 'NONE',  ( 9.328125000614518214, 6.421520780324663323E-16, -5.243569643749999010 ) ) ;
#56005 =( BOUNDED_CURVE ( )  B_SPLINE_CURVE ( 2, ( #57491, #69673, #51962, #53407, #23509, #68592, #1361 ),
 .UNSPECIFIED., .F., .F. ) 
 B_SPLINE_CURVE_WITH_KNOTS ( ( 3, 2, 2, 3 ),
 ( 0.8300000000000000711, 0.8333333333333334814, 0.8366666666666666696, 0.8399999999999999689 ),
 .UNSPECIFIED. ) 
 CURVE ( )  GEOMETRIC_REPRESENTATION_ITEM ( )  RATIONAL_B_SPLINE_CURVE ( ( 0.9999999999999955591, 0.8660254037844431485, 1.000000000000000000, 0.8660254037844387076, 1.000000000000000000, 0.8660254037844387076, 1.000000000000000000 ) ) 
 REPRESENTATION_ITEM ( '' )  );
#56004 = CARTESIAN_POINT ( 'NONE',  ( -1.999999999999997113, 15.23750000122903536, 33.46410161513775705 ) ) ;
#56006 = CARTESIAN_POINT ( 'NONE',  ( 7.321875000614516793, 3.027376345333611329, 5.243569643749999010 ) ) ;
#56007 = CARTESIAN_POINT ( 'NONE',  ( 3.957880893006796352, 3.055449414859130464, -4.228749118501266224 ) ) ;
#56008 = CARTESIAN_POINT ( 'NONE',  ( 7.115625000614516082, 3.027376345333613106, -5.243569643749998122 ) ) ;
#56009 = CARTESIAN_POINT ( 'NONE',  ( 11.29687500061451644, 6.054752690667223547, 3.707466751127219781E-16 ) ) ;
#56010 = SURFACE_STYLE_USAGE ( .BOTH. , #34186 ) ;
#56011 = CARTESIAN_POINT ( 'NONE',  ( 19.50000000122903288, -2.886751345948125991, -5.000000000000000000 ) ) ;
#56012 = CARTESIAN_POINT ( 'NONE',  ( 8.896875000614517859, -3.027376345333610441, -5.243569643749999898 ) ) ;
#56013 = CARTESIAN_POINT ( 'NONE',  ( 10.15312500061451750, -4.541064518000417216, -2.621784821875001281 ) ) ;
#56014 = CARTESIAN_POINT ( 'NONE',  ( 4.000000000000000000, 12.50000000000000000, 30.00000000000000000 ) ) ;
#56015 = CARTESIAN_POINT ( 'NONE',  ( 24.76875000122903003, -5.773502691896255534, -1.060575238724906372E-15 ) ) ;
#56016 = CARTESIAN_POINT ( 'NONE',  ( 19.05937500061451928, 0.000000000000000000, 5.243569643749999010 ) ) ;
#56017 = LINE ( 'NONE', #29027, #30157 ) ;
#56018 = CARTESIAN_POINT ( 'NONE',  ( 26.42812500061451431, 6.421520780324663323E-16, -5.243569643749999010 ) ) ;
#56019 = CARTESIAN_POINT ( 'NONE',  ( 11.20312500061451644, 4.541064518000418104, -2.621784821874998173 ) ) ;
#56020 = EDGE_CURVE ( 'NONE', #6086, #69242, #20533, .T. ) ;
#56021 = CARTESIAN_POINT ( 'NONE',  ( -4.999999999999998224, -2.928932188134522718, 4.999999999999998224 ) ) ;
#56022 = CARTESIAN_POINT ( 'NONE',  ( -2.121784821874999949, 12.58437500061451786, -33.67503911421598417 ) ) ;
#56023 = CARTESIAN_POINT ( 'NONE',  ( 12.93750000122903465, 4.330127018922191873, 2.499999999999999556 ) ) ;
#56024 = CARTESIAN_POINT ( 'NONE',  ( 28.26562500061451289, 3.027376345333613106, -5.243569643749998122 ) ) ;
#56025 = CARTESIAN_POINT ( 'NONE',  ( -4.243569643749999898, 15.30312500061451608, -30.00000000000000000 ) ) ;
#56026 = CARTESIAN_POINT ( 'NONE',  ( 15.93750000122903110, 6.123233995736764310E-16, -4.999999999999998224 ) ) ;
#56027 = CIRCLE ( 'NONE', #67775, 4.999999999999998224 ) ;
#56028 = CARTESIAN_POINT ( 'NONE',  ( 12.56250000000000178, -5.773502691896255534, -1.060575238724906372E-15 ) ) ;
#56029 = CARTESIAN_POINT ( 'NONE',  ( 13.85625000122903216, 0.000000000000000000, 4.999999999999998224 ) ) ;
#56030 = CARTESIAN_POINT ( 'NONE',  ( 23.35312500061451857, 4.541064518000418104, -2.621784821874998173 ) ) ;
#56031 = CARTESIAN_POINT ( 'NONE',  ( 6.796875000614516438, 6.054752690667223547, 3.707466751127219781E-16 ) ) ;
#56032 = CARTESIAN_POINT ( 'NONE',  ( 7.575000001229033053, 2.886751345948126879, 4.999999999999999112 ) ) ;
#56033 = CARTESIAN_POINT ( 'NONE',  ( 15.41250000122903252, -4.330127018922190985, -2.500000000000001332 ) ) ;
#56034 = CARTESIAN_POINT ( 'NONE',  ( 14.27812500061451573, 6.421520780324663323E-16, -5.243569643749999010 ) ) ;
#56035 = CARTESIAN_POINT ( 'NONE',  ( 17.54062500061451502, 6.054752690667223547, 3.707466751127219781E-16 ) ) ;
#56036 = CARTESIAN_POINT ( 'NONE',  ( 25.46250000122903501, 4.330127018922192761, -2.499999999999997780 ) ) ;
#56037 = CARTESIAN_POINT ( 'NONE',  ( 27.86250000122903359, 0.000000000000000000, 4.999999999999998224 ) ) ;
#56038 = CARTESIAN_POINT ( 'NONE',  ( 22.46250000000000213, -5.773502691896255534, -1.060575238724906372E-15 ) ) ;
#56039 = VECTOR ( 'NONE', #62481, 1000.000000000000000 ) ;
#56040 = CARTESIAN_POINT ( 'NONE',  ( 26.52187500061451431, 3.027376345333613106, -5.243569643749998122 ) ) ;
#56041 = DIRECTION ( 'NONE',  ( 1.000000000000000000, 0.000000000000000000, 0.000000000000000000 ) ) ;
#56042 = CARTESIAN_POINT ( 'NONE',  ( 9.900000001229033231, -2.886751345948129988, 4.999999999999997335 ) ) ;
#56043 = CARTESIAN_POINT ( 'NONE',  ( 27.00937500061451857, 4.541064518000418104, -2.621784821874998173 ) ) ;
#56044 = CARTESIAN_POINT ( 'NONE',  ( 10.31250000122903288, 0.000000000000000000, 4.999999999999998224 ) ) ;
#56045 = CARTESIAN_POINT ( 'NONE',  ( 6.009375000614519458, 0.000000000000000000, 5.243569643749999010 ) ) ;
#56046 = CARTESIAN_POINT ( 'NONE',  ( 22.94062500061451715, 6.054752690667223547, 3.707466751127219781E-16 ) ) ;
#56047 = CARTESIAN_POINT ( 'NONE',  ( 1.878215178124997609, 14.92812499938548321, 33.25316411605952993 ) ) ;
#56048 = CARTESIAN_POINT ( 'NONE',  ( 26.15625000122903288, -4.330127018922190985, -2.500000000000001332 ) ) ;
#56049 = CARTESIAN_POINT ( 'NONE',  ( 9.084375000614517859, 4.541064518000418104, 2.621784821874999949 ) ) ;
#56050 = CARTESIAN_POINT ( 'NONE',  ( 9.187500001229034652, 6.123233995736764310E-16, -4.999999999999998224 ) ) ;
#56051 = CARTESIAN_POINT ( 'NONE',  ( 3.121875000614518836, 3.027376345333613106, -5.243569643749998122 ) ) ;
#56052 = CARTESIAN_POINT ( 'NONE',  ( 7.246875000614518392, 6.054752690667223547, 3.707466751127219781E-16 ) ) ;
#56053 = CARTESIAN_POINT ( 'NONE',  ( 28.17187500061451644, -6.054752690667223547, -1.112240025338166033E-15 ) ) ;
#56054 = CARTESIAN_POINT ( 'NONE',  ( 21.89999999999999858, 0.000000000000000000, 4.999999999999998224 ) ) ;
#56055 = CARTESIAN_POINT ( 'NONE',  ( 19.87500000000000000, 6.123233995736764310E-16, -4.999999999999998224 ) ) ;
#56056 = VERTEX_POINT ( 'NONE', #69211 ) ;
#56057 = CARTESIAN_POINT ( 'NONE',  ( 26.21249999999999858, 2.886751345948129099, -4.999999999999998224 ) ) ;
#56058 = CARTESIAN_POINT ( 'NONE',  ( 27.72187500061451715, -6.054752690667223547, -1.112240025338166033E-15 ) ) ;
#56059 = ORIENTED_EDGE ( 'NONE', *, *, #71580, .F. ) ;
#56060 = CARTESIAN_POINT ( 'NONE',  ( 18.59062500061451573, -3.027376345333614438, 5.243569643749998122 ) ) ;
#56061 = CARTESIAN_POINT ( 'NONE',  ( 7.490625000614516082, -3.027376345333610441, -5.243569643749999898 ) ) ;
#56062 = CARTESIAN_POINT ( 'NONE',  ( 21.57187500061451146, 4.119189519843966529, 2.378215178124999607 ) ) ;
#56063 = CARTESIAN_POINT ( 'NONE',  ( 5.484375000614518214, 4.541064518000418104, 2.621784821874999949 ) ) ;
#56064 = CARTESIAN_POINT ( 'NONE',  ( 16.57500000122903216, 2.886751345948126879, 4.999999999999999112 ) ) ;
#56065 = VECTOR ( 'NONE', #17194, 1000.000000000000000 ) ;
#56066 = CARTESIAN_POINT ( 'NONE',  ( 24.89999999999999858, 4.330127018922192761, -2.499999999999997780 ) ) ;
#56067 = CARTESIAN_POINT ( 'NONE',  ( 15.82499999999999929, 6.123233995736764310E-16, -4.999999999999998224 ) ) ;
#56068 = CARTESIAN_POINT ( 'NONE',  ( 7.434375000614519280, -4.541064518000419881, 2.621784821874995952 ) ) ;
#56069 = CARTESIAN_POINT ( 'NONE',  ( 12.75937500061451857, 0.000000000000000000, 5.243569643749999010 ) ) ;
#56070 = CARTESIAN_POINT ( 'NONE',  ( 22.35937500061451644, -4.541064518000417216, -2.621784821875001281 ) ) ;
#56071 = CARTESIAN_POINT ( 'NONE',  ( -3.999999999999997335, 14.63750000000000107, -27.69059892324149530 ) ) ;
#56072 = ORIENTED_EDGE ( 'NONE', *, *, #67743, .T. ) ;
#56073 = CARTESIAN_POINT ( 'NONE',  ( 3.459375000614519635, -4.541064518000417216, -2.621784821875001281 ) ) ;
#56074 = CARTESIAN_POINT ( 'NONE',  ( 10.65000000000000036, 0.000000000000000000, 4.999999999999998224 ) ) ;
#56075 = VECTOR ( 'NONE', #14895, 1000.000000000000000 ) ;
#56076 = CARTESIAN_POINT ( 'NONE',  ( 7.059375000614518392, -4.541064518000417216, -2.621784821875001281 ) ) ;
#56077 = CARTESIAN_POINT ( 'NONE',  ( 3.756430356249998770, 14.85312499938548392, 32.16877607737302469 ) ) ;
#56078 = CARTESIAN_POINT ( 'NONE',  ( 21.67500000000000071, 6.123233995736764310E-16, -4.999999999999998224 ) ) ;
#56079 = CARTESIAN_POINT ( 'NONE',  ( 16.75312500061451715, 0.000000000000000000, 5.243569643749999010 ) ) ;
#56080 = CARTESIAN_POINT ( 'NONE',  ( 1.999999999999997335, 17.82499999999999929, 33.46410161513775705 ) ) ;
#56081 = CARTESIAN_POINT ( 'NONE',  ( 45.00000000000000000, 0.000000000000000000, 0.000000000000000000 ) ) ;
#56082 = CARTESIAN_POINT ( 'NONE',  ( 23.33437500061451786, 5.824947211148865298E-16, -4.756430356249998326 ) ) ;
#56083 = CARTESIAN_POINT ( 'NONE',  ( 10.26562500061451644, 3.027376345333613106, -5.243569643749998122 ) ) ;
#56084 = CARTESIAN_POINT ( 'NONE',  ( 27.04687500061451644, 6.054752690667223547, 3.707466751127219781E-16 ) ) ;
#56085 = CARTESIAN_POINT ( 'NONE',  ( 12.86250000000000071, 2.886751345948126879, 4.999999999999998224 ) ) ;
#56086 = CARTESIAN_POINT ( 'NONE',  ( 28.77187500061451431, 3.027376345333613106, -5.243569643749998122 ) ) ;
#56087 = CARTESIAN_POINT ( 'NONE',  ( 10.05000000000000071, 4.330127018922192761, -2.499999999999997780 ) ) ;
#56088 = CARTESIAN_POINT ( 'NONE',  ( 3.999999999999998668, 15.87500000122903465, 27.69059892324149175 ) ) ;
#56089 = CARTESIAN_POINT ( 'NONE',  ( 9.975000001229034297, -5.773502691896255534, -1.060575238724906372E-15 ) ) ;
#56090 = VECTOR ( 'NONE', #18058, 1000.000000000000000 ) ;
#56091 = CARTESIAN_POINT ( 'NONE',  ( 19.05937500061451928, 0.000000000000000000, 5.243569643749999010 ) ) ;
#56092 = CARTESIAN_POINT ( 'NONE',  ( 14.82187500061451679, 3.027376345333613106, -5.243569643749998122 ) ) ;
#56093 = CARTESIAN_POINT ( 'NONE',  ( 9.300000001229031810, 5.773502691896255534, 3.535250795749688401E-16 ) ) ;
#56094 = ORIENTED_EDGE ( 'NONE', *, *, #703, .F. ) ;
#56095 = CARTESIAN_POINT ( 'NONE',  ( 14.01562500061451644, 3.027376345333611329, 5.243569643749999010 ) ) ;
#56096 = CARTESIAN_POINT ( 'NONE',  ( 27.26250000122903216, 4.330127018922192761, -2.499999999999997780 ) ) ;
#56097 = CARTESIAN_POINT ( 'NONE',  ( 14.25937500061451679, -4.541064518000417216, -2.621784821875001281 ) ) ;
#56098 = CARTESIAN_POINT ( 'NONE',  ( 27.24375000122903145, 5.773502691896255534, 3.535250795749688401E-16 ) ) ;
#56099 = CARTESIAN_POINT ( 'NONE',  ( 16.04062500061451857, -3.027376345333610441, -5.243569643749999898 ) ) ;
#56100 = CARTESIAN_POINT ( 'NONE',  ( 1.071796769724491227, 20.18615380933863079, 26.00000000000000000 ) ) ;
#56101 = CARTESIAN_POINT ( 'NONE',  ( 26.74687500061451573, -3.027376345333614438, 5.243569643749998122 ) ) ;
#56102 = CARTESIAN_POINT ( 'NONE',  ( -3.000416591977282496E-16, 10.24062500061451608, 25.09994784771203058 ) ) ;
#56103 = CARTESIAN_POINT ( 'NONE',  ( 14.74687500061451573, -3.027376345333610441, -5.243569643749999898 ) ) ;
#56104 = CARTESIAN_POINT ( 'NONE',  ( 14.62500000122903288, 2.886751345948129099, -4.999999999999998224 ) ) ;
#56105 = CARTESIAN_POINT ( 'NONE',  ( 30.00000000000000000, 0.000000000000000000, 4.999999999999998224 ) ) ;
#56106 = CYLINDRICAL_SURFACE ( 'NONE', #23839, 4.000000000000000000 ) ;
#56107 = CARTESIAN_POINT ( 'NONE',  ( 20.82187500061451857, 3.027376345333611329, 5.243569643749999010 ) ) ;
#56108 = CARTESIAN_POINT ( 'NONE',  ( 20.62500000122903288, 2.886751345948126879, 4.999999999999999112 ) ) ;
#56109 = EDGE_CURVE ( 'NONE', #55464, #18961, #43221, .T. ) ;
#56110 = CARTESIAN_POINT ( 'NONE',  ( 15.30937500061451750, 4.541064518000418104, -2.621784821874998173 ) ) ;
#56111 = CARTESIAN_POINT ( 'NONE',  ( -4.243569643749999898, 12.20937500061451608, 30.00000000000000000 ) ) ;
#56112 = CARTESIAN_POINT ( 'NONE',  ( 16.41562500061451857, -6.054752690667223547, -1.112240025338166033E-15 ) ) ;
#56113 = VERTEX_POINT ( 'NONE', #49496 ) ;
#56114 = EDGE_LOOP ( 'NONE', ( #4185, #11040, #14094, #2299 ) ) ;
#56115 = CARTESIAN_POINT ( 'NONE',  ( 20.88749999999999929, 5.773502691896255534, 3.535250795749688894E-16 ) ) ;
#56116 = DIRECTION ( 'NONE',  ( 0.000000000000000000, 0.000000000000000000, -1.000000000000000000 ) ) ;
#56117 = CARTESIAN_POINT ( 'NONE',  ( 24.70312500061451644, 4.541064518000418104, -2.621784821874998173 ) ) ;
#56118 = CARTESIAN_POINT ( 'NONE',  ( 4.907911205059083602E-16, 5.000000000000000000, 33.99999999999999289 ) ) ;
#56119 = CARTESIAN_POINT ( 'NONE',  ( 16.87500000122903288, 2.886751345948129099, -4.999999999999998224 ) ) ;
#56120 = CARTESIAN_POINT ( 'NONE',  ( 21.62812500061451360, 4.541064518000418104, 2.621784821874999949 ) ) ;
#56121 = CARTESIAN_POINT ( 'NONE',  ( 24.62812500061451715, 6.421520780324663323E-16, -5.243569643749999010 ) ) ;
#56122 = CARTESIAN_POINT ( 'NONE',  ( 5.203125000614518214, -4.541064518000417216, -2.621784821875001281 ) ) ;
#56123 = ORIENTED_EDGE ( 'NONE', *, *, #49317, .T. ) ;
#56124 = CARTESIAN_POINT ( 'NONE',  ( 29.81250000000000000, 2.886751345948129099, -4.999999999999998224 ) ) ;
#56125 = CARTESIAN_POINT ( 'NONE',  ( 1.626862140677534273E-15, 10.32500000122903572, -26.00000000000000355 ) ) ;
#56126 = CARTESIAN_POINT ( 'NONE',  ( 12.75937500061451857, 0.000000000000000000, 4.756430356249998326 ) ) ;
#56127 = FACE_OUTER_BOUND ( 'NONE', #34028, .T. ) ;
#56128 = CARTESIAN_POINT ( 'NONE',  ( -2.000000000000000000, 11.03750000122903430, -33.46410161513775705 ) ) ;
#56129 = CARTESIAN_POINT ( 'NONE',  ( -3.000416591977282496E-16, 18.39687500061451786, -34.90005215228797653 ) ) ;
#56130 = CARTESIAN_POINT ( 'NONE',  ( 9.449999999999999289, -4.330127018922190985, -2.500000000000001332 ) ) ;
#56131 = CARTESIAN_POINT ( 'NONE',  ( 3.262500001229035718, -4.330127018922190985, -2.500000000000001332 ) ) ;
#56132 = CARTESIAN_POINT ( 'NONE',  ( 12.08437500061451608, 6.421520780324663323E-16, -5.243569643749999010 ) ) ;
#56133 = CARTESIAN_POINT ( 'NONE',  ( 4.471875000614518925, 3.027376345333613106, -5.243569643749998122 ) ) ;
#56134 = CARTESIAN_POINT ( 'NONE',  ( -1.626862140677534273E-15, 19.13749999999999929, 34.00000000000000000 ) ) ;
#56135 = AXIS2_PLACEMENT_3D ( 'NONE', #47253, #36528, #52794 ) ;
#56136 = CARTESIAN_POINT ( 'NONE',  ( -1.999999999999997113, 10.73750000122903536, 33.46410161513775705 ) ) ;
#56137 = CARTESIAN_POINT ( 'NONE',  ( 10.02187500061451964, 3.027376345333611329, 5.243569643749999010 ) ) ;
#56138 = FACE_OUTER_BOUND ( 'NONE', #17747, .T. ) ;
#56139 = CARTESIAN_POINT ( 'NONE',  ( 19.67812500061451786, 6.421520780324663323E-16, -5.243569643749999010 ) ) ;
#56140 = CARTESIAN_POINT ( 'NONE',  ( 29.09999999999999787, 0.000000000000000000, 4.999999999999998224 ) ) ;
#56141 = CARTESIAN_POINT ( 'NONE',  ( -3.000416591977282496E-16, 17.89062500061459104, 25.09994784771203058 ) ) ;
#56142 = CARTESIAN_POINT ( 'NONE',  ( 24.53437500061451715, -4.541064518000419881, 2.621784821874995952 ) ) ;
#56143 = CARTESIAN_POINT ( 'NONE',  ( 2.828911952606729230, -4.122772994526751056, 3.124276913337163286 ) ) ;
#56144 = CARTESIAN_POINT ( 'NONE',  ( 28.95000000122903572, -2.886751345948125991, -5.000000000000000000 ) ) ;
#56145 = CARTESIAN_POINT ( 'NONE',  ( 19.84687500061451360, 0.000000000000000000, 4.756430356249998326 ) ) ;
#56146 = CARTESIAN_POINT ( 'NONE',  ( 26.09062500061451573, 6.054752690667223547, 3.707466751127219781E-16 ) ) ;
#56147 = CARTESIAN_POINT ( 'NONE',  ( 15.51562500061451644, -6.054752690667223547, -1.112240025338166033E-15 ) ) ;
#56148 = CARTESIAN_POINT ( 'NONE',  ( 15.16875000122903394, 2.886751345948126879, 4.999999999999999112 ) ) ;
#56149 = CARTESIAN_POINT ( 'NONE',  ( 11.25937500061451679, 4.541064518000418104, -2.621784821874998173 ) ) ;
#56150 = CARTESIAN_POINT ( 'NONE',  ( 29.62500000000000000, -4.330127018922194537, 2.499999999999995559 ) ) ;
#56151 = CARTESIAN_POINT ( 'NONE',  ( 23.85000000122903430, -2.886751345948129988, 4.999999999999997335 ) ) ;
#56152 = CARTESIAN_POINT ( 'NONE',  ( 26.96249999999999858, -5.773502691896255534, -1.060575238724906372E-15 ) ) ;
#56153 = CARTESIAN_POINT ( 'NONE',  ( 14.89687500061451786, 6.054752690667223547, 3.707466751127219781E-16 ) ) ;
#56154 = CARTESIAN_POINT ( 'NONE',  ( 29.63437500061451502, 6.421520780324663323E-16, -5.243569643749999010 ) ) ;
#56155 = DIRECTION ( 'NONE',  ( 0.000000000000000000, 0.000000000000000000, 1.000000000000000000 ) ) ;
#56156 = CARTESIAN_POINT ( 'NONE',  ( 18.37500000000000355, -4.330127018922194537, 2.499999999999995559 ) ) ;
#56157 = CARTESIAN_POINT ( 'NONE',  ( 23.78437500061451360, 6.421520780324663323E-16, -5.243569643749999010 ) ) ;
#56158 = CARTESIAN_POINT ( 'NONE',  ( 14.29687500061451821, -3.027376345333610441, -5.243569643749999898 ) ) ;
#56159 = CARTESIAN_POINT ( 'NONE',  ( -1.878215178124999163, 16.50312499938548427, 26.74683588394047007 ) ) ;
#56160 = CARTESIAN_POINT ( 'NONE',  ( 28.91250000000000497, 2.886751345948129099, -4.999999999999998224 ) ) ;
#56161 = CARTESIAN_POINT ( 'NONE',  ( 3.112500001229034918, 0.000000000000000000, 4.999999999999998224 ) ) ;
#56162 = CARTESIAN_POINT ( 'NONE',  ( 5.137500000000000178, 5.773502691896255534, 3.535250795749688894E-16 ) ) ;
#56163 = CARTESIAN_POINT ( 'NONE',  ( 7.621875000614515727, 4.119189519843966529, 2.378215178124999607 ) ) ;
#56164 = CARTESIAN_POINT ( 'NONE',  ( 16.86562500061451786, -6.054752690667223547, -1.112240025338166033E-15 ) ) ;
#56165 = CARTESIAN_POINT ( 'NONE',  ( 8.437500000000000000, -2.886751345948129988, 4.999999999999997335 ) ) ;
#56166 = CARTESIAN_POINT ( 'NONE',  ( 2.840625000614518392, -3.027376345333614438, 5.243569643749998122 ) ) ;
#56167 = CARTESIAN_POINT ( 'NONE',  ( 18.00000000000000355, -4.330127018922190985, -2.500000000000001332 ) ) ;
#56168 = CARTESIAN_POINT ( 'NONE',  ( 4.243569643749999898, 13.69062500061451537, 32.45002607614398471 ) ) ;
#56169 = CARTESIAN_POINT ( 'NONE',  ( 4.000000000000000000, 18.38750000000000284, 27.69059892324149885 ) ) ;
#56170 = CARTESIAN_POINT ( 'NONE',  ( 21.60000000122903430, -2.886751345948129988, 4.999999999999997335 ) ) ;
#56171 = CARTESIAN_POINT ( 'NONE',  ( 2.154264117376507137, 9.766972526336937577, 35.60336559010523416 ) ) ;
#56172 = CARTESIAN_POINT ( 'NONE',  ( 26.89687500061451431, -3.027376345333610441, -5.243569643749999898 ) ) ;
#56173 = VECTOR ( 'NONE', #69192, 1000.000000000000000 ) ;
#56174 = ORIENTED_EDGE ( 'NONE', *, *, #1971, .T. ) ;
#56175 = CARTESIAN_POINT ( 'NONE',  ( 17.76562500061451644, -6.054752690667223547, -1.112240025338166033E-15 ) ) ;
#56176 = CARTESIAN_POINT ( 'NONE',  ( 22.15312500061451573, 0.000000000000000000, 5.243569643749999010 ) ) ;
#56177 = CARTESIAN_POINT ( 'NONE',  ( 22.58437500061451431, 4.541064518000418104, 2.621784821874999949 ) ) ;
#56178 = CARTESIAN_POINT ( 'NONE',  ( 7.687500000000000000, -2.886751345948125991, -5.000000000000000000 ) ) ;
#56179 = CARTESIAN_POINT ( 'NONE',  ( 9.815625000614518925, 3.027376345333613106, -5.243569643749998122 ) ) ;
#56180 = CARTESIAN_POINT ( 'NONE',  ( 24.40312500061451573, 0.000000000000000000, 5.243569643749999010 ) ) ;
#56181 = CARTESIAN_POINT ( 'NONE',  ( 14.93437500061451750, 4.541064518000418104, 2.621784821874999949 ) ) ;
#56182 = CARTESIAN_POINT ( 'NONE',  ( 19.54687500061451644, -3.027376345333614438, 5.243569643749998122 ) ) ;
#56183 = CARTESIAN_POINT ( 'NONE',  ( 19.34999999999999787, -4.330127018922190985, -2.500000000000001332 ) ) ;
#56184 = CARTESIAN_POINT ( 'NONE',  ( 2.121784821874999061, 16.95312500061451999, 26.32496088578401583 ) ) ;
#56185 = CARTESIAN_POINT ( 'NONE',  ( 22.53750000122903430, -4.330127018922194537, 2.499999999999995559 ) ) ;
#56186 = CARTESIAN_POINT ( 'NONE',  ( 15.49687500061451750, -2.746126346562646425, 4.756430356249996549 ) ) ;
#56187 = CARTESIAN_POINT ( 'NONE',  ( 11.54062500061451857, -3.027376345333610441, -5.243569643749999898 ) ) ;
#56188 = CARTESIAN_POINT ( 'NONE',  ( 5.334375000614517859, 6.421520780324663323E-16, -5.243569643749999010 ) ) ;
#56189 = CARTESIAN_POINT ( 'NONE',  ( 3.909375000614518481, -4.541064518000417216, -2.621784821875001281 ) ) ;
#56190 = ORIENTED_EDGE ( 'NONE', *, *, #13900, .F. ) ;
#56191 = CARTESIAN_POINT ( 'NONE',  ( 28.28437500061451715, 6.421520780324663323E-16, -5.243569643749999010 ) ) ;
#56192 = CARTESIAN_POINT ( 'NONE',  ( 18.14062500061451644, -3.027376345333614438, 5.243569643749998122 ) ) ;
#56193 = CARTESIAN_POINT ( 'NONE',  ( 27.03750000122903430, -4.330127018922194537, 2.499999999999995559 ) ) ;
#56194 = ADVANCED_FACE ( 'NONE', ( #38035 ), #71665, .T. ) ;
#56195 = CARTESIAN_POINT ( 'NONE',  ( 27.77812500061451573, 6.421520780324663323E-16, -5.243569643749999010 ) ) ;
#56196 = CARTESIAN_POINT ( 'NONE',  ( 25.13437500061451502, 6.421520780324663323E-16, -5.243569643749999010 ) ) ;
#56197 = CARTESIAN_POINT ( 'NONE',  ( 17.61562500061451786, 3.027376345333611329, 5.243569643749999010 ) ) ;
#56198 = CARTESIAN_POINT ( 'NONE',  ( 4.243569643749999010, 18.32187500061451502, 27.54997392385601174 ) ) ;
#56199 = CARTESIAN_POINT ( 'NONE',  ( 23.99062500061451786, -3.027376345333614438, 5.243569643749998122 ) ) ;
#56200 = CARTESIAN_POINT ( 'NONE',  ( 4.162500001229033408, -4.330127018922190985, -2.500000000000001332 ) ) ;
#56201 = ORIENTED_EDGE ( 'NONE', *, *, #19460, .F. ) ;
#56202 = CARTESIAN_POINT ( 'NONE',  ( 26.81250000000000000, 2.886751345948126879, 4.999999999999999112 ) ) ;
#56203 = CARTESIAN_POINT ( 'NONE',  ( -2.000000000000000000, 14.52500000000000036, -33.46410161513775705 ) ) ;
#56204 = CARTESIAN_POINT ( 'NONE',  ( 3.756430356249998770, 17.21562499938548285, 32.16877607737302469 ) ) ;
#56205 = CARTESIAN_POINT ( 'NONE',  ( 4.621875000614516615, 3.027376345333611329, 5.243569643749999010 ) ) ;
#56206 = CARTESIAN_POINT ( 'NONE',  ( 10.34062500061451750, 6.054752690667223547, 3.707466751127219781E-16 ) ) ;
#56207 = CARTESIAN_POINT ( 'NONE',  ( 7.359375000614516438, 0.000000000000000000, 5.243569643749999010 ) ) ;
#56208 = CARTESIAN_POINT ( 'NONE',  ( 25.16250000122903074, 0.000000000000000000, 4.999999999999998224 ) ) ;
#56209 =( BOUNDED_CURVE ( )  B_SPLINE_CURVE ( 2, ( #8821, #4026, #38357, #32819, #31725, #60511, #55357, #3291, #48356 ),
 .UNSPECIFIED., .F., .F. ) 
 B_SPLINE_CURVE_WITH_KNOTS ( ( 3, 2, 2, 2, 3 ),
 ( 0.03260869565217391908, 0.03623188405797101580, 0.04347826086956521618, 0.05072463768115942351, 0.05434782608695652717 ),
 .UNSPECIFIED. ) 
 CURVE ( )  GEOMETRIC_REPRESENTATION_ITEM ( )  RATIONAL_B_SPLINE_CURVE ( ( 0.9330127018922192983, 0.9330127018922194093, 1.000000000000000000, 0.8660254037844387076, 1.000000000000000000, 0.8660254037844387076, 1.000000000000000000, 0.9330127018922192983, 0.9330127018922194093 ) ) 
 REPRESENTATION_ITEM ( '' )  );
#56210 = CARTESIAN_POINT ( 'NONE',  ( 13.84687500061451537, -3.027376345333610441, -5.243569643749999898 ) ) ;
#56211 = CARTESIAN_POINT ( 'NONE',  ( 29.50312500061451360, -4.541064518000417216, -2.621784821875001281 ) ) ;
#56212 = CARTESIAN_POINT ( 'NONE',  ( 28.04999999999999716, 4.330127018922192761, -2.499999999999997780 ) ) ;
#56213 = CARTESIAN_POINT ( 'NONE',  ( 27.08437500061451786, 4.541064518000418104, 2.621784821874999949 ) ) ;
#56214 = FACE_OUTER_BOUND ( 'NONE', #63418, .T. ) ;
#56215 = CARTESIAN_POINT ( 'NONE',  ( 13.04062500061451502, 6.054752690667223547, 3.707466751127219781E-16 ) ) ;
#56216 = VERTEX_POINT ( 'NONE', #11053 ) ;
#56217 = CARTESIAN_POINT ( 'NONE',  ( 9.140625000614518214, -3.027376345333614438, 5.243569643749998122 ) ) ;
#56218 = CARTESIAN_POINT ( 'NONE',  ( 5.465625000614517504, 3.027376345333611329, 5.243569643749999010 ) ) ;
#56219 = CARTESIAN_POINT ( 'NONE',  ( 17.97187500061451715, 2.746126346562645981, -4.756430356249997438 ) ) ;
#56220 = FACE_OUTER_BOUND ( 'NONE', #54967, .T. ) ;
#56221 = CARTESIAN_POINT ( 'NONE',  ( 15.82499999999999929, 6.123233995736764310E-16, -4.999999999999998224 ) ) ;
#56222 =( BOUNDED_CURVE ( )  B_SPLINE_CURVE ( 2, ( #40215, #18740, #24657, #64180, #36112, #58633, #51296, #697, #62737 ),
 .UNSPECIFIED., .F., .F. ) 
 B_SPLINE_CURVE_WITH_KNOTS ( ( 3, 2, 2, 2, 3 ),
 ( 0.6527777777777777901, 0.6574074074074074403, 0.6666666666666666297, 0.6759259259259259300, 0.6805555555555555802 ),
 .UNSPECIFIED. ) 
 CURVE ( )  GEOMETRIC_REPRESENTATION_ITEM ( )  RATIONAL_B_SPLINE_CURVE ( ( 0.9330127018922194093, 0.9330127018922194093, 1.000000000000000000, 0.8660254037844387076, 1.000000000000000000, 0.8660254037844387076, 1.000000000000000000, 0.9330127018922194093, 0.9330127018922194093 ) ) 
 REPRESENTATION_ITEM ( '' )  );
#56223 = CARTESIAN_POINT ( 'NONE',  ( 14.89687500061451786, 6.054752690667223547, 3.707466751127219781E-16 ) ) ;
#56224 = CARTESIAN_POINT ( 'NONE',  ( 12.52500000122903145, 2.886751345948126879, 4.999999999999999112 ) ) ;
#56225 = CARTESIAN_POINT ( 'NONE',  ( 18.93750000000000000, -2.886751345948125991, -5.000000000000000000 ) ) ;
#56226 = CARTESIAN_POINT ( 'NONE',  ( 21.12187500061451573, 3.027376345333613106, -5.243569643749998122 ) ) ;
#56227 = CARTESIAN_POINT ( 'NONE',  ( -4.243569643749999898, 13.91562500061451679, -32.45002607614398471 ) ) ;
#56228 = CARTESIAN_POINT ( 'NONE',  ( -1.487416814333745711E-14, 16.96250000000000213, 34.00000000000000000 ) ) ;
#56229 = CARTESIAN_POINT ( 'NONE',  ( 24.60937500061451644, 2.746126346562645981, -4.756430356249997438 ) ) ;
#56230 = CARTESIAN_POINT ( 'NONE',  ( 25.71562500061451573, 3.027376345333611329, 5.243569643749999010 ) ) ;
#56231 = CARTESIAN_POINT ( 'NONE',  ( -2.000000000000000000, 19.47499999999999787, -33.46410161513775705 ) ) ;
#56232 = CARTESIAN_POINT ( 'NONE',  ( 17.55000000000000071, -4.330127018922190985, -2.500000000000001332 ) ) ;
#56233 = CARTESIAN_POINT ( 'NONE',  ( 27.59999999999999787, 4.330127018922192761, -2.499999999999997780 ) ) ;
#56234 = ADVANCED_FACE ( 'NONE', ( #39136 ), #38780, .F. ) ;
#56235 = CARTESIAN_POINT ( 'NONE',  ( 10.00312500061451715, 0.000000000000000000, 5.243569643749999010 ) ) ;
#56236 = CARTESIAN_POINT ( 'NONE',  ( 26.59687500061451360, 0.000000000000000000, 4.756430356249998326 ) ) ;
#56237 =( BOUNDED_CURVE ( )  B_SPLINE_CURVE ( 2, ( #7767, #63552, #29216, #790, #11864, #52473, #56917 ),
 .UNSPECIFIED., .F., .F. ) 
 B_SPLINE_CURVE_WITH_KNOTS ( ( 3, 2, 2, 3 ),
 ( 0.1583333333333333814, 0.1611111111111111771, 0.1638888888888889173, 0.1666666666666666852 ),
 .UNSPECIFIED. ) 
 CURVE ( )  GEOMETRIC_REPRESENTATION_ITEM ( )  RATIONAL_B_SPLINE_CURVE ( ( 0.9999999999999973355, 0.8660254037844413721, 1.000000000000000000, 0.8660254037844387076, 1.000000000000000000, 0.8660254037844373753, 1.000000000000001332 ) ) 
 REPRESENTATION_ITEM ( '' )  );
#56238 = CARTESIAN_POINT ( 'NONE',  ( 18.08437500061451431, 4.541064518000418104, 2.621784821874999949 ) ) ;
#56239 = CARTESIAN_POINT ( 'NONE',  ( 13.24687500061451750, -4.119189519843965641, -2.378215178125001383 ) ) ;
#56240 = EDGE_CURVE ( 'NONE', #26559, #72520, #55761, .T. ) ;
#56241 = CARTESIAN_POINT ( 'NONE',  ( 4.265625000614517326, -6.054752690667223547, -1.112240025338166033E-15 ) ) ;
#56242 = CARTESIAN_POINT ( 'NONE',  ( 10.54687500061451644, -3.027376345333614438, 5.243569643749998122 ) ) ;
#56243 = ORIENTED_EDGE ( 'NONE', *, *, #16399, .T. ) ;
#56244 = CARTESIAN_POINT ( 'NONE',  ( 22.13437500061451502, 4.541064518000418104, 2.621784821874999949 ) ) ;
#56245 = LINE ( 'NONE', #456, #64236 ) ;
#56246 = CARTESIAN_POINT ( 'NONE',  ( 29.84999999999999787, 4.330127018922192761, -2.499999999999997780 ) ) ;
#56247 = CARTESIAN_POINT ( 'NONE',  ( 6.225000000000001421, -4.330127018922194537, 2.499999999999995559 ) ) ;
#56248 = CARTESIAN_POINT ( 'NONE',  ( 14.51250000122903394, -4.330127018922190985, -2.500000000000001332 ) ) ;
#56249 = CARTESIAN_POINT ( 'NONE',  ( 3.021917804904423743, -3.983467431823952687, -3.409840147052992432 ) ) ;
#56250 = CARTESIAN_POINT ( 'NONE',  ( 3.797099728130578278, -3.253013707837530522, 4.112539957277816072 ) ) ;
#56251 = ORIENTED_EDGE ( 'NONE', *, *, #68367, .F. ) ;
#56252 = CARTESIAN_POINT ( 'NONE',  ( 12.03749999999999964, -2.886751345948129988, 4.999999999999997335 ) ) ;
#56253 = CARTESIAN_POINT ( 'NONE',  ( 27.62812500061451360, -4.541064518000419881, 2.621784821874995952 ) ) ;
#56254 = CARTESIAN_POINT ( 'NONE',  ( 16.27499999999999858, 6.123233995736764310E-16, -4.999999999999998224 ) ) ;
#56255 = ADVANCED_FACE ( 'NONE', ( #22496 ), #45046, .F. ) ;
#56256 = CARTESIAN_POINT ( 'NONE',  ( 11.06250000122903288, 4.330127018922192761, -2.499999999999997780 ) ) ;
#56257 = CARTESIAN_POINT ( 'NONE',  ( 10.15312500061451750, -4.541064518000417216, -2.621784821875001281 ) ) ;
#56258 = CARTESIAN_POINT ( 'NONE',  ( 7.800000000000001599, 4.330127018922192761, -2.499999999999997780 ) ) ;
#56259 = CYLINDRICAL_SURFACE ( 'NONE', #53753, 4.999999999999998224 ) ;
#56260 = CARTESIAN_POINT ( 'NONE',  ( -3.000416591977282496E-16, 15.24687500061451928, -34.90005215228797653 ) ) ;
#56261 = CARTESIAN_POINT ( 'NONE',  ( 27.07500000122903216, -5.773502691896255534, -1.060575238724906372E-15 ) ) ;
#56262 = CARTESIAN_POINT ( 'NONE',  ( 3.756430356250000102, 14.89062499938548356, 30.00000000000000000 ) ) ;
#56263 = CARTESIAN_POINT ( 'NONE',  ( 8.400000000000000355, 0.000000000000000000, 4.999999999999998224 ) ) ;
#56264 = CARTESIAN_POINT ( 'NONE',  ( -3.999999999999999112, 13.25000000000000178, -30.00000000000000000 ) ) ;
#56265 = ORIENTED_EDGE ( 'NONE', *, *, #7253, .F. ) ;
#56266 = CARTESIAN_POINT ( 'NONE',  ( 23.91562500061451502, 3.027376345333611329, 5.243569643749999010 ) ) ;
#56267 = CARTESIAN_POINT ( 'NONE',  ( 28.71562500061451573, 3.027376345333613106, -5.243569643749998122 ) ) ;
#56268 = VECTOR ( 'NONE', #29847, 1000.000000000000000 ) ;
#56269 = CARTESIAN_POINT ( 'NONE',  ( 28.73437500061451644, 6.421520780324663323E-16, -5.243569643749999010 ) ) ;
#56270 = CARTESIAN_POINT ( 'NONE',  ( 19.54687500061451644, -3.027376345333614438, 5.243569643749998122 ) ) ;
#56271 = EDGE_CURVE ( 'NONE', #4004, #68252, #58282, .T. ) ;
#56272 = CARTESIAN_POINT ( 'NONE',  ( 16.45312500061451289, -4.541064518000417216, -2.621784821875001281 ) ) ;
#56273 = CARTESIAN_POINT ( 'NONE',  ( 2.121784821875001281, 11.85312500061459673, -26.32496088578401938 ) ) ;
#56274 = CARTESIAN_POINT ( 'NONE',  ( 7.715625000614515727, 3.027376345333611329, 5.243569643749999010 ) ) ;
#56275 = CARTESIAN_POINT ( 'NONE',  ( 28.83750000122903145, -4.330127018922194537, 2.499999999999995559 ) ) ;
#56276 = CARTESIAN_POINT ( 'NONE',  ( 24.64687500061451431, -2.746126346562641984, -4.756430356249999214 ) ) ;
#56277 = CARTESIAN_POINT ( 'NONE',  ( 18.25312500061451715, -4.541064518000417216, -2.621784821875001281 ) ) ;
#56278 = DIRECTION ( 'NONE',  ( -1.000000000000000000, -0.000000000000000000, -0.000000000000000000 ) ) ;
#56279 = CARTESIAN_POINT ( 'NONE',  ( 1.878215178124997609, 18.41562499938548214, 33.25316411605952993 ) ) ;
#56280 = CARTESIAN_POINT ( 'NONE',  ( 13.20937500061451786, 0.000000000000000000, 5.243569643749999010 ) ) ;
#56281 = CARTESIAN_POINT ( 'NONE',  ( 11.22187500061451892, 3.027376345333613106, -5.243569643749998122 ) ) ;
#56282 = CARTESIAN_POINT ( 'NONE',  ( 21.38437500061451502, -4.541064518000419881, 2.621784821874995952 ) ) ;
#56283 = ORIENTED_EDGE ( 'NONE', *, *, #66773, .F. ) ;
#56284 = CARTESIAN_POINT ( 'NONE',  ( 3.178125000614515638, 4.541064518000418104, 2.621784821874999949 ) ) ;
#56285 = CARTESIAN_POINT ( 'NONE',  ( 25.56562500061452070, 3.027376345333613106, -5.243569643749998122 ) ) ;
#56286 = CARTESIAN_POINT ( 'NONE',  ( 27.21562500061451928, -6.054752690667223547, -1.112240025338166033E-15 ) ) ;
#56287 = CARTESIAN_POINT ( 'NONE',  ( -1.999999999999997113, 16.47500000000000142, 33.46410161513775705 ) ) ;
#56288 = CARTESIAN_POINT ( 'NONE',  ( 4.696875000614518569, -3.027376345333614438, 5.243569643749998122 ) ) ;
#56289 = CARTESIAN_POINT ( 'NONE',  ( 13.05000000122903536, -2.886751345948129988, 4.999999999999997335 ) ) ;
#56290 = CARTESIAN_POINT ( 'NONE',  ( 6.000000001229033764, -2.886751345948125991, -5.000000000000000000 ) ) ;
#56291 = CARTESIAN_POINT ( 'NONE',  ( 28.61250000122903359, 4.330127018922192761, -2.499999999999997780 ) ) ;
#56292 = CARTESIAN_POINT ( 'NONE',  ( 3.999999999999998668, 19.15624999877096357, 32.30940107675850470 ) ) ;
#56293 = CARTESIAN_POINT ( 'NONE',  ( 16.63125000122903074, -4.330127018922194537, 2.499999999999995559 ) ) ;
#56294 = CARTESIAN_POINT ( 'NONE',  ( 12.87187500061451750, -6.054752690667223547, -1.112240025338166033E-15 ) ) ;
#56295 = CARTESIAN_POINT ( 'NONE',  ( 29.56875000122903074, 2.886751345948126879, 4.999999999999998224 ) ) ;
#56296 = CARTESIAN_POINT ( 'NONE',  ( 18.89062500061451644, 6.054752690667223547, 3.707466751127219781E-16 ) ) ;
#56297 = CARTESIAN_POINT ( 'NONE',  ( 13.88437500061451679, 6.421520780324663323E-16, -5.243569643749999010 ) ) ;
#56298 = CARTESIAN_POINT ( 'NONE',  ( 3.890625000614517326, -3.027376345333610441, -5.243569643749999898 ) ) ;
#56299 = CARTESIAN_POINT ( 'NONE',  ( 22.88437500061451857, 6.421520780324663323E-16, -5.243569643749999010 ) ) ;
#56300 = CARTESIAN_POINT ( 'NONE',  ( 9.609375000614518214, 0.000000000000000000, 5.243569643749999010 ) ) ;
#56301 = CARTESIAN_POINT ( 'NONE',  ( 5.690625000614516260, -3.027376345333610441, -5.243569643749999898 ) ) ;
#56302 = CARTESIAN_POINT ( 'NONE',  ( 10.68749999999999467, -2.886751345948019409, 5.000000000000189182 ) ) ;
#56303 = CARTESIAN_POINT ( 'NONE',  ( 5.625000001229036428, 2.886751345948129099, -4.999999999999998224 ) ) ;
#56304 = CARTESIAN_POINT ( 'NONE',  ( 21.25312500061451715, 0.000000000000000000, 5.243569643749999010 ) ) ;
#56305 = CARTESIAN_POINT ( 'NONE',  ( 7.387500001229032165, 6.123233995736764310E-16, -4.999999999999998224 ) ) ;
#56306 = CARTESIAN_POINT ( 'NONE',  ( 16.30312500061451786, 0.000000000000000000, 5.243569643749999010 ) ) ;
#56307 = CARTESIAN_POINT ( 'NONE',  ( 12.66562500061451502, 3.027376345333611329, 5.243569643749999010 ) ) ;
#56308 = CARTESIAN_POINT ( 'NONE',  ( 25.39687500061451431, -2.746126346562646425, 4.756430356249996549 ) ) ;
#56309 = CARTESIAN_POINT ( 'NONE',  ( 15.07499999999999929, 4.330127018922191873, 2.499999999999999556 ) ) ;
#56310 = CARTESIAN_POINT ( 'NONE',  ( 9.112500001229033586, -4.330127018922190985, -2.500000000000001332 ) ) ;
#56311 = CARTESIAN_POINT ( 'NONE',  ( 5.278125000614516615, 6.421520780324663323E-16, -5.243569643749999010 ) ) ;
#56312 = CARTESIAN_POINT ( 'NONE',  ( 20.66250000122903074, 0.000000000000000000, 4.999999999999998224 ) ) ;
#56313 = CARTESIAN_POINT ( 'NONE',  ( 27.44999999999999929, -4.330127018922190985, -2.500000000000001332 ) ) ;
#56314 = CARTESIAN_POINT ( 'NONE',  ( 9.001249775931846008E-16, 11.42187500061451999, -25.09994784771203058 ) ) ;
#56315 = DIRECTION ( 'NONE',  ( -1.000000000000000000, -0.000000000000000000, -0.000000000000000000 ) ) ;
#56316 = CYLINDRICAL_SURFACE ( 'NONE', #40672, 3.999999999999996447 ) ;
#56317 = VECTOR ( 'NONE', #16733, 1000.000000000000000 ) ;
#56318 = CARTESIAN_POINT ( 'NONE',  ( 28.31250000122903288, 0.000000000000000000, 4.999999999999998224 ) ) ;
#56319 = CARTESIAN_POINT ( 'NONE',  ( 21.30937500061451573, 0.000000000000000000, 5.243569643749999010 ) ) ;
#56320 = CARTESIAN_POINT ( 'NONE',  ( 12.37500000000000000, 4.330127018922191873, 2.499999999999999556 ) ) ;
#56321 = CARTESIAN_POINT ( 'NONE',  ( 17.46562500061451217, 3.027376345333613106, -5.243569643749998122 ) ) ;
#56322 = CARTESIAN_POINT ( 'NONE',  ( 12.61875000122903323, -5.773502691896255534, -1.060575238724906372E-15 ) ) ;
#56323 = CARTESIAN_POINT ( 'NONE',  ( -4.000000000000000888, 20.80624999877097281, 32.30940107675850470 ) ) ;
#56324 = DIRECTION ( 'NONE',  ( 0.000000000000000000, 0.000000000000000000, -1.000000000000000000 ) ) ;
#56325 = CARTESIAN_POINT ( 'NONE',  ( 29.37187500061451928, 3.027376345333611329, 5.243569643749999010 ) ) ;
#56326 = CARTESIAN_POINT ( 'NONE',  ( 20.70937500061451786, 2.746126346562643317, 4.756430356249998326 ) ) ;
#56327 = CARTESIAN_POINT ( 'NONE',  ( 12.85312500061451502, -4.541064518000417216, -2.621784821875001281 ) ) ;
#56328 = CARTESIAN_POINT ( 'NONE',  ( 11.48437500061451644, -4.541064518000419881, 2.621784821874995952 ) ) ;
#56329 = VERTEX_POINT ( 'NONE', #72753 ) ;
#56330 = CARTESIAN_POINT ( 'NONE',  ( 1.626862140677534273E-15, 14.26250000000000107, -26.00000000000000355 ) ) ;
#56331 = CARTESIAN_POINT ( 'NONE',  ( 21.92812500061451431, 6.421520780324663323E-16, -5.243569643749999010 ) ) ;
#56332 = CARTESIAN_POINT ( 'NONE',  ( -5.810221930991193690E-16, 13.25000000122903465, -34.00000000000000000 ) ) ;
#56333 = EDGE_CURVE ( 'NONE', #27416, #18316, #58155, .T. ) ;
#56334 = CARTESIAN_POINT ( 'NONE',  ( 11.88749999999999751, 5.773502691896255534, 3.535250795749688894E-16 ) ) ;
#56335 = CARTESIAN_POINT ( 'NONE',  ( 22.87500000122903288, 2.886751345948126879, 4.999999999999999112 ) ) ;
#56336 = CARTESIAN_POINT ( 'NONE',  ( 16.11562500061451786, 3.027376345333613106, -5.243569643749998122 ) ) ;
#56337 = CARTESIAN_POINT ( 'NONE',  ( 12.53437500061451537, 5.492252693125287522, 3.363034840372157021E-16 ) ) ;
#56338 = EDGE_LOOP ( 'NONE', ( #6736, #51800, #25986, #27054 ) ) ;
#56339 = CARTESIAN_POINT ( 'NONE',  ( 20.62499999999999645, -4.330127018922194537, 2.499999999999995559 ) ) ;
#56340 = ADVANCED_FACE ( 'NONE', ( #56127 ), #73114, .T. ) ;
#56341 = CARTESIAN_POINT ( 'NONE',  ( 24.48749999999999716, 5.773502691896255534, 3.535250795749688894E-16 ) ) ;
#56342 = CARTESIAN_POINT ( 'NONE',  ( 21.45937500061451786, -4.541064518000417216, -2.621784821875001281 ) ) ;
#56343 = CARTESIAN_POINT ( 'NONE',  ( 25.49062500061451786, -3.027376345333610441, -5.243569643749999898 ) ) ;
#56344 = ORIENTED_EDGE ( 'NONE', *, *, #23135, .T. ) ;
#56345 = CARTESIAN_POINT ( 'NONE',  ( 45.00000000000000000, 0.000000000000000000, 4.999999999999998224 ) ) ;
#56346 = CARTESIAN_POINT ( 'NONE',  ( 8.878125000614515372, 6.421520780324663323E-16, -5.243569643749999010 ) ) ;
#56347 = CARTESIAN_POINT ( 'NONE',  ( 45.00000000000000000, 0.000000000000000000, 4.999999999999998224 ) ) ;
#56348 = CARTESIAN_POINT ( 'NONE',  ( 15.29999999999999893, -4.330127018922190985, -2.500000000000001332 ) ) ;
#56349 = CARTESIAN_POINT ( 'NONE',  ( -2.121784821874999949, 19.72812500061451857, 26.32496088578401938 ) ) ;
#56350 = CARTESIAN_POINT ( 'NONE',  ( 4.396875000614516971, -3.027376345333610441, -5.243569643749999898 ) ) ;
#56351 = CARTESIAN_POINT ( 'NONE',  ( 28.32187500061451502, 3.027376345333613106, -5.243569643749998122 ) ) ;
#56352 = ORIENTED_EDGE ( 'NONE', *, *, #62588, .T. ) ;
#56353 = CARTESIAN_POINT ( 'NONE',  ( 23.27812500061451573, 6.421520780324663323E-16, -5.243569643749999010 ) ) ;
#56354 = CARTESIAN_POINT ( 'NONE',  ( 25.09687500061451715, -3.027376345333610441, -5.243569643749999898 ) ) ;
#56355 = CARTESIAN_POINT ( 'NONE',  ( 4.243569643749999010, 19.61562500061459602, -32.45002607614398471 ) ) ;
#56356 = CARTESIAN_POINT ( 'NONE',  ( 12.15000000000000036, -4.330127018922190985, -2.500000000000001332 ) ) ;
#56357 = CARTESIAN_POINT ( 'NONE',  ( 8.503125000614515372, 4.541064518000418104, -2.621784821874998173 ) ) ;
#56358 = DIRECTION ( 'NONE',  ( -0.000000000000000000, -1.000000000000000000, -0.000000000000000000 ) ) ;
#56359 = CARTESIAN_POINT ( 'NONE',  ( 17.02499999999999858, -4.330127018922194537, 2.499999999999995559 ) ) ;
#56360 = CARTESIAN_POINT ( 'NONE',  ( 25.75312500061451715, 0.000000000000000000, 5.243569643749999010 ) ) ;
#56361 = CARTESIAN_POINT ( 'NONE',  ( 29.55937500061451217, 2.746126346562645981, -4.756430356249997438 ) ) ;
#56362 = CARTESIAN_POINT ( 'NONE',  ( 13.88437500061451679, 5.824947211148865298E-16, -4.756430356249998326 ) ) ;
#56363 = CARTESIAN_POINT ( 'NONE',  ( 3.028125000614518392, 6.421520780324663323E-16, -5.243569643749999010 ) ) ;
#56364 = CARTESIAN_POINT ( 'NONE',  ( 19.02187500061451786, 3.027376345333611329, 5.243569643749999010 ) ) ;
#56365 = CARTESIAN_POINT ( 'NONE',  ( -2.121784821874999949, 14.38437500061451679, 26.32496088578401938 ) ) ;
#56366 = CARTESIAN_POINT ( 'NONE',  ( 21.79687500061451644, -3.027376345333614438, 5.243569643749998122 ) ) ;
#56367 = CARTESIAN_POINT ( 'NONE',  ( 3.075000000000001510, -4.330127018922194537, 2.499999999999995559 ) ) ;
#56368 = CARTESIAN_POINT ( 'NONE',  ( 9.001249775931846008E-16, 19.07187500061451857, 34.90005215228797653 ) ) ;
#56369 = CARTESIAN_POINT ( 'NONE',  ( 9.178125000614517859, -4.541064518000419881, 2.621784821874995952 ) ) ;
#56370 = CARTESIAN_POINT ( 'NONE',  ( 45.00000000000000000, -5.218601775200152559, -7.332543590861073213 ) ) ;
#56371 = CARTESIAN_POINT ( 'NONE',  ( 7.246875000614518392, 6.054752690667223547, 3.707466751127219781E-16 ) ) ;
#56372 = FACE_OUTER_BOUND ( 'NONE', #46274, .T. ) ;
#56373 = CARTESIAN_POINT ( 'NONE',  ( 6.515625000614516438, -6.054752690667223547, -1.112240025338166033E-15 ) ) ;
#56374 = CARTESIAN_POINT ( 'NONE',  ( 11.52187500061451608, -6.054752690667223547, -1.112240025338166033E-15 ) ) ;
#56375 = CARTESIAN_POINT ( 'NONE',  ( 18.18750000122903288, 6.123233995736764310E-16, -4.999999999999998224 ) ) ;
#56376 = CARTESIAN_POINT ( 'NONE',  ( 9.084375000614517859, 4.541064518000418104, 2.621784821874999949 ) ) ;
#56377 = CARTESIAN_POINT ( 'NONE',  ( 8.915625000614515017, 3.027376345333613106, -5.243569643749998122 ) ) ;
#56378 = CARTESIAN_POINT ( 'NONE',  ( 5.240625000614517859, -3.027376345333610441, -5.243569643749999898 ) ) ;
#56379 = CARTESIAN_POINT ( 'NONE',  ( 26.23125000122903216, 6.123233995736764310E-16, -4.999999999999998224 ) ) ;
#56380 = CARTESIAN_POINT ( 'NONE',  ( 18.04687500061451999, 6.054752690667223547, 3.707466751127219781E-16 ) ) ;
#56381 = CARTESIAN_POINT ( 'NONE',  ( 26.99062500061451431, 6.054752690667223547, 3.707466751127219781E-16 ) ) ;
#56382 = CARTESIAN_POINT ( 'NONE',  ( 13.26562500061451644, -6.054752690667223547, -1.112240025338166033E-15 ) ) ;
#56383 = EDGE_CURVE ( 'NONE', #64264, #15264, #50631, .T. ) ;
#56384 = AXIS2_PLACEMENT_3D ( 'NONE', #57870, #64879, #46808 ) ;
#56385 = CARTESIAN_POINT ( 'NONE',  ( 29.29687500061450933, 6.054752690667223547, 3.707466751127219781E-16 ) ) ;
#56386 = CARTESIAN_POINT ( 'NONE',  ( 4.243569643749999010, 10.67187500061451644, -32.45002607614398471 ) ) ;
#56387 =( BOUNDED_CURVE ( )  B_SPLINE_CURVE ( 2, ( #32872, #70572, #26607, #15500, #49145, #14777, #4448 ),
 .UNSPECIFIED., .F., .F. ) 
 B_SPLINE_CURVE_WITH_KNOTS ( ( 3, 2, 2, 3 ),
 ( 0.5800000000000000711, 0.5833333333333334814, 0.5866666666666666696, 0.5899999999999999689 ),
 .UNSPECIFIED. ) 
 CURVE ( )  GEOMETRIC_REPRESENTATION_ITEM ( )  RATIONAL_B_SPLINE_CURVE ( ( 0.9999999999999955591, 0.8660254037844431485, 1.000000000000000000, 0.8660254037844387076, 1.000000000000000000, 0.8660254037844387076, 1.000000000000000000 ) ) 
 REPRESENTATION_ITEM ( '' )  );
#56388 = CARTESIAN_POINT ( 'NONE',  ( 12.71250000122903145, -4.330127018922190985, -2.500000000000001332 ) ) ;
#56389 = CARTESIAN_POINT ( 'NONE',  ( 27.02812500061451573, 4.541064518000418104, 2.621784821874999949 ) ) ;
#56390 = CARTESIAN_POINT ( 'NONE',  ( 4.243569643749999898, 15.04062500061451679, -27.54997392385601529 ) ) ;
#56391 = CARTESIAN_POINT ( 'NONE',  ( 16.35000000122903430, -2.886751345948125991, -5.000000000000000000 ) ) ;
#56392 = CARTESIAN_POINT ( 'NONE',  ( 12.22499999999999964, 6.123233995736764310E-16, -4.999999999999998224 ) ) ;
#56393 = CARTESIAN_POINT ( 'NONE',  ( 21.74062500061451431, -3.027376345333614438, 5.243569643749998122 ) ) ;
#56394 = CARTESIAN_POINT ( 'NONE',  ( 8.896875000614517859, -3.027376345333610441, -5.243569643749999898 ) ) ;
#56395 = CARTESIAN_POINT ( 'NONE',  ( 8.175000001229031810, -5.773502691896255534, -1.060575238724906372E-15 ) ) ;
#56396 = CARTESIAN_POINT ( 'NONE',  ( 15.86250000122903181, -4.330127018922190985, -2.500000000000001332 ) ) ;
#56397 = CARTESIAN_POINT ( 'NONE',  ( 12.47812500061451502, 6.421520780324663323E-16, -5.243569643749999010 ) ) ;
#56398 = CARTESIAN_POINT ( 'NONE',  ( 15.32812500061451644, 4.541064518000418104, 2.621784821874999949 ) ) ;
#56399 = CARTESIAN_POINT ( 'NONE',  ( 27.48750000122903359, -4.330127018922194537, 2.499999999999995559 ) ) ;
#56400 = CARTESIAN_POINT ( 'NONE',  ( 22.80000000000000071, 0.000000000000000000, 4.999999999999998224 ) ) ;
#56401 = CARTESIAN_POINT ( 'NONE',  ( 22.69687500061451857, -3.027376345333614438, 5.243569643749998122 ) ) ;
#56402 = DIRECTION ( 'NONE',  ( 0.000000000000000000, 0.7071067811865388020, -0.7071067811865562325 ) ) ;
#56403 = CARTESIAN_POINT ( 'NONE',  ( 11.32500000122903394, -5.773502691896255534, -1.060575238724906372E-15 ) ) ;
#56404 = CARTESIAN_POINT ( 'NONE',  ( 28.43437500061451573, 4.541064518000418104, 2.621784821874999949 ) ) ;
#56405 = CARTESIAN_POINT ( 'NONE',  ( 4.959375000614516971, 4.541064518000418104, -2.621784821874998173 ) ) ;
#56406 = CARTESIAN_POINT ( 'NONE',  ( 23.39062500061451289, 6.054752690667223547, 3.707466751127219781E-16 ) ) ;
#56407 = CARTESIAN_POINT ( 'NONE',  ( -3.756430356250000990, 15.71562499938548108, 32.16877607737301048 ) ) ;
#56408 = CARTESIAN_POINT ( 'NONE',  ( 7.012500000000001954, 2.886751345948126879, 4.999999999999998224 ) ) ;
#56409 = CARTESIAN_POINT ( 'NONE',  ( 9.421875000614519990, 3.027376345333613106, -5.243569643749998122 ) ) ;
#56410 = CARTESIAN_POINT ( 'NONE',  ( -5.810221930991193690E-16, 12.68750000000000000, 26.00000000000000355 ) ) ;
#56411 = CARTESIAN_POINT ( 'NONE',  ( 3.834375000614519635, -4.541064518000419881, 2.621784821874995952 ) ) ;
#56412 = CARTESIAN_POINT ( 'NONE',  ( 7.096875000614517148, -3.027376345333610441, -5.243569643749999898 ) ) ;
#56413 = DIRECTION ( 'NONE',  ( 1.000000000000000000, 0.000000000000000000, 0.000000000000000000 ) ) ;
#56414 = CARTESIAN_POINT ( 'NONE',  ( 25.99687500061451928, -3.027376345333610441, -5.243569643749999898 ) ) ;
#56415 = CARTESIAN_POINT ( 'NONE',  ( 27.73125000122902861, 4.330127018922191873, 2.499999999999999556 ) ) ;
#56416 = CARTESIAN_POINT ( 'NONE',  ( 19.27500000000000213, -4.330127018922194537, 2.499999999999995559 ) ) ;
#56417 = ORIENTED_EDGE ( 'NONE', *, *, #43935, .F. ) ;
#56418 = CARTESIAN_POINT ( 'NONE',  ( 28.19999999999999929, 0.000000000000000000, 4.999999999999998224 ) ) ;
#56419 = ADVANCED_FACE ( 'NONE', ( #4439 ), #21402, .F. ) ;
#56420 =( BOUNDED_CURVE ( )  B_SPLINE_CURVE ( 2, ( #48705, #54606, #64587, #2900, #20607, #31710, #70130, #2537, #54245 ),
 .UNSPECIFIED., .F., .F. ) 
 B_SPLINE_CURVE_WITH_KNOTS ( ( 3, 2, 2, 2, 3 ),
 ( 0.8369565217391304879, 0.8405797101449274944, 0.8478260869565217295, 0.8550724637681159646, 0.8586956521739130821 ),
 .UNSPECIFIED. ) 
 CURVE ( )  GEOMETRIC_REPRESENTATION_ITEM ( )  RATIONAL_B_SPLINE_CURVE ( ( 0.9330127018922192983, 0.9330127018922202975, 1.000000000000000000, 0.8660254037844387076, 1.000000000000000000, 0.8660254037844387076, 1.000000000000000000, 0.9330127018922194093, 0.9330127018922194093 ) ) 
 REPRESENTATION_ITEM ( '' )  );
#56421 = CARTESIAN_POINT ( 'NONE',  ( 29.78437500061451715, 4.541064518000418104, 2.621784821874999949 ) ) ;
#56422 = ORIENTED_EDGE ( 'NONE', *, *, #60445, .F. ) ;
#56423 = CARTESIAN_POINT ( 'NONE',  ( 16.19062500061451715, 6.054752690667223547, 3.707466751127219781E-16 ) ) ;
#56424 = CARTESIAN_POINT ( 'NONE',  ( 9.103125000614515017, 0.000000000000000000, 5.243569643749999010 ) ) ;
#56425 = CARTESIAN_POINT ( 'NONE',  ( 18.34687500061451360, 4.119189519843966529, -2.378215178124998275 ) ) ;
#56426 = CARTESIAN_POINT ( 'NONE',  ( 3.496875000614518836, -3.027376345333610441, -5.243569643749999898 ) ) ;
#56427 = CARTESIAN_POINT ( 'NONE',  ( 17.77500000122903145, 2.886751345948129099, -4.999999999999998224 ) ) ;
#56428 = CARTESIAN_POINT ( 'NONE',  ( 22.57499999999999929, 6.123233995736764310E-16, -4.999999999999998224 ) ) ;
#56429 = CARTESIAN_POINT ( 'NONE',  ( 6.721875000614518925, 3.027376345333613106, -5.243569643749998122 ) ) ;
#56430 = CARTESIAN_POINT ( 'NONE',  ( 12.12187500061451573, 3.027376345333613106, -5.243569643749998122 ) ) ;
#56431 = CARTESIAN_POINT ( 'NONE',  ( 21.57187500061451502, 3.027376345333613106, -5.243569643749998122 ) ) ;
#56432 = CARTESIAN_POINT ( 'NONE',  ( 2.000000000000001332, 15.76250000122903216, -26.53589838486224650 ) ) ;
#56433 = ORIENTED_EDGE ( 'NONE', *, *, #44720, .T. ) ;
#56434 = CARTESIAN_POINT ( 'NONE',  ( 4.096875000614518925, 6.054752690667223547, 3.707466751127219781E-16 ) ) ;
#56435 = CARTESIAN_POINT ( 'NONE',  ( 5.896875000614518747, 6.054752690667223547, 3.707466751127219781E-16 ) ) ;
#56436 = CARTESIAN_POINT ( 'NONE',  ( 18.33749999999999858, -2.886751345948129988, 4.999999999999997335 ) ) ;
#56437 = CARTESIAN_POINT ( 'NONE',  ( 17.09062500061451573, 6.054752690667223547, 3.707466751127219781E-16 ) ) ;
#56438 = CARTESIAN_POINT ( 'NONE',  ( -3.999999999999999556, 18.53749999999999787, 27.69059892324149175 ) ) ;
#56439 = DIRECTION ( 'NONE',  ( 0.000000000000000000, 0.000000000000000000, 1.000000000000000000 ) ) ;
#56440 = CARTESIAN_POINT ( 'NONE',  ( 23.07187500061451857, 2.746126346562643317, 4.756430356249998326 ) ) ;
#56441 = CARTESIAN_POINT ( 'NONE',  ( 10.41562500061451679, 3.027376345333611329, 5.243569643749999010 ) ) ;
#56442 = CARTESIAN_POINT ( 'NONE',  ( 26.37187500061451217, -6.054752690667223547, -1.112240025338166033E-15 ) ) ;
#56443 = DIRECTION ( 'NONE',  ( 0.000000000000000000, 0.000000000000000000, -1.000000000000000000 ) ) ;
#56444 = CARTESIAN_POINT ( 'NONE',  ( 28.13437500061451502, -4.541064518000419881, 2.621784821874995952 ) ) ;
#56445 = CARTESIAN_POINT ( 'NONE',  ( 10.42500000000000071, 6.123233995736764310E-16, -4.999999999999998224 ) ) ;
#56446 = CARTESIAN_POINT ( 'NONE',  ( 8.484601909799253346E-16, 16.62500000122903288, 34.61880215351700230 ) ) ;
#56447 = CARTESIAN_POINT ( 'NONE',  ( 9.337500001229033231, 4.330127018922191873, 2.499999999999999556 ) ) ;
#56448 = CARTESIAN_POINT ( 'NONE',  ( 18.83437500061451431, 6.421520780324663323E-16, -5.243569643749999010 ) ) ;
#56449 = CARTESIAN_POINT ( 'NONE',  ( 13.35937500061451821, -4.541064518000417216, -2.621784821875001281 ) ) ;
#56450 = CARTESIAN_POINT ( 'NONE',  ( 4.000000000000000000, 13.83124999877096606, 27.69059892324149885 ) ) ;
#56451 = ORIENTED_EDGE ( 'NONE', *, *, #61270, .T. ) ;
#56452 = CARTESIAN_POINT ( 'NONE',  ( 13.64062500061451644, -3.027376345333614438, 5.243569643749998122 ) ) ;
#56453 = CARTESIAN_POINT ( 'NONE',  ( 27.30000000122903359, 5.773502691896255534, 3.535250795749688894E-16 ) ) ;
#56454 = CARTESIAN_POINT ( 'NONE',  ( 15.90937500061451892, 0.000000000000000000, 5.243569643749999010 ) ) ;
#56455 = CARTESIAN_POINT ( 'NONE',  ( 4.520916466877470619, 8.924797207603102578, -33.96362936841865121 ) ) ;
#56456 = CARTESIAN_POINT ( 'NONE',  ( 18.17812500061451786, -4.541064518000419881, 2.621784821874995952 ) ) ;
#56457 = LINE ( 'NONE', #5847, #53948 ) ;
#56458 = CARTESIAN_POINT ( 'NONE',  ( 27.04687500061451644, 6.054752690667223547, 3.707466751127219781E-16 ) ) ;
#56459 = CARTESIAN_POINT ( 'NONE',  ( 9.001249775931846008E-16, 10.91562500061451857, 34.90005215228797653 ) ) ;
#56460 = CARTESIAN_POINT ( 'NONE',  ( 15.30937500061451750, 4.541064518000418104, -2.621784821874998173 ) ) ;
#56461 = CARTESIAN_POINT ( 'NONE',  ( 13.20000000122903394, -2.886751345948125991, -5.000000000000000000 ) ) ;
#56462 = CARTESIAN_POINT ( 'NONE',  ( 7.921875000614517326, -5.492252693125287522, -1.008910452111647106E-15 ) ) ;
#56463 = CARTESIAN_POINT ( 'NONE',  ( -4.243569643749998122, 19.44687500061451857, -27.54997392385601174 ) ) ;
#56464 = CARTESIAN_POINT ( 'NONE',  ( 17.59687500061451715, 6.054752690667223547, 3.707466751127219781E-16 ) ) ;
#56465 = CARTESIAN_POINT ( 'NONE',  ( 19.53750000122903430, 6.123233995736764310E-16, -4.999999999999998224 ) ) ;
#56466 = CARTESIAN_POINT ( 'NONE',  ( 15.72187500061451892, 3.027376345333613106, -5.243569643749998122 ) ) ;
#56467 = CARTESIAN_POINT ( 'NONE',  ( 4.243569643749999898, 13.33437500061451786, 30.00000000000000000 ) ) ;
#56468 = CARTESIAN_POINT ( 'NONE',  ( 21.52500000122903145, 2.886751345948126879, 4.999999999999999112 ) ) ;
#56469 = CARTESIAN_POINT ( 'NONE',  ( 15.89062500061451289, -3.027376345333614438, 5.243569643749998122 ) ) ;
#56470 = VERTEX_POINT ( 'NONE', #23583 ) ;
#56471 = ORIENTED_EDGE ( 'NONE', *, *, #37141, .T. ) ;
#56472 = CARTESIAN_POINT ( 'NONE',  ( 21.56250000000000000, -5.773502691896255534, -1.060575238724906372E-15 ) ) ;
#56473 = CARTESIAN_POINT ( 'NONE',  ( 17.62500000000000000, 6.123233995736764310E-16, -4.999999999999998224 ) ) ;
#56474 = CARTESIAN_POINT ( 'NONE',  ( 4.190625000614518925, -3.027376345333614438, 5.243569643749998122 ) ) ;
#56475 = EDGE_CURVE ( 'NONE', #55166, #39465, #46128, .T. ) ;
#56476 = CARTESIAN_POINT ( 'NONE',  ( 15.93750000122903110, 6.123233995736764310E-16, -4.999999999999998224 ) ) ;
#56477 = CARTESIAN_POINT ( 'NONE',  ( 20.09062500061451573, -3.027376345333610441, -5.243569643749999898 ) ) ;
#56478 = CARTESIAN_POINT ( 'NONE',  ( 24.25312500061451715, 4.541064518000418104, -2.621784821874998173 ) ) ;
#56479 = CARTESIAN_POINT ( 'NONE',  ( 4.640625000614518214, -3.027376345333614438, 5.243569643749998122 ) ) ;
#56480 = CARTESIAN_POINT ( 'NONE',  ( 29.88749999999999929, 5.773502691896255534, 3.535250795749688894E-16 ) ) ;
#56481 = CARTESIAN_POINT ( 'NONE',  ( 1.999999999999998668, 11.86250000122903359, 26.53589838486224650 ) ) ;
#56482 = CARTESIAN_POINT ( 'NONE',  ( 9.609375000614518214, 0.000000000000000000, 4.756430356249998326 ) ) ;
#56483 = DIRECTION ( 'NONE',  ( 0.000000000000000000, 0.000000000000000000, 1.000000000000000000 ) ) ;
#56484 = CARTESIAN_POINT ( 'NONE',  ( 2.000000000000001332, 11.71250000122903501, -26.53589838486224650 ) ) ;
#56485 = CARTESIAN_POINT ( 'NONE',  ( -4.243569643749997233, 18.99687500061451928, -27.54997392385601174 ) ) ;
#56486 = CARTESIAN_POINT ( 'NONE',  ( 5.250000001229035540, 5.773502691896255534, 3.535250795749688894E-16 ) ) ;
#56487 = CARTESIAN_POINT ( 'NONE',  ( 8.550000000000002487, -4.330127018922190985, -2.500000000000001332 ) ) ;
#56488 = CARTESIAN_POINT ( 'NONE',  ( 3.487500001229035362, 4.330127018922191873, 2.499999999999999556 ) ) ;
#56489 = CARTESIAN_POINT ( 'NONE',  ( 12.49687500061451573, -3.027376345333610441, -5.243569643749999898 ) ) ;
#56490 = CARTESIAN_POINT ( 'NONE',  ( 24.52500000122903501, 2.886751345948146419, -4.999999999999968914 ) ) ;
#56491 = CARTESIAN_POINT ( 'NONE',  ( 3.834375000614519635, -4.541064518000419881, 2.621784821874995952 ) ) ;
#56492 = FACE_OUTER_BOUND ( 'NONE', #12342, .T. ) ;
#56493 = CARTESIAN_POINT ( 'NONE',  ( 24.31875000122903074, -5.773502691896255534, -1.060575238724906372E-15 ) ) ;
#56494 = CARTESIAN_POINT ( 'NONE',  ( 9.759375000614516793, -4.541064518000417216, -2.621784821875001281 ) ) ;
#56495 = CARTESIAN_POINT ( 'NONE',  ( 2.000000000000001332, 14.30000000000000071, 33.46410161513774995 ) ) ;
#56496 = CARTESIAN_POINT ( 'NONE',  ( -2.121784821874999949, 16.57812500061459815, 26.32496088578401938 ) ) ;
#56497 = CARTESIAN_POINT ( 'NONE',  ( 21.53437500061451715, 6.421520780324663323E-16, -5.243569643749999010 ) ) ;
#56498 = CARTESIAN_POINT ( 'NONE',  ( 0.000000000000000000, 27.50000000000000000, 30.00000000000000000 ) ) ;
#56499 = EDGE_CURVE ( 'NONE', #26952, #37978, #6609, .T. ) ;
#56500 = CARTESIAN_POINT ( 'NONE',  ( 29.51250000122903216, 4.330127018922192761, -2.499999999999997780 ) ) ;
#56501 = CARTESIAN_POINT ( 'NONE',  ( 18.12187500061451928, -4.119189519843968306, 2.378215178124996054 ) ) ;
#56502 = CARTESIAN_POINT ( 'NONE',  ( 22.11562500061451786, 3.027376345333611329, 5.243569643749999010 ) ) ;
#56503 = CARTESIAN_POINT ( 'NONE',  ( 15.14062500061451644, -3.027376345333610441, -5.243569643749999898 ) ) ;
#56504 = CARTESIAN_POINT ( 'NONE',  ( 25.58437500061451431, 5.492252693125287522, 3.363034840372157021E-16 ) ) ;
#56505 = CARTESIAN_POINT ( 'NONE',  ( 11.63437500061451857, 6.421520780324663323E-16, -5.243569643749999010 ) ) ;
#56506 = CARTESIAN_POINT ( 'NONE',  ( 27.86249999999999716, -5.773502691896255534, -1.060575238724906372E-15 ) ) ;
#56507 = CARTESIAN_POINT ( 'NONE',  ( 25.98750000122903003, 4.330127018922191873, 2.499999999999999556 ) ) ;
#56508 = CARTESIAN_POINT ( 'NONE',  ( 3.196875000614516793, 6.054752690667223547, 3.707466751127219781E-16 ) ) ;
#56509 = CARTESIAN_POINT ( 'NONE',  ( 14.25937500061451679, -4.541064518000417216, -2.621784821875001281 ) ) ;
#56510 = CARTESIAN_POINT ( 'NONE',  ( 28.84687500061452070, 6.054752690667223547, 3.707466751127219781E-16 ) ) ;
#56511 = CARTESIAN_POINT ( 'NONE',  ( 8.250000001229034652, -2.886751345948126435, -5.000000000000000000 ) ) ;
#56512 = CARTESIAN_POINT ( 'NONE',  ( 15.73125000122903216, -4.330127018922194537, 2.499999999999995559 ) ) ;
#56513 = CARTESIAN_POINT ( 'NONE',  ( 21.90937500061451715, -4.541064518000417216, -2.621784821875001281 ) ) ;
#56514 = CARTESIAN_POINT ( 'NONE',  ( 15.42187500061451821, 3.027376345333611329, 5.243569643749999010 ) ) ;
#56515 = CARTESIAN_POINT ( 'NONE',  ( 2.655984681222220721E-16, 15.11562499938548321, 25.66244784525396483 ) ) ;
#56516 = CARTESIAN_POINT ( 'NONE',  ( 26.47499999999999787, -4.330127018922194537, 2.499999999999995559 ) ) ;
#56517 = CARTESIAN_POINT ( 'NONE',  ( 3.862500001229035362, 4.330127018922192761, -2.499999999999997780 ) ) ;
#56518 = CARTESIAN_POINT ( 'NONE',  ( 28.80937500061451573, 4.119189519843966529, -2.378215178124998275 ) ) ;
#56519 = CARTESIAN_POINT ( 'NONE',  ( 16.49062500061451786, -3.027376345333610441, -5.243569643749999898 ) ) ;
#56520 = CARTESIAN_POINT ( 'NONE',  ( 6.299999999999999822, -4.330127018922190985, -2.500000000000001332 ) ) ;
#56521 = DIRECTION ( 'NONE',  ( -0.9848080501874550974, 0.000000000000000000, 0.1736464922939214839 ) ) ;
#56522 = CARTESIAN_POINT ( 'NONE',  ( 17.28750000000000142, 5.773502691896255534, 3.535250795749688894E-16 ) ) ;
#56523 = CARTESIAN_POINT ( 'NONE',  ( 2.121784821875001281, 13.65312500061451750, 33.67503911421598417 ) ) ;
#56524 = CARTESIAN_POINT ( 'NONE',  ( 24.69375000122903074, -2.886751345948130876, 4.999999999999996447 ) ) ;
#56525 = CARTESIAN_POINT ( 'NONE',  ( 19.83750000122903145, -4.330127018922194537, 2.499999999999995559 ) ) ;
#56526 = DIRECTION ( 'NONE',  ( -0.000000000000000000, -1.000000000000000000, -0.000000000000000000 ) ) ;
#56527 = CARTESIAN_POINT ( 'NONE',  ( 27.94687500061451502, 6.054752690667223547, 3.707466751127219781E-16 ) ) ;
#56528 = ORIENTED_EDGE ( 'NONE', *, *, #68511, .T. ) ;
#56529 = CARTESIAN_POINT ( 'NONE',  ( 22.64062500061451644, -3.027376345333614438, 5.243569643749998122 ) ) ;
#56530 = CARTESIAN_POINT ( 'NONE',  ( 21.68437500061451573, 4.541064518000418104, 2.621784821874999949 ) ) ;
#56531 = CARTESIAN_POINT ( 'NONE',  ( 5.625000000000001776, 4.330127018922191873, 2.499999999999999556 ) ) ;
#56532 = CARTESIAN_POINT ( 'NONE',  ( 8.953125000614518214, 4.541064518000418104, -2.621784821874998173 ) ) ;
#56533 = CARTESIAN_POINT ( 'NONE',  ( 24.06562500061451715, -6.054752690667223547, -1.112240025338166033E-15 ) ) ;
#56534 = CARTESIAN_POINT ( 'NONE',  ( 12.34687500061452070, -3.027376345333614438, 5.243569643749998122 ) ) ;
#56535 = CARTESIAN_POINT ( 'NONE',  ( 16.84687500061451715, -3.027376345333614438, 5.243569643749998122 ) ) ;
#56536 = CARTESIAN_POINT ( 'NONE',  ( 0.000000000000000000, 20.00000000000000000, -33.99999999999999289 ) ) ;
#56537 = CARTESIAN_POINT ( 'NONE',  ( 2.121784821874999061, 16.50312500061451715, 26.32496088578401583 ) ) ;
#56538 = CARTESIAN_POINT ( 'NONE',  ( 21.45000000122903216, 5.773502691896255534, 3.535250795749688894E-16 ) ) ;
#56539 = CARTESIAN_POINT ( 'NONE',  ( 13.69687500061451679, -2.746126346562646425, 4.756430356249996549 ) ) ;
#56540 = CARTESIAN_POINT ( 'NONE',  ( 11.91562500061451857, -6.054752690667223547, -1.112240025338166033E-15 ) ) ;
#56541 = CARTESIAN_POINT ( 'NONE',  ( 6.571875000614517681, -6.054752690667223547, -1.112240025338166033E-15 ) ) ;
#56542 = CARTESIAN_POINT ( 'NONE',  ( 5.371875000614516615, 3.027376345333613106, -5.243569643749998122 ) ) ;
#56543 = ORIENTED_EDGE ( 'NONE', *, *, #30819, .T. ) ;
#56544 = CARTESIAN_POINT ( 'NONE',  ( 25.50937500061451502, -4.541064518000417216, -2.621784821875001281 ) ) ;
#56545 = CARTESIAN_POINT ( 'NONE',  ( 16.26562500061451289, 3.027376345333611329, 5.243569643749999010 ) ) ;
#56546 = CARTESIAN_POINT ( 'NONE',  ( 27.67500000122903359, 2.886751345948129099, -4.999999999999998224 ) ) ;
#56547 = CARTESIAN_POINT ( 'NONE',  ( 28.52812500061451573, -4.541064518000419881, 2.621784821874995952 ) ) ;
#56548 = CARTESIAN_POINT ( 'NONE',  ( 22.47187500061451715, 3.027376345333613106, -5.243569643749998122 ) ) ;
#56549 = CARTESIAN_POINT ( 'NONE',  ( 16.64062500061451289, 6.054752690667223547, 3.707466751127219781E-16 ) ) ;
#56550 = CARTESIAN_POINT ( 'NONE',  ( -2.121784821874999949, 19.33437500061451786, 26.32496088578401938 ) ) ;
#56551 = CARTESIAN_POINT ( 'NONE',  ( 23.54062500061451146, -3.027376345333614438, 5.243569643749998122 ) ) ;
#56552 = CARTESIAN_POINT ( 'NONE',  ( 4.725000001229034297, 2.886751345948129099, -4.999999999999998224 ) ) ;
#56553 = ORIENTED_EDGE ( 'NONE', *, *, #7032, .F. ) ;
#56554 = CARTESIAN_POINT ( 'NONE',  ( 28.01249999999999574, 2.886751345948129099, -4.999999999999998224 ) ) ;
#56555 = CARTESIAN_POINT ( 'NONE',  ( -3.999999999999999112, 13.25000000000000178, -30.00000000000000000 ) ) ;
#56556 = CARTESIAN_POINT ( 'NONE',  ( 3.756430356249998770, 17.66562499938548214, 32.16877607737302469 ) ) ;
#56557 = CARTESIAN_POINT ( 'NONE',  ( 2.859375000614519546, 0.000000000000000000, 5.243569643749999010 ) ) ;
#56558 = CARTESIAN_POINT ( 'NONE',  ( 10.86562500061451431, 3.027376345333611329, 5.243569643749999010 ) ) ;
#56559 = CARTESIAN_POINT ( 'NONE',  ( 21.82500000122903572, 2.886751345948129099, -4.999999999999998224 ) ) ;
#56560 = CARTESIAN_POINT ( 'NONE',  ( 12.83437500061451786, -4.541064518000419881, 2.621784821874995952 ) ) ;
#56561 = CARTESIAN_POINT ( 'NONE',  ( 3.721875000614518036, 3.027376345333611329, 5.243569643749999010 ) ) ;
#56562 = CARTESIAN_POINT ( 'NONE',  ( 26.73749999999999716, 5.773502691896255534, 3.535250795749688894E-16 ) ) ;
#56563 = CARTESIAN_POINT ( 'NONE',  ( 14.70000000122903216, 5.773502691896255534, 3.535250795749688401E-16 ) ) ;
#56564 = CARTESIAN_POINT ( 'NONE',  ( 13.60312500061451679, 0.000000000000000000, 5.243569643749999010 ) ) ;
#56565 = ORIENTED_EDGE ( 'NONE', *, *, #55072, .T. ) ;
#56566 = CARTESIAN_POINT ( 'NONE',  ( 9.515625000614518214, 3.027376345333611329, 5.243569643749999010 ) ) ;
#56567 = CARTESIAN_POINT ( 'NONE',  ( 7.040625000614517681, -3.027376345333610441, -5.243569643749999898 ) ) ;
#56568 = CARTESIAN_POINT ( 'NONE',  ( 19.20937500061451786, -4.119189519843965641, -2.378215178125001383 ) ) ;
#56569 = CARTESIAN_POINT ( 'NONE',  ( 9.528763966825557376E-15, 17.07500000122903572, -26.00000000000000000 ) ) ;
#56570 = CARTESIAN_POINT ( 'NONE',  ( 15.86250000000000249, 2.886751345948129099, -4.999999999999998224 ) ) ;
#56571 =( BOUNDED_CURVE ( )  B_SPLINE_CURVE ( 2, ( #28566, #51820, #39664, #1223, #498, #23729, #10846, #44844, #62183 ),
 .UNSPECIFIED., .F., .F. ) 
 B_SPLINE_CURVE_WITH_KNOTS ( ( 3, 2, 2, 2, 3 ),
 ( 0.5138888888888889506, 0.5185185185185184897, 0.5277777777777777901, 0.5370370370370370905, 0.5416666666666667407 ),
 .UNSPECIFIED. ) 
 CURVE ( )  GEOMETRIC_REPRESENTATION_ITEM ( )  RATIONAL_B_SPLINE_CURVE ( ( 0.9330127018922192983, 0.9330127018922200755, 1.000000000000000000, 0.8660254037844387076, 1.000000000000000000, 0.8660254037844387076, 1.000000000000000000, 0.9330127018922185211, 0.9330127018922192983 ) ) 
 REPRESENTATION_ITEM ( '' )  );
#56572 = CARTESIAN_POINT ( 'NONE',  ( 16.02187500061451786, -6.054752690667223547, -1.112240025338166033E-15 ) ) ;
#56573 = CARTESIAN_POINT ( 'NONE',  ( 11.47500000122903252, 2.886751345948129099, -4.999999999999998224 ) ) ;
#56574 = EDGE_CURVE ( 'NONE', #16892, #45352, #22773, .T. ) ;
#56575 = CARTESIAN_POINT ( 'NONE',  ( 18.60937500061451644, 0.000000000000000000, 5.243569643749999010 ) ) ;
#56576 = CARTESIAN_POINT ( 'NONE',  ( 19.50000000000000000, 4.330127018922192761, -2.499999999999997780 ) ) ;
#56577 = CARTESIAN_POINT ( 'NONE',  ( 19.88437500061451857, 4.541064518000418104, 2.621784821874999949 ) ) ;
#56578 = CARTESIAN_POINT ( 'NONE',  ( 2.121784821874999061, 14.70312500061451644, -33.67503911421598417 ) ) ;
#56579 = CARTESIAN_POINT ( 'NONE',  ( 3.999999999999998668, 16.66250000000000142, 27.69059892324149530 ) ) ;
#56580 = CARTESIAN_POINT ( 'NONE',  ( 24.94687500061451502, -4.119189519843965641, -2.378215178125001383 ) ) ;
#56581 = CARTESIAN_POINT ( 'NONE',  ( 3.999999999999998668, 13.30624999877096570, 32.30940107675850470 ) ) ;
#56582 = CARTESIAN_POINT ( 'NONE',  ( 27.59062500061451573, -3.027376345333614438, 5.243569643749998122 ) ) ;
#56583 = CARTESIAN_POINT ( 'NONE',  ( 25.01249999999999929, 2.886751345948126879, 4.999999999999998224 ) ) ;
#56584 = CARTESIAN_POINT ( 'NONE',  ( 27.83437500061451786, 6.421520780324663323E-16, -5.243569643749999010 ) ) ;
#56585 = CARTESIAN_POINT ( 'NONE',  ( 25.05000000000000071, 0.000000000000000000, 4.999999999999998224 ) ) ;
#56586 = EDGE_CURVE ( 'NONE', #18379, #8722, #30332, .T. ) ;
#56587 = CARTESIAN_POINT ( 'NONE',  ( 8.240625000614516082, -3.027376345333614438, 5.243569643749998122 ) ) ;
#56588 = CARTESIAN_POINT ( 'NONE',  ( 24.08437500061451075, -2.746126346562642428, -4.756430356249999214 ) ) ;
#56589 = CARTESIAN_POINT ( 'NONE',  ( 17.97187500061451715, 3.027376345333613106, -5.243569643749998122 ) ) ;
#56590 = CARTESIAN_POINT ( 'NONE',  ( 11.89687500061451608, -4.119189519843965641, -2.378215178125001383 ) ) ;
#56591 = CARTESIAN_POINT ( 'NONE',  ( 6.103125000614515905, -4.541064518000417216, -2.621784821875001281 ) ) ;
#56592 = CARTESIAN_POINT ( 'NONE',  ( 9.721875000614517148, -6.054752690667223547, -1.112240025338166033E-15 ) ) ;
#56593 = ORIENTED_EDGE ( 'NONE', *, *, #5758, .T. ) ;
#56594 = CARTESIAN_POINT ( 'NONE',  ( 22.32187500061451502, -6.054752690667223547, -1.112240025338166033E-15 ) ) ;
#56595 = FACE_OUTER_BOUND ( 'NONE', #29788, .T. ) ;
#56596 = CARTESIAN_POINT ( 'NONE',  ( 28.49999999999999645, 4.330127018922192761, -2.499999999999997780 ) ) ;
#56597 = CARTESIAN_POINT ( 'NONE',  ( 3.187500000000002220, -2.886751345948125991, -5.000000000000000000 ) ) ;
#56598 = CARTESIAN_POINT ( 'NONE',  ( 15.00000000122903465, -2.886751345948125991, -5.000000000000000000 ) ) ;
#56599 = CARTESIAN_POINT ( 'NONE',  ( 30.00000000000000000, 6.123233995736764310E-16, -4.999999999999998224 ) ) ;
#56600 = CARTESIAN_POINT ( 'NONE',  ( 3.768252779319924972, -3.286398503110366409, 4.085920018314769919 ) ) ;
#56601 = ORIENTED_EDGE ( 'NONE', *, *, #71019, .F. ) ;
#56602 = CARTESIAN_POINT ( 'NONE',  ( 13.64999999999999858, 4.330127018922192761, -2.499999999999997780 ) ) ;
#56603 = CARTESIAN_POINT ( 'NONE',  ( 23.69062500061451004, -3.027376345333610441, -5.243569643749999898 ) ) ;
#56604 = CARTESIAN_POINT ( 'NONE',  ( 14.88750000000000107, -2.886751345948125991, -5.000000000000000000 ) ) ;
#56605 = CARTESIAN_POINT ( 'NONE',  ( 10.65000000122903323, 5.773502691896255534, 3.535250795749688894E-16 ) ) ;
#56606 = CARTESIAN_POINT ( 'NONE',  ( 7.903125000614515727, -4.541064518000417216, -2.621784821875001281 ) ) ;
#56607 = CARTESIAN_POINT ( 'NONE',  ( 9.037499999999999645, -2.886751345948125991, -5.000000000000000000 ) ) ;
#56608 = CARTESIAN_POINT ( 'NONE',  ( 19.31250000122903288, 0.000000000000000000, 4.999999999999998224 ) ) ;
#56609 = CARTESIAN_POINT ( 'NONE',  ( 9.001249775931846008E-16, 13.67187500061451999, -25.09994784771203058 ) ) ;
#56610 = CARTESIAN_POINT ( 'NONE',  ( 27.97500000122903074, -5.773502691896255534, -1.060575238724906372E-15 ) ) ;
#56611 = CARTESIAN_POINT ( 'NONE',  ( -3.756430356249999214, 16.42812499938548143, 27.83122392262697176 ) ) ;
#56612 = CARTESIAN_POINT ( 'NONE',  ( 6.675000000000000711, -4.330127018922194537, 2.499999999999995559 ) ) ;
#56613 = CARTESIAN_POINT ( 'NONE',  ( 0.000000000000000000, 27.50000000000000000, 30.00000000000000000 ) ) ;
#56614 = ORIENTED_EDGE ( 'NONE', *, *, #58189, .F. ) ;
#56615 = CARTESIAN_POINT ( 'NONE',  ( 20.80312500061451431, 0.000000000000000000, 5.243569643749999010 ) ) ;
#56616 = CARTESIAN_POINT ( 'NONE',  ( 13.42500000122903536, 2.886751345948126879, 4.999999999999999112 ) ) ;
#56617 = CARTESIAN_POINT ( 'NONE',  ( 3.346476778685950837, -3.715034440765132562, -3.519825879858566431 ) ) ;
#56618 = CARTESIAN_POINT ( 'NONE',  ( 28.58437500061451786, -4.541064518000419881, 2.621784821874995952 ) ) ;
#56619 = CARTESIAN_POINT ( 'NONE',  ( 20.03437500061451715, -4.541064518000419881, 2.621784821874995952 ) ) ;
#56620 = CARTESIAN_POINT ( 'NONE',  ( 17.01562500061451644, 3.027376345333613106, -5.243569643749998122 ) ) ;
#56621 = CARTESIAN_POINT ( 'NONE',  ( -2.121784821874999949, 11.17812500061459424, -33.67503911421598417 ) ) ;
#56622 = CARTESIAN_POINT ( 'NONE',  ( 6.965625000614518392, -6.054752690667223547, -1.112240025338166033E-15 ) ) ;
#56623 =( BOUNDED_CURVE ( )  B_SPLINE_CURVE ( 2, ( #40832, #18259, #29377, #13445, #46007, #41546, #68543, #63348, #7557 ),
 .UNSPECIFIED., .F., .F. ) 
 B_SPLINE_CURVE_WITH_KNOTS ( ( 3, 2, 2, 2, 3 ),
 ( 0.8804347826086956763, 0.8840579710144927938, 0.8913043478260869179, 0.8985507246376811530, 0.9021739130434782705 ),
 .UNSPECIFIED. ) 
 CURVE ( )  GEOMETRIC_REPRESENTATION_ITEM ( )  RATIONAL_B_SPLINE_CURVE ( ( 0.9330127018922194093, 0.9330127018922194093, 1.000000000000000000, 0.8660254037844387076, 1.000000000000000000, 0.8660254037844387076, 1.000000000000000000, 0.9330127018922194093, 0.9330127018922194093 ) ) 
 REPRESENTATION_ITEM ( '' )  );
#56624 = CARTESIAN_POINT ( 'NONE',  ( 27.56250000122902932, -4.330127018922190985, -2.500000000000001332 ) ) ;
#56625 = CARTESIAN_POINT ( 'NONE',  ( 20.82187500061451857, 2.746126346562643317, 4.756430356249998326 ) ) ;
#56626 = CARTESIAN_POINT ( 'NONE',  ( 19.71562500061451928, 3.027376345333612662, -5.243569643749998122 ) ) ;
#56627 = CARTESIAN_POINT ( 'NONE',  ( 30.00000000000000000, 0.000000000000000000, 0.000000000000000000 ) ) ;
#56628 = LINE ( 'NONE', #1576, #21859 ) ;
#56629 = CARTESIAN_POINT ( 'NONE',  ( 12.72187500061451537, 3.027376345333611329, 5.243569643749999010 ) ) ;
#56630 = CARTESIAN_POINT ( 'NONE',  ( 11.18437500061451928, 6.421520780324663323E-16, -5.243569643749999010 ) ) ;
#56631 = CARTESIAN_POINT ( 'NONE',  ( 19.69687500061451857, -3.027376345333610441, -5.243569643749999898 ) ) ;
#56632 = ORIENTED_EDGE ( 'NONE', *, *, #10028, .T. ) ;
#56633 = CARTESIAN_POINT ( 'NONE',  ( 24.92812500061451431, -4.541064518000419881, 2.621784821874995952 ) ) ;
#56634 = CARTESIAN_POINT ( 'NONE',  ( 19.28437500061451360, 6.421520780324663323E-16, -5.243569643749999010 ) ) ;
#56635 = CARTESIAN_POINT ( 'NONE',  ( 23.72812500061451502, 6.421520780324663323E-16, -5.243569643749999010 ) ) ;
#56636 = CARTESIAN_POINT ( 'NONE',  ( 7.781250001229034652, 6.123233995736764310E-16, -4.999999999999998224 ) ) ;
#56637 = CARTESIAN_POINT ( 'NONE',  ( -3.999999999999997335, 17.33749999999999858, 32.30940107675850470 ) ) ;
#56638 = CARTESIAN_POINT ( 'NONE',  ( 3.721875000614518036, 3.027376345333611329, 5.243569643749999010 ) ) ;
#56639 = CARTESIAN_POINT ( 'NONE',  ( 12.71250000122903145, -4.330127018922190985, -2.500000000000001332 ) ) ;
#56640 = CARTESIAN_POINT ( 'NONE',  ( 6.150000001229033231, 5.773502691896255534, 3.535250795749688894E-16 ) ) ;
#56641 = CARTESIAN_POINT ( 'NONE',  ( 4.000000000000000000, 19.28750000000000142, -27.69059892324149530 ) ) ;
#56642 = CARTESIAN_POINT ( 'NONE',  ( 26.73750000122903003, 6.123233995736764310E-16, -4.999999999999998224 ) ) ;
#56643 = CARTESIAN_POINT ( 'NONE',  ( -4.000000000000000888, 17.65624999877096712, 32.30940107675850470 ) ) ;
#56644 = CARTESIAN_POINT ( 'NONE',  ( 16.93125000122903145, 4.330127018922191873, 2.499999999999999556 ) ) ;
#56645 = CARTESIAN_POINT ( 'NONE',  ( 11.63437500061451857, 6.421520780324663323E-16, -5.243569643749999010 ) ) ;
#56646 = FACE_OUTER_BOUND ( 'NONE', #59816, .T. ) ;
#56647 = CARTESIAN_POINT ( 'NONE',  ( 17.69062500061451715, -3.027376345333614438, 5.243569643749998122 ) ) ;
#56648 = CARTESIAN_POINT ( 'NONE',  ( 12.98437500061451821, 6.421520780324663323E-16, -5.243569643749999010 ) ) ;
#56649 = CARTESIAN_POINT ( 'NONE',  ( 3.965625000614515727, 3.027376345333613106, -5.243569643749998122 ) ) ;
#56650 = CARTESIAN_POINT ( 'NONE',  ( 19.62187500061451573, -6.054752690667223547, -1.112240025338166033E-15 ) ) ;
#56651 = CARTESIAN_POINT ( 'NONE',  ( 10.09687500061451715, -3.027376345333614438, 5.243569643749998122 ) ) ;
#56652 = LINE ( 'NONE', #6410, #39520 ) ;
#56653 = CARTESIAN_POINT ( 'NONE',  ( 1.071796769724495002, 16.00759618943233775, 34.00000000000000000 ) ) ;
#56654 = CARTESIAN_POINT ( 'NONE',  ( 5.700000001229033941, 5.773502691896255534, 3.535250795749688894E-16 ) ) ;
#56655 = CARTESIAN_POINT ( 'NONE',  ( 19.67812500061451786, 6.421520780324663323E-16, -5.243569643749999010 ) ) ;
#56656 =( BOUNDED_CURVE ( )  B_SPLINE_CURVE ( 2, ( #45627, #40086, #52605, #64041, #64773, #69956, #36697 ),
 .UNSPECIFIED., .F., .F. ) 
 B_SPLINE_CURVE_WITH_KNOTS ( ( 3, 2, 2, 3 ),
 ( 0.05000000000000003053, 0.05277777777777779844, 0.05555555555555556635, 0.05833333333333334120 ),
 .UNSPECIFIED. ) 
 CURVE ( )  GEOMETRIC_REPRESENTATION_ITEM ( )  RATIONAL_B_SPLINE_CURVE ( ( 0.9999999999999986677, 0.8660254037844400399, 1.000000000000000000, 0.8660254037844387076, 1.000000000000000000, 0.8660254037844383745, 1.000000000000000222 ) ) 
 REPRESENTATION_ITEM ( '' )  );
#56657 = CARTESIAN_POINT ( 'NONE',  ( 6.862500001229034474, -4.330127018922190985, -2.500000000000001332 ) ) ;
#56658 = CARTESIAN_POINT ( 'NONE',  ( 18.25312500061451715, -4.541064518000417216, -2.621784821875001281 ) ) ;
#56659 = CARTESIAN_POINT ( 'NONE',  ( 13.00312500061451537, 4.541064518000418104, -2.621784821874998173 ) ) ;
#56660 = CARTESIAN_POINT ( 'NONE',  ( 25.88437500061451502, -4.119189519843968306, 2.378215178124996054 ) ) ;
#56661 = CARTESIAN_POINT ( 'NONE',  ( 13.53749999999999964, -2.886751345948125991, -5.000000000000000000 ) ) ;
#56662 = CARTESIAN_POINT ( 'NONE',  ( 8.512500001229033941, 0.000000000000000000, 4.999999999999998224 ) ) ;
#56663 = CARTESIAN_POINT ( 'NONE',  ( 6.253125000614517148, 4.541064518000418104, -2.621784821874998173 ) ) ;
#56664 = CARTESIAN_POINT ( 'NONE',  ( 18.07500000122903216, -5.773502691896255534, -1.060575238724906372E-15 ) ) ;
#56665 = CARTESIAN_POINT ( 'NONE',  ( 25.98750000000000071, -2.886751345948129988, 4.999999999999997335 ) ) ;
#56666 = CARTESIAN_POINT ( 'NONE',  ( 4.243569643749999898, 11.49687500061451928, -27.54997392385601529 ) ) ;
#56667 = CARTESIAN_POINT ( 'NONE',  ( 4.561349860989134974, -2.048213574975756401, 4.693545306252407734 ) ) ;
#56668 = EDGE_CURVE ( 'NONE', #51781, #18169, #40225, .T. ) ;
#56669 = CARTESIAN_POINT ( 'NONE',  ( 2.775000001229033675, -5.773502691896255534, -1.060575238724906372E-15 ) ) ;
#56670 = CARTESIAN_POINT ( 'NONE',  ( 20.18437500061451573, 6.421520780324663323E-16, -5.243569643749999010 ) ) ;
#56671 = CARTESIAN_POINT ( 'NONE',  ( 17.12812500061451715, 4.541064518000418104, 2.621784821874999949 ) ) ;
#56672 = CARTESIAN_POINT ( 'NONE',  ( 12.54375000122903394, -2.886751345948129988, 4.999999999999997335 ) ) ;
#56673 = CARTESIAN_POINT ( 'NONE',  ( 11.06250000000000178, 2.886751345948126879, 4.999999999999998224 ) ) ;
#56674 = CARTESIAN_POINT ( 'NONE',  ( -5.810221930991193690E-16, 14.15000000122903145, 26.00000000000000355 ) ) ;
#56675 = CARTESIAN_POINT ( 'NONE',  ( 27.08437500061451786, 4.541064518000418104, 2.621784821874999949 ) ) ;
#56676 = CARTESIAN_POINT ( 'NONE',  ( 17.85937500061451644, 2.746126346562645981, -4.756430356249997438 ) ) ;
#56677 = CARTESIAN_POINT ( 'NONE',  ( 11.31562500061451892, 3.027376345333611329, 5.243569643749999010 ) ) ;
#56678 = CARTESIAN_POINT ( 'NONE',  ( 11.97187500061451892, -6.054752690667223547, -1.112240025338166033E-15 ) ) ;
#56679 = ORIENTED_EDGE ( 'NONE', *, *, #45231, .T. ) ;
#56680 = CARTESIAN_POINT ( 'NONE',  ( 9.375000000000001776, -4.330127018922194537, 2.499999999999995559 ) ) ;
#56681 = CARTESIAN_POINT ( 'NONE',  ( 20.76562500061451644, 3.027376345333611329, 5.243569643749999010 ) ) ;
#56682 = DIRECTION ( 'NONE',  ( -0.000000000000000000, -1.000000000000000000, -0.000000000000000000 ) ) ;
#56683 = CARTESIAN_POINT ( 'NONE',  ( 12.67499999999999893, 6.123233995736764310E-16, -4.999999999999998224 ) ) ;
#56684 = CARTESIAN_POINT ( 'NONE',  ( 22.08750000122903501, -4.330127018922194537, 2.499999999999995559 ) ) ;
#56685 = CARTESIAN_POINT ( 'NONE',  ( 15.47812500061451679, -4.541064518000419881, 2.621784821874995952 ) ) ;
#56686 = CARTESIAN_POINT ( 'NONE',  ( 13.17187500061451466, -4.119189519843968306, 2.378215178124996054 ) ) ;
#56687 = ORIENTED_EDGE ( 'NONE', *, *, #25127, .F. ) ;
#56688 = CARTESIAN_POINT ( 'NONE',  ( 20.40000000000000213, 4.330127018922192761, -2.499999999999997780 ) ) ;
#56689 = CARTESIAN_POINT ( 'NONE',  ( 23.55000000000000071, 4.330127018922192761, -2.499999999999997780 ) ) ;
#56690 = CARTESIAN_POINT ( 'NONE',  ( 22.13437500061451502, 4.541064518000418104, 2.621784821874999949 ) ) ;
#56691 = CARTESIAN_POINT ( 'NONE',  ( 25.86562500061451431, -6.054752690667223547, -1.112240025338166033E-15 ) ) ;
#56692 = ORIENTED_EDGE ( 'NONE', *, *, #23221, .T. ) ;
#56693 = CARTESIAN_POINT ( 'NONE',  ( 8.962500001229033231, 0.000000000000000000, 4.999999999999998224 ) ) ;
#56694 = CARTESIAN_POINT ( 'NONE',  ( 7.565625000614518036, 3.027376345333613106, -5.243569643749998122 ) ) ;
#56695 = CARTESIAN_POINT ( 'NONE',  ( 12.41249999999999964, 2.886751345948182834, 4.999999999999902300 ) ) ;
#56696 = CARTESIAN_POINT ( 'NONE',  ( 14.66249999999999964, 2.886751345948126879, 4.999999999999999112 ) ) ;
#56697 = CARTESIAN_POINT ( 'NONE',  ( 9.001249775931846008E-16, 18.56562500061451715, 34.90005215228797653 ) ) ;
#56698 = CARTESIAN_POINT ( 'NONE',  ( 3.834375000614519635, -4.541064518000419881, 2.621784821874995952 ) ) ;
#56699 = CARTESIAN_POINT ( 'NONE',  ( 27.38437500061451857, 6.421520780324663323E-16, -5.243569643749999010 ) ) ;
#56700 = ORIENTED_EDGE ( 'NONE', *, *, #14319, .T. ) ;
#56701 = CARTESIAN_POINT ( 'NONE',  ( 24.29062500061451502, 6.054752690667223547, 3.707466751127219781E-16 ) ) ;
#56702 = CARTESIAN_POINT ( 'NONE',  ( 25.47187500061451715, -6.054752690667223547, -1.112240025338166033E-15 ) ) ;
#56703 = CARTESIAN_POINT ( 'NONE',  ( 11.62500000000000000, -4.330127018922194537, 2.499999999999995559 ) ) ;
#56704 = CARTESIAN_POINT ( 'NONE',  ( 8.690625000614515372, -3.027376345333614438, 5.243569643749998122 ) ) ;
#56705 = CARTESIAN_POINT ( 'NONE',  ( 3.849931240356728512, 3.190302406438068505, 3.849931240356827544 ) ) ;
#56706 = CARTESIAN_POINT ( 'NONE',  ( 2.000000000000001332, 11.15000000000000213, 33.46410161513774995 ) ) ;
#56707 = CARTESIAN_POINT ( 'NONE',  ( 25.60312500061451502, 4.541064518000418104, -2.621784821874998173 ) ) ;
#56708 = CARTESIAN_POINT ( 'NONE',  ( 8.456250001229033586, 0.000000000000000000, 4.999999999999998224 ) ) ;
#56709 = CARTESIAN_POINT ( 'NONE',  ( 12.60937500061451821, 4.119189519843966529, -2.378215178124998275 ) ) ;
#56710 = CARTESIAN_POINT ( 'NONE',  ( 18.53437500061451715, 4.541064518000418104, 2.621784821874999949 ) ) ;
#56711 = CARTESIAN_POINT ( 'NONE',  ( 2.121784821874999061, 15.20937500061451786, 26.32496088578401583 ) ) ;
#56712 = CARTESIAN_POINT ( 'NONE',  ( 18.68437500061451928, -4.541064518000419881, 2.621784821874995952 ) ) ;
#56713 = CARTESIAN_POINT ( 'NONE',  ( 27.64687500061452141, -3.027376345333614438, 5.243569643749998122 ) ) ;
#56714 = CARTESIAN_POINT ( 'NONE',  ( 4.243569643749999898, 16.44687500061451857, 32.45002607614398471 ) ) ;
#56715 = CARTESIAN_POINT ( 'NONE',  ( 9.815625000614518925, 3.027376345333613106, -5.243569643749998122 ) ) ;
#56716 = CARTESIAN_POINT ( 'NONE',  ( 3.999999999999999112, 17.18750000122903288, 30.00000000000000000 ) ) ;
#56717 = CARTESIAN_POINT ( 'NONE',  ( 4.846875000614519813, -3.027376345333610441, -5.243569643749999898 ) ) ;
#56718 = CARTESIAN_POINT ( 'NONE',  ( 30.00000000000000000, 0.000000000000000000, 0.000000000000000000 ) ) ;
#56719 = CARTESIAN_POINT ( 'NONE',  ( 7.040625000614517681, -3.027376345333610441, -5.243569643749999898 ) ) ;
#56720 = CARTESIAN_POINT ( 'NONE',  ( 11.70937500061451608, 4.541064518000418104, -2.621784821874998173 ) ) ;
#56721 = CARTESIAN_POINT ( 'NONE',  ( 20.21250000122903145, 0.000000000000000000, 4.999999999999998224 ) ) ;
#56722 = CARTESIAN_POINT ( 'NONE',  ( 6.121875000614517504, -6.054752690667223547, -1.112240025338166033E-15 ) ) ;
#56723 = CARTESIAN_POINT ( 'NONE',  ( 10.82812500061451644, 4.541064518000418104, 2.621784821874999949 ) ) ;
#56724 = CARTESIAN_POINT ( 'NONE',  ( 5.690625000614515372, -3.027376345333610441, -5.243569643749999898 ) ) ;
#56725 = CARTESIAN_POINT ( 'NONE',  ( 22.48125000122903216, -4.330127018922194537, 2.499999999999995559 ) ) ;
#56726 = CARTESIAN_POINT ( 'NONE',  ( 19.02187500061451786, 3.027376345333611329, 5.243569643749999010 ) ) ;
#56727 = CARTESIAN_POINT ( 'NONE',  ( -3.999999999999999112, 11.52500000122903501, 27.69059892324149885 ) ) ;
#56728 = ORIENTED_EDGE ( 'NONE', *, *, #47742, .T. ) ;
#56729 = CARTESIAN_POINT ( 'NONE',  ( 24.70312500061451644, 4.541064518000418104, -2.621784821874998173 ) ) ;
#56730 = CARTESIAN_POINT ( 'NONE',  ( 12.32812500061451821, -4.541064518000419881, 2.621784821874995952 ) ) ;
#56731 = PLANE ( 'NONE',  #63189 ) ;
#56732 = CARTESIAN_POINT ( 'NONE',  ( 12.17812500061451608, 4.541064518000418104, 2.621784821874999949 ) ) ;
#56733 = CARTESIAN_POINT ( 'NONE',  ( 9.001249775931846008E-16, 10.07187500061451857, -25.09994784771203058 ) ) ;
#56734 = CARTESIAN_POINT ( 'NONE',  ( 13.12500000122903288, -5.773502691896255534, -1.060575238724906372E-15 ) ) ;
#56735 = ADVANCED_FACE ( 'NONE', ( #62384 ), #67939, .F. ) ;
#56736 = CARTESIAN_POINT ( 'NONE',  ( 26.39062500061451644, -3.027376345333610441, -5.243569643749999898 ) ) ;
#56737 = CARTESIAN_POINT ( 'NONE',  ( 9.001249775931846008E-16, 12.26562500061451644, -25.09994784771203058 ) ) ;
#56738 = CARTESIAN_POINT ( 'NONE',  ( 15.41250000122903252, -4.330127018922190985, -2.500000000000001332 ) ) ;
#56739 = CARTESIAN_POINT ( 'NONE',  ( 12.00000000000000000, 0.000000000000000000, 4.999999999999998224 ) ) ;
#56740 = CARTESIAN_POINT ( 'NONE',  ( 21.10312500061451502, 4.541064518000418104, -2.621784821874998173 ) ) ;
#56741 = CARTESIAN_POINT ( 'NONE',  ( 8.934375000614517504, 6.421520780324663323E-16, -5.243569643749999010 ) ) ;
#56742 = CARTESIAN_POINT ( 'NONE',  ( 7.425000001229034474, 2.886751345948129099, -4.999999999999998224 ) ) ;
#56743 = CARTESIAN_POINT ( 'NONE',  ( 15.26250000122903216, 0.000000000000000000, 4.999999999999998224 ) ) ;
#56744 = CARTESIAN_POINT ( 'NONE',  ( 11.65312500061451573, 4.541064518000418104, -2.621784821874998173 ) ) ;
#56745 = CARTESIAN_POINT ( 'NONE',  ( 16.82812500061451644, -4.541064518000419881, 2.621784821874995952 ) ) ;
#56746 = CARTESIAN_POINT ( 'NONE',  ( 28.98750000122903359, 6.123233995736764310E-16, -4.999999999999998224 ) ) ;
#56747 = CARTESIAN_POINT ( 'NONE',  ( 23.36250000000000071, -5.773502691896255534, -1.060575238724906372E-15 ) ) ;
#56748 = CARTESIAN_POINT ( 'NONE',  ( 22.99687500061451573, 6.054752690667223547, 3.707466751127219781E-16 ) ) ;
#56749 = CARTESIAN_POINT ( 'NONE',  ( 30.00000000000000000, 0.000000000000000000, 0.000000000000000000 ) ) ;
#56750 = CARTESIAN_POINT ( 'NONE',  ( 9.975000001229034297, -5.773502691896255534, -1.060575238724906372E-15 ) ) ;
#56751 = CARTESIAN_POINT ( 'NONE',  ( 27.45937500061451786, 4.541064518000418104, -2.621784821874998173 ) ) ;
#56752 = CARTESIAN_POINT ( 'NONE',  ( 5.634375000614519458, -4.541064518000419881, 2.621784821874995952 ) ) ;
#56753 = CARTESIAN_POINT ( 'NONE',  ( 24.29062500061451502, 6.054752690667223547, 3.707466751127219781E-16 ) ) ;
#56754 = CARTESIAN_POINT ( 'NONE',  ( -3.756430356249999214, 14.29062499938548214, 27.83122392262697176 ) ) ;
#56755 = CYLINDRICAL_SURFACE ( 'NONE', #16142, 4.000000000000000000 ) ;
#56756 = CARTESIAN_POINT ( 'NONE',  ( 9.984375000614518214, 4.541064518000418104, 2.621784821874999949 ) ) ;
#56757 = CARTESIAN_POINT ( 'NONE',  ( 1.071796769724489895, 12.66740381056766651, 26.00000000000000355 ) ) ;
#56758 = CARTESIAN_POINT ( 'NONE',  ( 29.69062500061451715, 6.054752690667223547, 3.707466751127219781E-16 ) ) ;
#56759 = CARTESIAN_POINT ( 'NONE',  ( 6.646875000614518747, -3.027376345333610441, -5.243569643749999898 ) ) ;
#56760 = CARTESIAN_POINT ( 'NONE',  ( -5.810221930991193690E-16, 14.48749999999999893, 26.00000000000000355 ) ) ;
#56761 = CARTESIAN_POINT ( 'NONE',  ( 27.19687500061451857, -3.027376345333614438, 5.243569643749998122 ) ) ;
#56762 = EDGE_CURVE ( 'NONE', #53784, #24717, #37887, .T. ) ;
#56763 = CARTESIAN_POINT ( 'NONE',  ( 2.121784821874999061, 11.10312500061459495, 26.32496088578401583 ) ) ;
#56764 = CARTESIAN_POINT ( 'NONE',  ( 19.31250000000000000, -5.773502691896255534, -1.060575238724906372E-15 ) ) ;
#56765 = ORIENTED_EDGE ( 'NONE', *, *, #27624, .T. ) ;
#56766 = CARTESIAN_POINT ( 'NONE',  ( 26.51249999999999929, -5.773502691896255534, -1.060575238724906372E-15 ) ) ;
#56767 = CARTESIAN_POINT ( 'NONE',  ( 29.25937500061451502, 4.541064518000418104, -2.621784821874998173 ) ) ;
#56768 = ORIENTED_EDGE ( 'NONE', *, *, #4430, .T. ) ;
#56769 = CARTESIAN_POINT ( 'NONE',  ( 16.64062500061451289, 6.054752690667223547, 3.707466751127219781E-16 ) ) ;
#56770 = CARTESIAN_POINT ( 'NONE',  ( 7.903125000614515727, -4.541064518000417216, -2.621784821875001281 ) ) ;
#56771 = CARTESIAN_POINT ( 'NONE',  ( 19.88437500061451502, -2.746126346562646425, 4.756430356249996549 ) ) ;
#56772 = CARTESIAN_POINT ( 'NONE',  ( 4.546875000614517326, 6.054752690667223547, 3.707466751127219781E-16 ) ) ;
#56773 = CARTESIAN_POINT ( 'NONE',  ( 17.02500000122903145, 2.886751345948126879, 4.999999999999999112 ) ) ;
#56774 = CARTESIAN_POINT ( 'NONE',  ( 22.01249999999999574, -5.773502691896255534, -1.060575238724906372E-15 ) ) ;
#56775 = CARTESIAN_POINT ( 'NONE',  ( 3.571875000614517237, 3.027376345333613106, -5.243569643749998122 ) ) ;
#56776 = CARTESIAN_POINT ( 'NONE',  ( 10.54687500061451644, -3.027376345333614438, 5.243569643749998122 ) ) ;
#56777 = CARTESIAN_POINT ( 'NONE',  ( 20.93437500061451573, -4.541064518000419881, 2.621784821874995952 ) ) ;
#56778 = CARTESIAN_POINT ( 'NONE',  ( -1.071796769724483234, 17.20759618943233704, -34.00000000000000711 ) ) ;
#56779 = ORIENTED_EDGE ( 'NONE', *, *, #55506, .F. ) ;
#56780 = CARTESIAN_POINT ( 'NONE',  ( 3.684375000614518836, 4.541064518000418104, 2.621784821874999949 ) ) ;
#56781 = CARTESIAN_POINT ( 'NONE',  ( 7.884375000614517681, -4.541064518000419881, 2.621784821874995952 ) ) ;
#56782 = CARTESIAN_POINT ( 'NONE',  ( 17.92500000000000071, -4.330127018922194537, 2.499999999999995559 ) ) ;
#56783 = CARTESIAN_POINT ( 'NONE',  ( 16.04062500061451857, -3.027376345333610441, -5.243569643749999898 ) ) ;
#56784 = CARTESIAN_POINT ( 'NONE',  ( -1.999999999999999112, 19.84999999999999787, 26.53589838486224650 ) ) ;
#56786 = DIRECTION ( 'NONE',  ( -1.000000000000000000, -0.000000000000000000, -0.000000000000000000 ) ) ;
#56785 =( GEOMETRIC_REPRESENTATION_CONTEXT ( 3 ) GLOBAL_UNCERTAINTY_ASSIGNED_CONTEXT ( ( #70562 ) ) GLOBAL_UNIT_ASSIGNED_CONTEXT ( ( #54189, #23466, #6847 ) ) REPRESENTATION_CONTEXT ( 'NONE', 'WORKASPACE' ) );
#56787 = CARTESIAN_POINT ( 'NONE',  ( 18.98437500061451644, 4.119189519843966529, 2.378215178124999607 ) ) ;
#56788 = CARTESIAN_POINT ( 'NONE',  ( 10.15312500061451750, -4.541064518000417216, -2.621784821875001281 ) ) ;
#56789 = CARTESIAN_POINT ( 'NONE',  ( 26.93437500061451573, 6.421520780324663323E-16, -5.243569643749999010 ) ) ;
#56790 = CARTESIAN_POINT ( 'NONE',  ( 20.17499999999999716, -4.330127018922194537, 2.499999999999995559 ) ) ;
#56791 = CARTESIAN_POINT ( 'NONE',  ( 26.25937500061451857, 0.000000000000000000, 5.243569643749999010 ) ) ;
#56792 = CARTESIAN_POINT ( 'NONE',  ( 8.737500000000002487, 5.773502691896255534, 3.535250795749688894E-16 ) ) ;
#56793 = CARTESIAN_POINT ( 'NONE',  ( 4.000000000000000000, 15.80000000122903359, 32.30940107675849049 ) ) ;
#56794 = CARTESIAN_POINT ( 'NONE',  ( 10.12500000122903465, 2.886751345948129099, -4.999999999999998224 ) ) ;
#56795 = CARTESIAN_POINT ( 'NONE',  ( 19.99687500061451573, -3.027376345333614438, 5.243569643749998122 ) ) ;
#56796 = CARTESIAN_POINT ( 'NONE',  ( 14.07187500061451679, 3.027376345333611329, 5.243569643749999010 ) ) ;
#56797 = CARTESIAN_POINT ( 'NONE',  ( -3.305247878049081707E-15, 5.000000000000034639, -34.00000000000004263 ) ) ;
#56798 = ORIENTED_EDGE ( 'NONE', *, *, #41535, .T. ) ;
#56799 = CARTESIAN_POINT ( 'NONE',  ( 15.25312500061451715, 4.541064518000418104, -2.621784821874998173 ) ) ;
#56800 = CARTESIAN_POINT ( 'NONE',  ( 27.03750000122903430, -4.330127018922194537, 2.499999999999995559 ) ) ;
#56801 = CARTESIAN_POINT ( 'NONE',  ( 11.97187500061451892, -6.054752690667223547, -1.112240025338166033E-15 ) ) ;
#56802 = CARTESIAN_POINT ( 'NONE',  ( 3.337500000000000355, 5.773502691896255534, 3.535250795749688401E-16 ) ) ;
#56803 = CARTESIAN_POINT ( 'NONE',  ( 16.37812500061451715, -4.541064518000419881, 2.621784821874995952 ) ) ;
#56804 = CARTESIAN_POINT ( 'NONE',  ( 21.01875000122903003, 2.886751345948126879, 4.999999999999998224 ) ) ;
#56805 = CARTESIAN_POINT ( 'NONE',  ( 26.48437500061451644, 6.421520780324663323E-16, -5.243569643749999010 ) ) ;
#56806 = CARTESIAN_POINT ( 'NONE',  ( 2.923357432354301455, -4.056350739605543154, 3.322806236625610588 ) ) ;
#56807 = CARTESIAN_POINT ( 'NONE',  ( 15.42187500061451821, 3.027376345333611329, 5.243569643749999010 ) ) ;
#56808 = CARTESIAN_POINT ( 'NONE',  ( 11.06250000122903288, 4.330127018922192761, -2.499999999999997780 ) ) ;
#56809 = CARTESIAN_POINT ( 'NONE',  ( 8.596875000614518925, 5.492252693125287522, 3.363034840372157021E-16 ) ) ;
#56810 = CARTESIAN_POINT ( 'NONE',  ( -2.121784821874999949, 15.73437500061451644, -33.67503911421598417 ) ) ;
#56811 = CARTESIAN_POINT ( 'NONE',  ( 17.55937500061451573, 4.541064518000418104, -2.621784821874998173 ) ) ;
#56812 = CARTESIAN_POINT ( 'NONE',  ( 20.81250000122903643, -4.330127018922190985, -2.500000000000001332 ) ) ;
#56813 = CARTESIAN_POINT ( 'NONE',  ( 14.22187500061451537, -6.054752690667223547, -1.112240025338166033E-15 ) ) ;
#56814 = CARTESIAN_POINT ( 'NONE',  ( -4.243569643749999898, 13.07187500061452035, 27.54997392385601529 ) ) ;
#56815 = CARTESIAN_POINT ( 'NONE',  ( 22.76250000122903216, 4.330127018922192761, -2.499999999999997780 ) ) ;
#56816 = CARTESIAN_POINT ( 'NONE',  ( 14.50312500061451537, 0.000000000000000000, 5.243569643749999010 ) ) ;
#56817 = CARTESIAN_POINT ( 'NONE',  ( 25.42500000000000071, 4.330127018922191873, 2.499999999999999556 ) ) ;
#56818 = EDGE_LOOP ( 'NONE', ( #27086, #44660, #70266, #63033, #23203, #33672 ) ) ;
#56819 = VERTEX_POINT ( 'NONE', #23941 ) ;
#56820 = CARTESIAN_POINT ( 'NONE',  ( 20.10000000000000142, 0.000000000000000000, 4.999999999999998224 ) ) ;
#56821 = CARTESIAN_POINT ( 'NONE',  ( -6.275039685470489619E-15, 17.97500000122903074, 33.99999999999999289 ) ) ;
#56822 = CARTESIAN_POINT ( 'NONE',  ( 3.290625000614516793, -3.027376345333614438, 5.243569643749998122 ) ) ;
#56823 = CARTESIAN_POINT ( 'NONE',  ( 14.40000000122903323, -2.886751345948129988, 4.999999999999997335 ) ) ;
#56824 = CARTESIAN_POINT ( 'NONE',  ( 19.90312500061451573, 0.000000000000000000, 5.243569643749999010 ) ) ;
#56825 = ADVANCED_FACE ( 'NONE', ( #57918 ), #7325, .F. ) ;
#56826 = CARTESIAN_POINT ( 'NONE',  ( 22.37812500061451360, 6.421520780324663323E-16, -5.243569643749999010 ) ) ;
#56827 = CARTESIAN_POINT ( 'NONE',  ( 3.178125000614515638, 4.541064518000418104, 2.621784821874999949 ) ) ;
#56828 = CARTESIAN_POINT ( 'NONE',  ( 28.83749999999999858, -2.886751345948125991, -5.000000000000000000 ) ) ;
#56829 = CARTESIAN_POINT ( 'NONE',  ( 4.628252511229727695, 3.493065785874447826, -3.949832584684945580 ) ) ;
#56830 = CARTESIAN_POINT ( 'NONE',  ( 8.971875000614515372, 2.746126346562645981, -4.756430356249997438 ) ) ;
#56831 = CARTESIAN_POINT ( 'NONE',  ( 29.67187500061451644, 3.027376345333613106, -5.243569643749998122 ) ) ;
#56832 = CARTESIAN_POINT ( 'NONE',  ( -3.999999999999999556, 11.97500000122903252, -32.30940107675850470 ) ) ;
#56833 = CARTESIAN_POINT ( 'NONE',  ( -4.243569643749997233, 17.19687500061451502, -27.54997392385601174 ) ) ;
#56834 = CARTESIAN_POINT ( 'NONE',  ( 6.037500001229035185, 6.123233995736764310E-16, -4.999999999999998224 ) ) ;
#56835 = CARTESIAN_POINT ( 'NONE',  ( 7.912499999999999645, 2.886751345948126879, 4.999999999999999112 ) ) ;
#56836 =( BOUNDED_CURVE ( )  B_SPLINE_CURVE ( 2, ( #35136, #22242, #62485, #34407, #44796, #16689, #56231, #56935, #5625 ),
 .UNSPECIFIED., .F., .F. ) 
 B_SPLINE_CURVE_WITH_KNOTS ( ( 3, 2, 2, 2, 3 ),
 ( 0.03260869565217391908, 0.03623188405797101580, 0.04347826086956521618, 0.05072463768115942351, 0.05434782608695652717 ),
 .UNSPECIFIED. ) 
 CURVE ( )  GEOMETRIC_REPRESENTATION_ITEM ( )  RATIONAL_B_SPLINE_CURVE ( ( 0.9330127018922192983, 0.9330127018922194093, 1.000000000000000000, 0.8660254037844387076, 1.000000000000000000, 0.8660254037844387076, 1.000000000000000000, 0.9330127018922192983, 0.9330127018922194093 ) ) 
 REPRESENTATION_ITEM ( '' )  );
#56837 = CARTESIAN_POINT ( 'NONE',  ( 4.200000001229033053, -2.886751345948125991, -5.000000000000000000 ) ) ;
#56838 = CARTESIAN_POINT ( 'NONE',  ( 11.18437500061451928, 6.421520780324663323E-16, -5.243569643749999010 ) ) ;
#56839 = AXIS2_PLACEMENT_3D ( 'NONE', #23372, #17104, #11580 ) ;
#56840 = CARTESIAN_POINT ( 'NONE',  ( -1.487416814333745711E-14, 16.62500000122903288, -26.00000000000000000 ) ) ;
#56841 = CARTESIAN_POINT ( 'NONE',  ( 3.984375000614517326, 6.421520780324663323E-16, -5.243569643749999010 ) ) ;
#56842 = CARTESIAN_POINT ( 'NONE',  ( 12.07499999999999929, -4.330127018922194537, 2.499999999999995559 ) ) ;
#56843 = CARTESIAN_POINT ( 'NONE',  ( 3.999999999999998668, 19.47500000122903430, 27.69059892324149530 ) ) ;
#56844 = CARTESIAN_POINT ( 'NONE',  ( 10.80937500061451928, 4.541064518000418104, -2.621784821874998173 ) ) ;
#56845 = CARTESIAN_POINT ( 'NONE',  ( 13.99687500061451928, 6.054752690667223547, 3.707466751127219781E-16 ) ) ;
#56846 = CARTESIAN_POINT ( 'NONE',  ( -3.999999999999999112, 18.61250000000000426, -32.30940107675850470 ) ) ;
#56847 = CARTESIAN_POINT ( 'NONE',  ( 7.612500000000000711, -5.773502691896255534, -1.060575238724906372E-15 ) ) ;
#56848 = CARTESIAN_POINT ( 'NONE',  ( -3.000416591977282496E-16, 18.34062500061459744, 25.09994784771203058 ) ) ;
#56849 = CARTESIAN_POINT ( 'NONE',  ( 20.74687500061451573, 6.054752690667223547, 3.707466751127219781E-16 ) ) ;
#56850 = CARTESIAN_POINT ( 'NONE',  ( -3.137519842735245283E-14, 14.37500000122903288, -26.00000000000000711 ) ) ;
#56851 = CARTESIAN_POINT ( 'NONE',  ( 27.15000000122902790, -2.886751345948125991, -5.000000000000000000 ) ) ;
#56852 = CARTESIAN_POINT ( 'NONE',  ( 18.00937500061451502, 2.746126346562643317, 4.756430356249998326 ) ) ;
#56853 = CARTESIAN_POINT ( 'NONE',  ( 22.86562500061451431, 3.027376345333613106, -5.243569643749998122 ) ) ;
#56854 = CARTESIAN_POINT ( 'NONE',  ( 15.36562500061451608, 3.027376345333611329, 5.243569643749999010 ) ) ;
#56855 = CARTESIAN_POINT ( 'NONE',  ( 26.10937500061451644, 2.746126346562643317, 4.756430356249998326 ) ) ;
#56856 = CARTESIAN_POINT ( 'NONE',  ( 11.10937500061451644, -4.541064518000417216, -2.621784821875001281 ) ) ;
#56857 = CARTESIAN_POINT ( 'NONE',  ( 27.63749999999999929, 5.773502691896255534, 3.535250795749688894E-16 ) ) ;
#56858 = CARTESIAN_POINT ( 'NONE',  ( 25.57500000122903216, 2.886751345948126879, 4.999999999999999112 ) ) ;
#56859 = CARTESIAN_POINT ( 'NONE',  ( 4.509375000614518569, 4.541064518000418104, -2.621784821874998173 ) ) ;
#56860 = CARTESIAN_POINT ( 'NONE',  ( 13.47187500061451537, 3.027376345333613106, -5.243569643749998122 ) ) ;
#56861 = CARTESIAN_POINT ( 'NONE',  ( 28.39687500061452141, 6.054752690667223547, 3.707466751127219781E-16 ) ) ;
#56862 = DIRECTION ( 'NONE',  ( -1.000000000000000000, -0.000000000000000000, -0.000000000000000000 ) ) ;
#56863 = ADVANCED_FACE ( 'NONE', ( #18751 ), #343, .T. ) ;
#56864 = CARTESIAN_POINT ( 'NONE',  ( -1.999999999999997113, 12.08750000122903501, 33.46410161513775705 ) ) ;
#56865 = CARTESIAN_POINT ( 'NONE',  ( 22.69687500061451857, -3.027376345333614438, 5.243569643749998122 ) ) ;
#56866 = CARTESIAN_POINT ( 'NONE',  ( 14.25937500061451679, -4.541064518000417216, -2.621784821875001281 ) ) ;
#56867 = ADVANCED_FACE ( 'NONE', ( #35756 ), #45452, .T. ) ;
#56868 = CARTESIAN_POINT ( 'NONE',  ( -3.756430356249999214, 17.44062499938548427, 27.83122392262697531 ) ) ;
#56869 = CARTESIAN_POINT ( 'NONE',  ( 25.91250000000000142, 2.886751345948126879, 4.999999999999999112 ) ) ;
#56870 = CARTESIAN_POINT ( 'NONE',  ( 4.200000001229033053, -2.886751345948125991, -5.000000000000000000 ) ) ;
#56871 = CARTESIAN_POINT ( 'NONE',  ( 26.74687500061451573, -2.746126346562646425, 4.756430356249996549 ) ) ;
#56872 = CARTESIAN_POINT ( 'NONE',  ( 16.37812500061451715, -4.541064518000419881, 2.621784821874995952 ) ) ;
#56873 = CARTESIAN_POINT ( 'NONE',  ( 7.200000000000001954, -4.330127018922190985, -2.500000000000001332 ) ) ;
#56874 = CYLINDRICAL_SURFACE ( 'NONE', #25431, 3.999999999999996447 ) ;
#56875 = CARTESIAN_POINT ( 'NONE',  ( 16.61250000000000426, -5.773502691896255534, -1.060575238724906372E-15 ) ) ;
#56876 = CARTESIAN_POINT ( 'NONE',  ( -2.121784821874999949, 12.52812500061451573, 26.32496088578401938 ) ) ;
#56877 = CARTESIAN_POINT ( 'NONE',  ( 30.00000000000000000, 0.000000000000000000, 0.000000000000000000 ) ) ;
#56878 = CARTESIAN_POINT ( 'NONE',  ( 20.55000000122903359, 5.773502691896255534, 3.535250795749688894E-16 ) ) ;
#56879 = CARTESIAN_POINT ( 'NONE',  ( 28.28437500061451715, 6.421520780324663323E-16, -5.243569643749999010 ) ) ;
#56880 = ORIENTED_EDGE ( 'NONE', *, *, #47376, .T. ) ;
#56881 = CARTESIAN_POINT ( 'NONE',  ( 20.87812500061451715, -4.541064518000419881, 2.621784821874995952 ) ) ;
#56882 = CARTESIAN_POINT ( 'NONE',  ( 21.57187500061451502, 3.027376345333613106, -5.243569643749998122 ) ) ;
#56883 = CARTESIAN_POINT ( 'NONE',  ( 4.912499999999999645, -5.773502691896255534, -1.060575238724906372E-15 ) ) ;
#56884 = CARTESIAN_POINT ( 'NONE',  ( 8.653125000614515727, 0.000000000000000000, 5.243569643749999010 ) ) ;
#56885 = CARTESIAN_POINT ( 'NONE',  ( 23.24062500061451786, -3.027376345333610441, -5.243569643749999898 ) ) ;
#56886 = CARTESIAN_POINT ( 'NONE',  ( 11.55937500061451928, -4.541064518000417216, -2.621784821875001281 ) ) ;
#56887 = CARTESIAN_POINT ( 'NONE',  ( 16.28437500061452070, 4.541064518000418104, 2.621784821874999949 ) ) ;
#56888 = CARTESIAN_POINT ( 'NONE',  ( -4.243569643749999898, 17.51562500061451644, 27.54997392385601529 ) ) ;
#56889 = CARTESIAN_POINT ( 'NONE',  ( 22.38750000122903216, 4.330127018922191873, 2.499999999999999556 ) ) ;
#56890 = CARTESIAN_POINT ( 'NONE',  ( 15.60937500061451644, -4.119189519843965641, -2.378215178125001383 ) ) ;
#56891 = CARTESIAN_POINT ( 'NONE',  ( 9.628125000614517148, -4.541064518000419881, 2.621784821874995952 ) ) ;
#56892 = CARTESIAN_POINT ( 'NONE',  ( 4.546875000614517326, 6.054752690667223547, 3.707466751127219781E-16 ) ) ;
#56893 = CARTESIAN_POINT ( 'NONE',  ( 5.296875000614518214, -3.027376345333610441, -5.243569643749999898 ) ) ;
#56894 = ORIENTED_EDGE ( 'NONE', *, *, #2674, .F. ) ;
#56895 = CARTESIAN_POINT ( 'NONE',  ( 24.57187500061451502, -6.054752690667223547, -1.112240025338166033E-15 ) ) ;
#56896 = CARTESIAN_POINT ( 'NONE',  ( 17.76562500061451644, -6.054752690667223547, -1.112240025338166033E-15 ) ) ;
#56897 = CARTESIAN_POINT ( 'NONE',  ( 26.70000000122903572, -2.886751345948125991, -5.000000000000000000 ) ) ;
#56898 = CARTESIAN_POINT ( 'NONE',  ( 28.86562500061451786, 3.027376345333611329, 5.243569643749999010 ) ) ;
#56899 = AXIS2_PLACEMENT_3D ( 'NONE', #19620, #30718, #53251 ) ;
#56900 = CARTESIAN_POINT ( 'NONE',  ( 21.12187500061451573, 3.027376345333613106, -5.243569643749998122 ) ) ;
#56901 = CARTESIAN_POINT ( 'NONE',  ( 17.95312500061451644, 4.541064518000418104, -2.621784821874998173 ) ) ;
#56902 = CARTESIAN_POINT ( 'NONE',  ( 4.243569643749999898, 19.59687500061452070, 32.45002607614398471 ) ) ;
#56903 = CARTESIAN_POINT ( 'NONE',  ( 22.22812500061451502, -4.541064518000419881, 2.621784821874995952 ) ) ;
#56904 = CARTESIAN_POINT ( 'NONE',  ( 7.303125000614516082, 0.000000000000000000, 4.756430356249998326 ) ) ;
#56905 = ORIENTED_EDGE ( 'NONE', *, *, #51310, .F. ) ;
#56906 = CARTESIAN_POINT ( 'NONE',  ( 27.33750000000000213, -2.886751345948129988, 4.999999999999997335 ) ) ;
#56907 = CARTESIAN_POINT ( 'NONE',  ( -3.999999999999997335, 13.28749999999999964, -27.69059892324149175 ) ) ;
#56908 = CARTESIAN_POINT ( 'NONE',  ( -3.756430356249999214, 18.34062499938548640, 27.83122392262697531 ) ) ;
#56909 = CARTESIAN_POINT ( 'NONE',  ( 29.54062500061451502, -3.027376345333610441, -5.243569643749999898 ) ) ;
#56910 = CARTESIAN_POINT ( 'NONE',  ( 9.740625000614516082, -3.027376345333610441, -5.243569643749999898 ) ) ;
#56911 = CARTESIAN_POINT ( 'NONE',  ( 22.20000000122903216, -2.886751345948125991, -5.000000000000000000 ) ) ;
#56912 = CARTESIAN_POINT ( 'NONE',  ( 12.30937500061451573, 0.000000000000000000, 5.243569643749999010 ) ) ;
#56913 = CARTESIAN_POINT ( 'NONE',  ( 28.41562500061451502, 3.027376345333611329, 5.243569643749999010 ) ) ;
#56914 = CARTESIAN_POINT ( 'NONE',  ( 28.91250000000000497, 2.886751345948129099, -4.999999999999998224 ) ) ;
#56915 = EDGE_CURVE ( 'NONE', #44045, #55550, #5673, .T. ) ;
#56916 = CARTESIAN_POINT ( 'NONE',  ( -3.999999999999997335, 18.35000000122903430, -27.69059892324149175 ) ) ;
#56917 = CARTESIAN_POINT ( 'NONE',  ( 25.16250000122903074, 0.000000000000000000, 4.999999999999998224 ) ) ;
#56918 = CARTESIAN_POINT ( 'NONE',  ( 11.80312500061451608, 0.000000000000000000, 5.243569643749999010 ) ) ;
#56919 = ORIENTED_EDGE ( 'NONE', *, *, #9235, .T. ) ;
#56920 = CARTESIAN_POINT ( 'NONE',  ( 8.578125000614518214, 4.541064518000418104, 2.621784821874999949 ) ) ;
#56921 = CARTESIAN_POINT ( 'NONE',  ( 6.515625000614516438, -6.054752690667223547, -1.112240025338166033E-15 ) ) ;
#56922 = CARTESIAN_POINT ( 'NONE',  ( 15.42187500061451821, 2.746126346562643317, 4.756430356249998326 ) ) ;
#56923 = FACE_OUTER_BOUND ( 'NONE', #64710, .T. ) ;
#56924 = CARTESIAN_POINT ( 'NONE',  ( 15.26249999999999929, -5.773502691896255534, -1.060575238724906372E-15 ) ) ;
#56925 = CARTESIAN_POINT ( 'NONE',  ( 15.72187500061451892, 3.027376345333613106, -5.243569643749998122 ) ) ;
#56926 = CARTESIAN_POINT ( 'NONE',  ( 11.58750000122903501, 4.330127018922191873, 2.499999999999999556 ) ) ;
#56927 = CARTESIAN_POINT ( 'NONE',  ( 18.45937500061451431, 4.541064518000418104, -2.621784821874998173 ) ) ;
#56928 = CARTESIAN_POINT ( 'NONE',  ( 17.62500000000000000, 6.123233995736764310E-16, -4.999999999999998224 ) ) ;
#56929 = CARTESIAN_POINT ( 'NONE',  ( 20.37187500061451573, 3.027376345333611329, 5.243569643749999010 ) ) ;
#56930 = CARTESIAN_POINT ( 'NONE',  ( 4.243569643749999898, 14.17812500061451608, -30.00000000000000000 ) ) ;
#56931 = LINE ( 'NONE', #23315, #12356 ) ;
#56932 = CARTESIAN_POINT ( 'NONE',  ( 25.65937500061451360, 2.746126346562643317, 4.756430356249998326 ) ) ;
#56933 = CARTESIAN_POINT ( 'NONE',  ( 4.000000000000000000, 15.18124999877096570, 27.69059892324149885 ) ) ;
#56934 = CARTESIAN_POINT ( 'NONE',  ( 26.76562500061451644, -6.054752690667223547, -1.112240025338166033E-15 ) ) ;
#56935 = CARTESIAN_POINT ( 'NONE',  ( -1.071796769724490117, 19.45759618943232994, -34.00000000000000000 ) ) ;
#56936 = CARTESIAN_POINT ( 'NONE',  ( 28.69687500061451502, -3.027376345333610441, -5.243569643749999898 ) ) ;
#56937 = CARTESIAN_POINT ( 'NONE',  ( 25.31250000000000000, 2.886751345948129099, -4.999999999999998224 ) ) ;
#56938 = CARTESIAN_POINT ( 'NONE',  ( 6.553125000614518747, -4.541064518000417216, -2.621784821875001281 ) ) ;
#56939 = VECTOR ( 'NONE', #20544, 1000.000000000000000 ) ;
#56940 = CARTESIAN_POINT ( 'NONE',  ( 24.49687500061451573, -4.119189519843965641, -2.378215178125001383 ) ) ;
#56941 = CARTESIAN_POINT ( 'NONE',  ( 19.54687500061451644, -3.027376345333614438, 5.243569643749998122 ) ) ;
#56942 = CARTESIAN_POINT ( 'NONE',  ( 11.52187500061451608, 5.824947211148865298E-16, -4.756430356249998326 ) ) ;
#56943 = CARTESIAN_POINT ( 'NONE',  ( 5.240625000614516971, -3.027376345333610441, -5.243569643749999898 ) ) ;
#56944 = CARTESIAN_POINT ( 'NONE',  ( 10.24687500061451750, -3.027376345333610441, -5.243569643749999898 ) ) ;
#56945 = EDGE_LOOP ( 'NONE', ( #71357, #71957, #10315, #61384 ) ) ;
#56946 = CARTESIAN_POINT ( 'NONE',  ( 20.25937500061451857, 4.541064518000418104, -2.621784821874998173 ) ) ;
#56947 = LINE ( 'NONE', #50700, #13487 ) ;
#56948 = CARTESIAN_POINT ( 'NONE',  ( 27.97500000000000142, 6.123233995736764310E-16, -4.999999999999998224 ) ) ;
#56949 = CARTESIAN_POINT ( 'NONE',  ( 29.78437500061451715, 4.541064518000418104, 2.621784821874999949 ) ) ;
#56950 = CARTESIAN_POINT ( 'NONE',  ( 17.90625000122903288, 0.000000000000000000, 4.999999999999998224 ) ) ;
#56951 = CARTESIAN_POINT ( 'NONE',  ( 3.412230204620315011, -4.173532794979288418, -3.258368439540926698 ) ) ;
#56952 = ORIENTED_EDGE ( 'NONE', *, *, #66019, .F. ) ;
#56953 = CARTESIAN_POINT ( 'NONE',  ( 9.975000000000001421, 6.123233995736764310E-16, -4.999999999999998224 ) ) ;
#56954 = CARTESIAN_POINT ( 'NONE',  ( 13.62187500061451750, -4.119189519843968306, 2.378215178124996054 ) ) ;
#56955 = CARTESIAN_POINT ( 'NONE',  ( 25.26562500061451289, 3.027376345333611329, 5.243569643749999010 ) ) ;
#56956 = CARTESIAN_POINT ( 'NONE',  ( 14.92500000000000071, 6.123233995736764310E-16, -4.999999999999998224 ) ) ;
#56957 = EDGE_CURVE ( 'NONE', #33991, #6203, #68120, .T. ) ;
#56958 = CARTESIAN_POINT ( 'NONE',  ( 11.32500000122903394, -5.773502691896255534, -1.060575238724906372E-15 ) ) ;
#56959 = CARTESIAN_POINT ( 'NONE',  ( 8.803125000614517859, -4.541064518000417216, -2.621784821875001281 ) ) ;
#56960 = CARTESIAN_POINT ( 'NONE',  ( 9.150000000000002132, 4.330127018922192761, -2.499999999999997780 ) ) ;
#56961 = CARTESIAN_POINT ( 'NONE',  ( 18.82500000122903572, 2.886751345948060266, 5.000000000000114575 ) ) ;
#56962 = CARTESIAN_POINT ( 'NONE',  ( 29.17500000122903714, 2.886751345948126879, 4.999999999999999112 ) ) ;
#56963 = CARTESIAN_POINT ( 'NONE',  ( 3.756430356250000546, 16.27812499938548285, 27.83122392262697886 ) ) ;
#56964 = CARTESIAN_POINT ( 'NONE',  ( 7.650000000000000355, -4.330127018922190985, -2.500000000000001332 ) ) ;
#56965 = LINE ( 'NONE', #16721, #71565 ) ;
#56966 = ORIENTED_EDGE ( 'NONE', *, *, #70256, .T. ) ;
#56967 = CARTESIAN_POINT ( 'NONE',  ( 21.40312500061451573, -4.541064518000417216, -2.621784821875001281 ) ) ;
#56968 = CARTESIAN_POINT ( 'NONE',  ( 28.79062500061451502, 6.054752690667223547, 3.707466751127219781E-16 ) ) ;
#56969 = CARTESIAN_POINT ( 'NONE',  ( 29.48437500061451644, -4.541064518000419881, 2.621784821874995952 ) ) ;
#56970 = CARTESIAN_POINT ( 'NONE',  ( 18.94687500061451502, 6.054752690667223547, 3.707466751127219781E-16 ) ) ;
#56971 = CARTESIAN_POINT ( 'NONE',  ( 16.41562500061451857, -6.054752690667223547, -1.112240025338166033E-15 ) ) ;
#56972 = CARTESIAN_POINT ( 'NONE',  ( -2.121784821874999949, 11.62812500061459353, -33.67503911421598417 ) ) ;
#56973 = CARTESIAN_POINT ( 'NONE',  ( 3.928125000614516527, 6.421520780324663323E-16, -5.243569643749999010 ) ) ;
#56974 = CARTESIAN_POINT ( 'NONE',  ( 28.38750000122903216, -4.330127018922194537, 2.499999999999995559 ) ) ;
#56975 = CARTESIAN_POINT ( 'NONE',  ( 22.88437500061451857, 5.824947211148865298E-16, -4.756430356249998326 ) ) ;
#56976 = CARTESIAN_POINT ( 'NONE',  ( 18.14062500061451644, -3.027376345333614438, 5.243569643749998122 ) ) ;
#56977 = CARTESIAN_POINT ( 'NONE',  ( 1.071796769724489895, 14.01740381056766793, 26.00000000000000355 ) ) ;
#56978 = CARTESIAN_POINT ( 'NONE',  ( 3.600000001229033408, -2.886751345948129988, 4.999999999999997335 ) ) ;
#56979 = CARTESIAN_POINT ( 'NONE',  ( 12.60937500061451821, 4.541064518000418104, -2.621784821874998173 ) ) ;
#56980 = CARTESIAN_POINT ( 'NONE',  ( 13.05937500061451750, 4.541064518000418104, -2.621784821874998173 ) ) ;
#56981 = CARTESIAN_POINT ( 'NONE',  ( 19.35937500061451644, 4.541064518000418104, -2.621784821874998173 ) ) ;
#56982 = ORIENTED_EDGE ( 'NONE', *, *, #50916, .T. ) ;
#56983 = CARTESIAN_POINT ( 'NONE',  ( -5.999929701724457942, 8.000052723701786661, 29.79473720932466918 ) ) ;
#56984 = CARTESIAN_POINT ( 'NONE',  ( 24.36562500061451786, 3.027376345333611329, 5.243569643749999010 ) ) ;
#56985 = CARTESIAN_POINT ( 'NONE',  ( 18.42187500061451644, 3.027376345333613106, -5.243569643749998122 ) ) ;
#56986 = CARTESIAN_POINT ( 'NONE',  ( 24.74062500061451786, 6.054752690667223547, 3.707466751127219781E-16 ) ) ;
#56987 = CARTESIAN_POINT ( 'NONE',  ( 1.592000809091587073E-14, 15.95000000122903394, -34.00000000000000000 ) ) ;
#56988 = CARTESIAN_POINT ( 'NONE',  ( -2.000000000000000000, 17.22500000000000142, 26.53589838486224650 ) ) ;
#56989 = CARTESIAN_POINT ( 'NONE',  ( 29.35312500061451502, 0.000000000000000000, 5.243569643749999010 ) ) ;
#56990 = CARTESIAN_POINT ( 'NONE',  ( 10.80000000122903536, -2.886751345948129988, 4.999999999999997335 ) ) ;
#56991 = CARTESIAN_POINT ( 'NONE',  ( 7.687500001229033764, -4.330127018922194537, 2.499999999999995559 ) ) ;
#56992 = CARTESIAN_POINT ( 'NONE',  ( 2.000000000000001332, 19.69999999999999929, -26.53589838486224650 ) ) ;
#56993 = CARTESIAN_POINT ( 'NONE',  ( 28.23750000122903359, 4.330127018922191873, 2.499999999999999556 ) ) ;
#56994 = CARTESIAN_POINT ( 'NONE',  ( -8.484601909799255319E-16, 19.08124999877096784, 34.61880215351700940 ) ) ;
#56995 = CARTESIAN_POINT ( 'NONE',  ( 16.78125000122903288, 6.123233995736764310E-16, -4.999999999999998224 ) ) ;
#56996 = CARTESIAN_POINT ( 'NONE',  ( 8.971875000614515372, 3.027376345333613106, -5.243569643749998122 ) ) ;
#56997 = CARTESIAN_POINT ( 'NONE',  ( 10.06875000122903252, 2.886751345948129099, -4.999999999999997335 ) ) ;
#56998 = CARTESIAN_POINT ( 'NONE',  ( 17.50312500061451715, 4.541064518000418104, -2.621784821874998173 ) ) ;
#56999 = CARTESIAN_POINT ( 'NONE',  ( 11.18437500061451928, 6.421520780324663323E-16, -5.243569643749999010 ) ) ;
#57000 = CARTESIAN_POINT ( 'NONE',  ( 29.66250000122903074, 0.000000000000000000, 4.999999999999998224 ) ) ;
#57001 = CARTESIAN_POINT ( 'NONE',  ( 19.54687500061451289, -3.027376345333614438, 5.243569643749998122 ) ) ;
#57002 = CARTESIAN_POINT ( 'NONE',  ( 6.871875000614517504, 3.027376345333611329, 5.243569643749999010 ) ) ;
#57003 = CARTESIAN_POINT ( 'NONE',  ( 25.61250000122903359, 0.000000000000000000, 4.999999999999998224 ) ) ;
#57004 = CARTESIAN_POINT ( 'NONE',  ( 2.000000000000000444, 16.17500000000000071, 26.53589838486224650 ) ) ;
#57005 =( BOUNDED_CURVE ( )  B_SPLINE_CURVE ( 2, ( #1760, #17632, #57531, #17275, #57159, #56450, #68270, #69360, #34630 ),
 .UNSPECIFIED., .F., .F. ) 
 B_SPLINE_CURVE_WITH_KNOTS ( ( 3, 2, 2, 2, 3 ),
 ( 0.09722222222222222376, 0.1018518518518518462, 0.1111111111111111049, 0.1203703703703703637, 0.1250000000000000000 ),
 .UNSPECIFIED. ) 
 CURVE ( )  GEOMETRIC_REPRESENTATION_ITEM ( )  RATIONAL_B_SPLINE_CURVE ( ( 0.9330127018922192983, 0.9330127018922194093, 1.000000000000000000, 0.8660254037844387076, 1.000000000000000000, 0.8660254037844387076, 1.000000000000000000, 0.9330127018922191873, 0.9330127018922192983 ) ) 
 REPRESENTATION_ITEM ( '' )  );
#57006 = CARTESIAN_POINT ( 'NONE',  ( 10.30312500061451431, 4.541064518000418104, -2.621784821874998173 ) ) ;
#57007 = CARTESIAN_POINT ( 'NONE',  ( 19.90312500061451573, 0.000000000000000000, 5.243569643749999010 ) ) ;
#57008 = EDGE_CURVE ( 'NONE', #72520, #23570, #41273, .T. ) ;
#57009 = ORIENTED_EDGE ( 'NONE', *, *, #25685, .F. ) ;
#57010 = CARTESIAN_POINT ( 'NONE',  ( 5.250000001229035540, 5.773502691896255534, 3.535250795749688894E-16 ) ) ;
#57011 = CARTESIAN_POINT ( 'NONE',  ( 15.55312500061451608, -4.541064518000417216, -2.621784821875001281 ) ) ;
#57012 = CARTESIAN_POINT ( 'NONE',  ( 13.19062500061451537, -3.027376345333614438, 5.243569643749998122 ) ) ;
#57013 = CARTESIAN_POINT ( 'NONE',  ( 24.19687500061451857, -2.746126346562642428, -4.756430356249999214 ) ) ;
#57014 = CARTESIAN_POINT ( 'NONE',  ( 12.37500000000000000, 4.330127018922191873, 2.499999999999999556 ) ) ;
#57015 = CARTESIAN_POINT ( 'NONE',  ( 8.737500001229033586, 6.123233995736764310E-16, -4.999999999999998224 ) ) ;
#57016 = CARTESIAN_POINT ( 'NONE',  ( 5.728125000614515905, 6.421520780324663323E-16, -5.243569643749999010 ) ) ;
#57017 = CARTESIAN_POINT ( 'NONE',  ( 18.52500000122903145, -5.773502691896255534, -1.060575238724906372E-15 ) ) ;
#57018 = CARTESIAN_POINT ( 'NONE',  ( 27.37500000000000000, -4.330127018922194537, 2.499999999999995559 ) ) ;
#57019 = CARTESIAN_POINT ( 'NONE',  ( 2.121784821874999061, 11.15937500061451715, -33.67503911421598417 ) ) ;
#57020 = CARTESIAN_POINT ( 'NONE',  ( 8.550000000000002487, -4.330127018922190985, -2.500000000000001332 ) ) ;
#57021 = CARTESIAN_POINT ( 'NONE',  ( 3.975000001229033852, 2.886751345948126879, 4.999999999999999112 ) ) ;
#57022 = CARTESIAN_POINT ( 'NONE',  ( 19.24687500061452283, -3.027376345333610441, -5.243569643749999898 ) ) ;
#57023 = CARTESIAN_POINT ( 'NONE',  ( 21.45000000122903216, 5.773502691896255534, 3.535250795749688401E-16 ) ) ;
#57024 = CARTESIAN_POINT ( 'NONE',  ( 17.54062500061451502, 6.054752690667223547, 3.707466751127219781E-16 ) ) ;
#57025 = CARTESIAN_POINT ( 'NONE',  ( 9.168750001229035718, 2.886751345948129099, -4.999999999999998224 ) ) ;
#57026 = CARTESIAN_POINT ( 'NONE',  ( 22.50000000122903288, -2.886751345948163738, 4.999999999999939604 ) ) ;
#57027 = CARTESIAN_POINT ( 'NONE',  ( 29.74687500061451217, 6.054752690667223547, 3.707466751127219781E-16 ) ) ;
#57028 = CARTESIAN_POINT ( 'NONE',  ( 27.34687500061451360, -3.027376345333610441, -5.243569643749999898 ) ) ;
#57029 = CARTESIAN_POINT ( 'NONE',  ( 19.54687500061451289, -4.119189519843965641, -2.378215178125001383 ) ) ;
#57030 = CARTESIAN_POINT ( 'NONE',  ( 12.17812500061451608, 4.541064518000418104, 2.621784821874999949 ) ) ;
#57031 = CARTESIAN_POINT ( 'NONE',  ( 11.59687500061451892, -3.027376345333610441, -5.243569643749999898 ) ) ;
#57032 = VERTEX_POINT ( 'NONE', #44841 ) ;
#57033 = CARTESIAN_POINT ( 'NONE',  ( 9.412499999999999645, -5.773502691896255534, -1.060575238724906372E-15 ) ) ;
#57034 = CARTESIAN_POINT ( 'NONE',  ( 19.22812500061451502, 6.421520780324663323E-16, -5.243569643749999010 ) ) ;
#57035 = CARTESIAN_POINT ( 'NONE',  ( 45.00000000000000000, 0.000000000000000000, 4.999999999999998224 ) ) ;
#57036 = CARTESIAN_POINT ( 'NONE',  ( 20.40000000000000213, 4.330127018922192761, -2.499999999999997780 ) ) ;
#57037 =( BOUNDED_CURVE ( )  B_SPLINE_CURVE ( 2, ( #54405, #69928, #53298, #14136, #20403, #19297, #13771, #54045, #48500 ),
 .UNSPECIFIED., .F., .F. ) 
 B_SPLINE_CURVE_WITH_KNOTS ( ( 3, 2, 2, 2, 3 ),
 ( 0.1195652173913043514, 0.1231884057971014551, 0.1304347826086956486, 0.1376811594202898559, 0.1413043478260869734 ),
 .UNSPECIFIED. ) 
 CURVE ( )  GEOMETRIC_REPRESENTATION_ITEM ( )  RATIONAL_B_SPLINE_CURVE ( ( 0.9330127018922194093, 0.9330127018922194093, 1.000000000000000000, 0.8660254037844387076, 1.000000000000000000, 0.8660254037844387076, 1.000000000000000000, 0.9330127018922190762, 0.9330127018922194093 ) ) 
 REPRESENTATION_ITEM ( '' )  );
#57038 = CARTESIAN_POINT ( 'NONE',  ( 9.449999999999999289, -4.330127018922190985, -2.500000000000001332 ) ) ;
#57039 = CARTESIAN_POINT ( 'NONE',  ( 21.18750000122903288, -4.330127018922194537, 2.499999999999995559 ) ) ;
#57040 = CARTESIAN_POINT ( 'NONE',  ( 15.17812500061451608, 6.421520780324663323E-16, -5.243569643749999010 ) ) ;
#57041 = CARTESIAN_POINT ( 'NONE',  ( 10.43437500061451395, -2.746126346562646425, 4.756430356249996549 ) ) ;
#57042 = ORIENTED_EDGE ( 'NONE', *, *, #67238, .F. ) ;
#57043 = CARTESIAN_POINT ( 'NONE',  ( 19.08750000000000213, 5.773502691896255534, 3.535250795749688894E-16 ) ) ;
#57044 = CARTESIAN_POINT ( 'NONE',  ( 21.71249999999999858, 2.886751345948129099, -4.999999999999998224 ) ) ;
#57045 =( BOUNDED_CURVE ( )  B_SPLINE_CURVE ( 2, ( #61861, #6443, #28978, #45970, #41158, #41868, #30055, #24868, #24143 ),
 .UNSPECIFIED., .F., .F. ) 
 B_SPLINE_CURVE_WITH_KNOTS ( ( 3, 2, 2, 2, 3 ),
 ( 0.4891304347826087029, 0.4927536231884058204, 0.5000000000000000000, 0.5072463768115942351, 0.5108695652173913526 ),
 .UNSPECIFIED. ) 
 CURVE ( )  GEOMETRIC_REPRESENTATION_ITEM ( )  RATIONAL_B_SPLINE_CURVE ( ( 0.9330127018922194093, 0.9330127018922194093, 1.000000000000000000, 0.8660254037844387076, 1.000000000000000000, 0.8660254037844387076, 1.000000000000000000, 0.9330127018922182991, 0.9330127018922192983 ) ) 
 REPRESENTATION_ITEM ( '' )  );
#57046 = CARTESIAN_POINT ( 'NONE',  ( 19.84687500061451360, 6.054752690667223547, 3.707466751127219781E-16 ) ) ;
#57047 = CARTESIAN_POINT ( 'NONE',  ( 25.30312500061451431, 0.000000000000000000, 5.243569643749999010 ) ) ;
#57048 = ORIENTED_EDGE ( 'NONE', *, *, #4064, .T. ) ;
#57049 = CARTESIAN_POINT ( 'NONE',  ( 8.925000001229033586, 2.886751345948193936, 4.999999999999883649 ) ) ;
#57050 = CARTESIAN_POINT ( 'NONE',  ( 7.228125000614517681, 4.541064518000418104, 2.621784821874999949 ) ) ;
#57051 = CARTESIAN_POINT ( 'NONE',  ( 1.071796769724489895, 15.47990381179670116, 26.00000000000000355 ) ) ;
#57052 = CARTESIAN_POINT ( 'NONE',  ( 13.76250000000000107, 2.886751345948126879, 4.999999999999999112 ) ) ;
#57053 = CARTESIAN_POINT ( 'NONE',  ( -3.000416591977282496E-16, 17.89062500061451644, 25.09994784771203058 ) ) ;
#57054 = CARTESIAN_POINT ( 'NONE',  ( 28.26562500061451289, 3.027376345333613106, -5.243569643749998122 ) ) ;
#57055 = CARTESIAN_POINT ( 'NONE',  ( 26.70937500061451431, 0.000000000000000000, 5.243569643749999010 ) ) ;
#57056 = ORIENTED_EDGE ( 'NONE', *, *, #20794, .F. ) ;
#57057 = CARTESIAN_POINT ( 'NONE',  ( 22.90312500061451573, 4.541064518000418104, -2.621784821874998173 ) ) ;
#57058 = CARTESIAN_POINT ( 'NONE',  ( 25.24687500061451573, 6.054752690667223547, 3.707466751127219781E-16 ) ) ;
#57059 = CARTESIAN_POINT ( 'NONE',  ( 4.243569643749999898, 17.74062500061459602, -27.54997392385601529 ) ) ;
#57060 = CARTESIAN_POINT ( 'NONE',  ( 10.87500000000000000, 6.123233995736764310E-16, -4.999999999999998224 ) ) ;
#57061 = CARTESIAN_POINT ( 'NONE',  ( 9.253125000614517148, -4.541064518000417216, -2.621784821875001281 ) ) ;
#57062 = CARTESIAN_POINT ( 'NONE',  ( 28.84687500061452425, 5.492252693125287522, 3.363034840372157021E-16 ) ) ;
#57063 = CARTESIAN_POINT ( 'NONE',  ( 29.31562500061451715, 3.027376345333611329, 5.243569643749999010 ) ) ;
#57064 = CARTESIAN_POINT ( 'NONE',  ( 25.90312500061451573, -4.541064518000417216, -2.621784821875001281 ) ) ;
#57065 = CARTESIAN_POINT ( 'NONE',  ( 28.35937500061450933, 2.746126346562643317, 4.756430356249998326 ) ) ;
#57066 = CARTESIAN_POINT ( 'NONE',  ( 13.47187500061451537, 2.746126346562645981, -4.756430356249997438 ) ) ;
#57067 = CARTESIAN_POINT ( 'NONE',  ( 18.38437500061451857, 6.421520780324663323E-16, -5.243569643749999010 ) ) ;
#57068 = CARTESIAN_POINT ( 'NONE',  ( 4.243569643749999010, 11.12187500061451928, 27.54997392385601174 ) ) ;
#57069 = CARTESIAN_POINT ( 'NONE',  ( 19.05937500061451928, 0.000000000000000000, 5.243569643749999010 ) ) ;
#57070 = CARTESIAN_POINT ( 'NONE',  ( 28.28437500061451715, 6.421520780324663323E-16, -5.243569643749999010 ) ) ;
#57071 = CARTESIAN_POINT ( 'NONE',  ( -2.121784821874999949, 16.18437500061451573, 26.32496088578401938 ) ) ;
#57072 = CARTESIAN_POINT ( 'NONE',  ( 7.565625000614518036, 3.027376345333613106, -5.243569643749998122 ) ) ;
#57073 =( BOUNDED_CURVE ( )  B_SPLINE_CURVE ( 3, ( #59135, #41084, #36614, #48444 ),
 .UNSPECIFIED., .F., .F. ) 
 B_SPLINE_CURVE_WITH_KNOTS ( ( 4, 4 ),
 ( 4.712388980384689674, 5.310998844378103989 ),
 .UNSPECIFIED. ) 
 CURVE ( )  GEOMETRIC_REPRESENTATION_ITEM ( )  RATIONAL_B_SPLINE_CURVE ( ( 1.000000000000000000, 0.9703611099854635436, 0.9703611099854635436, 1.000000000000000000 ) ) 
 REPRESENTATION_ITEM ( '' )  );
#57074 = CARTESIAN_POINT ( 'NONE',  ( 3.909375000614518481, -4.541064518000417216, -2.621784821875001281 ) ) ;
#57075 = CARTESIAN_POINT ( 'NONE',  ( 2.000000000000001332, 15.65000000000000036, -26.53589838486224650 ) ) ;
#57076 = CARTESIAN_POINT ( 'NONE',  ( 6.478125000614516793, -4.541064518000419881, 2.621784821874995952 ) ) ;
#57077 = CARTESIAN_POINT ( 'NONE',  ( 12.83437500061451786, -4.541064518000419881, 2.621784821874995952 ) ) ;
#57078 = CARTESIAN_POINT ( 'NONE',  ( 18.07500000122903216, -5.773502691896255534, -1.060575238724906372E-15 ) ) ;
#57079 = CARTESIAN_POINT ( 'NONE',  ( 6.196875000614515905, -3.027376345333610441, -5.243569643749999898 ) ) ;
#57080 = CARTESIAN_POINT ( 'NONE',  ( 8.128125000614515372, 4.541064518000418104, 2.621784821874999949 ) ) ;
#57081 = CARTESIAN_POINT ( 'NONE',  ( 4.057522967627288146, -2.921730200955767298, 4.057522967627288146 ) ) ;
#57082 = CARTESIAN_POINT ( 'NONE',  ( 24.50625000122903074, 4.330127018922192761, -2.499999999999997780 ) ) ;
#57083 = CARTESIAN_POINT ( 'NONE',  ( 17.07187500061451502, 3.027376345333613106, -5.243569643749998122 ) ) ;
#57084 = DIRECTION ( 'NONE',  ( 0.000000000000000000, 0.000000000000000000, -1.000000000000000000 ) ) ;
#57085 = EDGE_LOOP ( 'NONE', ( #8260, #72686, #5863, #12804 ) ) ;
#57086 = CARTESIAN_POINT ( 'NONE',  ( 23.54062500061451146, -3.027376345333614438, 5.243569643749998122 ) ) ;
#57087 = CARTESIAN_POINT ( 'NONE',  ( 10.90312500061451928, 0.000000000000000000, 5.243569643749999010 ) ) ;
#57088 = CARTESIAN_POINT ( 'NONE',  ( 26.82187500061451857, -6.054752690667223547, -1.112240025338166033E-15 ) ) ;
#57089 = CARTESIAN_POINT ( 'NONE',  ( 10.94062500061451537, -3.027376345333614438, 5.243569643749998122 ) ) ;
#57090 = CARTESIAN_POINT ( 'NONE',  ( -2.121784821874999949, 9.884375000614518569, -33.67503911421598417 ) ) ;
#57091 = CARTESIAN_POINT ( 'NONE',  ( 12.26250000122903394, -4.330127018922190985, -2.500000000000001332 ) ) ;
#57092 = CARTESIAN_POINT ( 'NONE',  ( 27.62812500061451360, -4.541064518000419881, 2.621784821874995952 ) ) ;
#57093 = EDGE_CURVE ( 'NONE', #38622, #72150, #48826, .T. ) ;
#57094 = CARTESIAN_POINT ( 'NONE',  ( 2.121784821874999061, 12.00312500061451715, -33.67503911421598417 ) ) ;
#57095 = CARTESIAN_POINT ( 'NONE',  ( 12.67500000122903536, -5.773502691896255534, -1.060575238724906372E-15 ) ) ;
#57096 = CARTESIAN_POINT ( 'NONE',  ( 10.91250000000000320, 2.886751345948129099, -4.999999999999998224 ) ) ;
#57097 = CARTESIAN_POINT ( 'NONE',  ( 20.20312500061451644, 4.541064518000418104, -2.621784821874998173 ) ) ;
#57098 = CARTESIAN_POINT ( 'NONE',  ( 7.021875000614519635, -6.054752690667223547, -1.112240025338166033E-15 ) ) ;
#57099 = CARTESIAN_POINT ( 'NONE',  ( 19.61249999999999716, 2.886751345948126879, 4.999999999999999112 ) ) ;
#57100 = CARTESIAN_POINT ( 'NONE',  ( 8.362500001229031810, 4.330127018922192761, -2.499999999999997780 ) ) ;
#57101 = CARTESIAN_POINT ( 'NONE',  ( 16.80000000122903359, -2.886751345948125991, -5.000000000000000000 ) ) ;
#57102 = CARTESIAN_POINT ( 'NONE',  ( 13.90312500061451750, 4.541064518000418104, -2.621784821874998173 ) ) ;
#57103 = CARTESIAN_POINT ( 'NONE',  ( 16.00312500061451715, -4.541064518000417216, -2.621784821875001281 ) ) ;
#57104 = CARTESIAN_POINT ( 'NONE',  ( 26.13750000122903216, -4.330127018922194537, 2.499999999999995559 ) ) ;
#57105 = CARTESIAN_POINT ( 'NONE',  ( 19.72499999999999787, -4.330127018922194537, 2.499999999999995559 ) ) ;
#57106 = CARTESIAN_POINT ( 'NONE',  ( 23.78437500061451360, 6.421520780324663323E-16, -5.243569643749999010 ) ) ;
#57107 = FACE_OUTER_BOUND ( 'NONE', #31240, .T. ) ;
#57108 = CARTESIAN_POINT ( 'NONE',  ( 9.075000001229033941, -5.773502691896255534, -1.060575238724906372E-15 ) ) ;
#57109 = CARTESIAN_POINT ( 'NONE',  ( 9.534375000614517148, 4.541064518000418104, 2.621784821874999949 ) ) ;
#57110 = CARTESIAN_POINT ( 'NONE',  ( 24.87187500061451573, 3.027376345333611329, 5.243569643749999010 ) ) ;
#57111 = CARTESIAN_POINT ( 'NONE',  ( 3.159375000614518036, 4.541064518000418104, -2.621784821874998173 ) ) ;
#57112 = CARTESIAN_POINT ( 'NONE',  ( 23.16562500061451502, -6.054752690667223547, -1.112240025338166033E-15 ) ) ;
#57113 = CARTESIAN_POINT ( 'NONE',  ( 26.78437500061451360, -4.541064518000419881, 2.621784821874995952 ) ) ;
#57114 = CARTESIAN_POINT ( 'NONE',  ( -1.878215178124999163, 16.50312499938548427, 26.74683588394047007 ) ) ;
#57115 = CARTESIAN_POINT ( 'NONE',  ( -0.7368805616696194605, 9.859898480082234684, 25.82089837893477480 ) ) ;
#57116 = CARTESIAN_POINT ( 'NONE',  ( 7.059375000614518392, -4.541064518000417216, -2.621784821875001281 ) ) ;
#57117 = CARTESIAN_POINT ( 'NONE',  ( -1.626862140677534273E-15, 19.98124999877096641, 34.00000000000000000 ) ) ;
#57118 = CARTESIAN_POINT ( 'NONE',  ( 28.45312500061451289, 0.000000000000000000, 5.243569643749999010 ) ) ;
#57119 = CARTESIAN_POINT ( 'NONE',  ( 5.596875000614516260, -3.027376345333614438, 5.243569643749998122 ) ) ;
#57120 = CARTESIAN_POINT ( 'NONE',  ( 25.83749999999999503, 5.773502691896255534, 3.535250795749688401E-16 ) ) ;
#57121 = CARTESIAN_POINT ( 'NONE',  ( 26.67187500061451644, 3.027376345333611329, 5.243569643749999010 ) ) ;
#57122 = CARTESIAN_POINT ( 'NONE',  ( -4.243569643749999898, 9.865625000614596019, 27.54997392385601529 ) ) ;
#57123 = CARTESIAN_POINT ( 'NONE',  ( 16.05000000000000071, 0.000000000000000000, 4.999999999999998224 ) ) ;
#57124 = ORIENTED_EDGE ( 'NONE', *, *, #41575, .T. ) ;
#57125 = CARTESIAN_POINT ( 'NONE',  ( 28.31250000000000000, -5.773502691896255534, -1.060575238724906372E-15 ) ) ;
#57126 = CARTESIAN_POINT ( 'NONE',  ( 28.20937500061451786, -4.541064518000417216, -2.621784821875001281 ) ) ;
#57127 = ADVANCED_FACE ( 'NONE', ( #39661 ), #66266, .F. ) ;
#57128 = ORIENTED_EDGE ( 'NONE', *, *, #69433, .F. ) ;
#57129 = CARTESIAN_POINT ( 'NONE',  ( 15.77812500061451573, 4.541064518000418104, 2.621784821874999949 ) ) ;
#57130 = CARTESIAN_POINT ( 'NONE',  ( 6.628125000614517148, 6.421520780324663323E-16, -5.243569643749999010 ) ) ;
#57131 = CARTESIAN_POINT ( 'NONE',  ( 19.39687500061451786, 0.000000000000000000, 4.756430356249998326 ) ) ;
#57132 = CARTESIAN_POINT ( 'NONE',  ( 4.846875000614519813, -3.027376345333610441, -5.243569643749999898 ) ) ;
#57133 = EDGE_CURVE ( 'NONE', #52162, #24589, #63255, .T. ) ;
#57134 = CARTESIAN_POINT ( 'NONE',  ( 16.53750000122903430, 4.330127018922191873, 2.499999999999999556 ) ) ;
#57135 = CARTESIAN_POINT ( 'NONE',  ( 22.27499999999999858, 4.330127018922191873, 2.499999999999999556 ) ) ;
#57136 = CARTESIAN_POINT ( 'NONE',  ( 30.00000000000000000, 0.000000000000000000, 4.999999999999998224 ) ) ;
#57137 = CARTESIAN_POINT ( 'NONE',  ( 4.659375000614518925, 0.000000000000000000, 5.243569643749999010 ) ) ;
#57138 = CARTESIAN_POINT ( 'NONE',  ( 9.646875000614516082, -3.027376345333614438, 5.243569643749998122 ) ) ;
#57139 = CARTESIAN_POINT ( 'NONE',  ( 22.69687500061451857, -3.027376345333614438, 5.243569643749998122 ) ) ;
#57140 = CYLINDRICAL_SURFACE ( 'NONE', #33600, 3.999999999999996447 ) ;
#57141 = ORIENTED_EDGE ( 'NONE', *, *, #38471, .T. ) ;
#57142 = CARTESIAN_POINT ( 'NONE',  ( 3.084375000614519191, 6.421520780324663323E-16, -5.243569643749999010 ) ) ;
#57143 = CARTESIAN_POINT ( 'NONE',  ( 7.509375000614517681, -4.541064518000417216, -2.621784821875001281 ) ) ;
#57144 = CARTESIAN_POINT ( 'NONE',  ( 19.61249999999999716, 2.886751345948126879, 4.999999999999999112 ) ) ;
#57145 = CARTESIAN_POINT ( 'NONE',  ( 17.24062500061451786, -3.027376345333614438, 5.243569643749998122 ) ) ;
#57146 = CARTESIAN_POINT ( 'NONE',  ( -2.000000000000001776, 20.44999999999999929, 33.46410161513775705 ) ) ;
#57147 = CARTESIAN_POINT ( 'NONE',  ( 3.486133158594716510E-16, 19.88749999999999929, 26.00000000000000355 ) ) ;
#57148 = CARTESIAN_POINT ( 'NONE',  ( 19.09687500061451360, -2.746126346562646425, 4.756430356249996549 ) ) ;
#57149 = CARTESIAN_POINT ( 'NONE',  ( 11.16562500061451679, 3.027376345333613106, -5.243569643749998122 ) ) ;
#57150 = CARTESIAN_POINT ( 'NONE',  ( 27.45937500061451786, 4.541064518000418104, -2.621784821874998173 ) ) ;
#57151 = EDGE_CURVE ( 'NONE', #25696, #63910, #71481, .T. ) ;
#57152 = CYLINDRICAL_SURFACE ( 'NONE', #70239, 9.000000000000000000 ) ;
#57153 = CARTESIAN_POINT ( 'NONE',  ( 25.24687500061451573, 6.054752690667223547, 3.707466751127219781E-16 ) ) ;
#57154 = CARTESIAN_POINT ( 'NONE',  ( 7.237500000000000711, -2.886751345948125991, -5.000000000000000000 ) ) ;
#57155 = CARTESIAN_POINT ( 'NONE',  ( 2.000000000000001332, 13.96250000122903323, 33.46410161513774995 ) ) ;
#57156 = CARTESIAN_POINT ( 'NONE',  ( 6.337500001229033231, -4.330127018922194537, 2.499999999999995559 ) ) ;
#57157 = CARTESIAN_POINT ( 'NONE',  ( 18.38437500061451857, 6.421520780324663323E-16, -5.243569643749999010 ) ) ;
#57158 = CARTESIAN_POINT ( 'NONE',  ( 12.94687500061451857, -3.027376345333610441, -5.243569643749999898 ) ) ;
#57159 = CARTESIAN_POINT ( 'NONE',  ( 4.000000000000000000, 13.79374999877096641, 30.00000000000000000 ) ) ;
#57160 = ORIENTED_EDGE ( 'NONE', *, *, #60001, .T. ) ;
#57161 = CARTESIAN_POINT ( 'NONE',  ( 14.95312500061451644, 0.000000000000000000, 5.243569643749999010 ) ) ;
#57162 = CARTESIAN_POINT ( 'NONE',  ( 25.65000000122903145, -2.886751345948129988, 4.999999999999997335 ) ) ;
#57163 = CARTESIAN_POINT ( 'NONE',  ( 13.58437500061451786, 4.541064518000418104, 2.621784821874999949 ) ) ;
#57164 = CARTESIAN_POINT ( 'NONE',  ( 30.00000000000000000, 6.123233995736764310E-16, -4.999999999999998224 ) ) ;
#57165 = CARTESIAN_POINT ( 'NONE',  ( 14.80312500061451608, 4.541064518000418104, -2.621784821874998173 ) ) ;
#57166 = EDGE_CURVE ( 'NONE', #24963, #42547, #72990, .T. ) ;
#57167 = CARTESIAN_POINT ( 'NONE',  ( 26.51250000122903216, 0.000000000000000000, 4.999999999999998224 ) ) ;
#57168 = CARTESIAN_POINT ( 'NONE',  ( 27.42187500061451644, 3.027376345333613106, -5.243569643749998122 ) ) ;
#57169 = CARTESIAN_POINT ( 'NONE',  ( -2.121784821874996840, 10.42812500061451786, 33.67503911421598417 ) ) ;
#57170 = CARTESIAN_POINT ( 'NONE',  ( 12.48750000122903359, 4.330127018922191873, 2.499999999999999556 ) ) ;
#57171 = DIRECTION ( 'NONE',  ( 0.000000000000000000, 0.000000000000000000, 1.000000000000000000 ) ) ;
#57172 = DIRECTION ( 'NONE',  ( 0.000000000000000000, 0.000000000000000000, 1.000000000000000000 ) ) ;
#57173 = CARTESIAN_POINT ( 'NONE',  ( -4.243569643749998122, 17.19687500061451502, -27.54997392385601174 ) ) ;
#57174 = CARTESIAN_POINT ( 'NONE',  ( 18.60937500061451644, 0.000000000000000000, 5.243569643749999010 ) ) ;
#57175 = CARTESIAN_POINT ( 'NONE',  ( 19.80000000122903359, -2.886751345948129988, 4.999999999999997335 ) ) ;
#57176 = CARTESIAN_POINT ( 'NONE',  ( 13.95937500061451786, 4.541064518000418104, -2.621784821874998173 ) ) ;
#57177 = CARTESIAN_POINT ( 'NONE',  ( 4.243569643749999898, 10.59687500061451715, 32.45002607614398471 ) ) ;
#57178 = CARTESIAN_POINT ( 'NONE',  ( 21.71250000122903501, -4.330127018922190985, -2.500000000000001332 ) ) ;
#57179 = CARTESIAN_POINT ( 'NONE',  ( 14.99062500061451786, -3.027376345333614438, 5.243569643749998122 ) ) ;
#57180 = CARTESIAN_POINT ( 'NONE',  ( 5.810221930991193690E-16, 19.75624999877096499, 26.00000000000000000 ) ) ;
#57181 = ORIENTED_EDGE ( 'NONE', *, *, #13482, .T. ) ;
#57182 = ORIENTED_EDGE ( 'NONE', *, *, #25554, .T. ) ;
#57183 = VECTOR ( 'NONE', #66780, 1000.000000000000000 ) ;
#57184 = CARTESIAN_POINT ( 'NONE',  ( 17.43750000000000355, -2.886751345948129988, 4.999999999999997335 ) ) ;
#57185 = CYLINDRICAL_SURFACE ( 'NONE', #51512, 4.000000000000000000 ) ;
#57186 = CARTESIAN_POINT ( 'NONE',  ( 1.091159441285789677, 4.887044806266474417, 33.85802829779076717 ) ) ;
#57187 = CARTESIAN_POINT ( 'NONE',  ( 14.73750000122903359, 4.330127018922191873, 2.499999999999999556 ) ) ;
#57188 = CARTESIAN_POINT ( 'NONE',  ( 20.50312500061451715, -4.541064518000417216, -2.621784821875001281 ) ) ;
#57189 = CARTESIAN_POINT ( 'NONE',  ( 22.04062500061451502, 6.054752690667223547, 3.707466751127219781E-16 ) ) ;
#57190 = CARTESIAN_POINT ( 'NONE',  ( 2.840625000614518392, -3.027376345333614438, 5.243569643749998122 ) ) ;
#57191 = CARTESIAN_POINT ( 'NONE',  ( 27.18750000000000000, 5.773502691896255534, 3.535250795749688894E-16 ) ) ;
#57192 = CARTESIAN_POINT ( 'NONE',  ( 4.750527263192109828, 3.347582200546265430, 4.201817546140637738 ) ) ;
#57193 = CARTESIAN_POINT ( 'NONE',  ( 8.221875000614518925, 2.746126346562643317, 4.756430356249998326 ) ) ;
#57194 = DIRECTION ( 'NONE',  ( -1.000000000000000000, -0.000000000000000000, 0.000000000000000000 ) ) ;
#57195 = CARTESIAN_POINT ( 'NONE',  ( -2.000000000000000000, 11.93750000122903465, -33.46410161513775705 ) ) ;
#57196 = CARTESIAN_POINT ( 'NONE',  ( 4.243569643749999010, 16.52187500061451786, -32.45002607614398471 ) ) ;
#57197 = CARTESIAN_POINT ( 'NONE',  ( 6.975000001229032520, 2.886751345948129099, -4.999999999999998224 ) ) ;
#57198 = CARTESIAN_POINT ( 'NONE',  ( 9.525000000000002132, 6.123233995736764310E-16, -4.999999999999998224 ) ) ;
#57199 = CARTESIAN_POINT ( 'NONE',  ( 5.137500001229033941, 6.123233995736764310E-16, -4.999999999999998224 ) ) ;
#57200 = CARTESIAN_POINT ( 'NONE',  ( 10.24687500061451750, -3.027376345333610441, -5.243569643749999898 ) ) ;
#57201 = CARTESIAN_POINT ( 'NONE',  ( 23.66250000122903430, 4.330127018922192761, -2.499999999999997780 ) ) ;
#57202 = CARTESIAN_POINT ( 'NONE',  ( 3.531796677802674367, 3.539267187803308179, -3.868928841707397925 ) ) ;
#57203 = CARTESIAN_POINT ( 'NONE',  ( 28.04999999999999716, 4.330127018922192761, -2.499999999999997780 ) ) ;
#57204 = AXIS2_PLACEMENT_3D ( 'NONE', #19444, #47181, #19081 ) ;
#57205 = CARTESIAN_POINT ( 'NONE',  ( 24.43125000122903145, 6.123233995736764310E-16, -4.999999999999998224 ) ) ;
#57206 = CARTESIAN_POINT ( 'NONE',  ( 8.709375000614517859, 0.000000000000000000, 5.243569643749999010 ) ) ;
#57207 = CARTESIAN_POINT ( 'NONE',  ( 13.32187500061451502, -6.054752690667223547, -1.112240025338166033E-15 ) ) ;
#57208 = CARTESIAN_POINT ( 'NONE',  ( 45.00000000000000000, 0.000000000000000000, 0.000000000000000000 ) ) ;
#57209 = CARTESIAN_POINT ( 'NONE',  ( 7.537500000000002309, -2.886751345948129988, 4.999999999999997335 ) ) ;
#57210 = AXIS2_PLACEMENT_3D ( 'NONE', #45512, #28508, #22239 ) ;
#57211 = CARTESIAN_POINT ( 'NONE',  ( 4.243569643749999898, 16.42812500061459247, 30.00000000000000000 ) ) ;
#57212 = CARTESIAN_POINT ( 'NONE',  ( 22.28437500061451715, -4.541064518000419881, 2.621784821874995952 ) ) ;
#57213 = FACE_OUTER_BOUND ( 'NONE', #14120, .T. ) ;
#57214 = CARTESIAN_POINT ( 'NONE',  ( 25.87500000122903288, 2.886751345948129099, -4.999999999999998224 ) ) ;
#57215 = VECTOR ( 'NONE', #62776, 1000.000000000000000 ) ;
#57216 = CARTESIAN_POINT ( 'NONE',  ( 16.92187500061451644, 5.824947211148865298E-16, -4.756430356249998326 ) ) ;
#57217 = CARTESIAN_POINT ( 'NONE',  ( 22.94062500061451715, 6.054752690667223547, 3.707466751127219781E-16 ) ) ;
#57218 = CARTESIAN_POINT ( 'NONE',  ( 16.22812500061451857, 4.541064518000418104, 2.621784821874999949 ) ) ;
#57219 = CARTESIAN_POINT ( 'NONE',  ( 26.03437500061451360, 5.492252693125287522, 3.363034840372157021E-16 ) ) ;
#57220 = CARTESIAN_POINT ( 'NONE',  ( 12.49687500061451573, -3.027376345333610441, -5.243569643749999898 ) ) ;
#57221 = CARTESIAN_POINT ( 'NONE',  ( 28.57499999999999929, 4.330127018922191873, 2.499999999999999556 ) ) ;
#57222 = CARTESIAN_POINT ( 'NONE',  ( 24.67500000122903359, 2.886751345948126879, 4.999999999999999112 ) ) ;
#57223 = CARTESIAN_POINT ( 'NONE',  ( 11.93437500061451573, -4.541064518000419881, 2.621784821874995952 ) ) ;
#57224 = CARTESIAN_POINT ( 'NONE',  ( 29.44687500061451857, -3.027376345333614438, 5.243569643749998122 ) ) ;
#57225 = CARTESIAN_POINT ( 'NONE',  ( 2.971875000614517592, -6.054752690667223547, -1.112240025338166033E-15 ) ) ;
#57226 = CARTESIAN_POINT ( 'NONE',  ( 16.61250000122903359, 0.000000000000000000, 4.999999999999998224 ) ) ;
#57227 = CARTESIAN_POINT ( 'NONE',  ( 22.77187500061451786, -6.054752690667223547, -1.112240025338166033E-15 ) ) ;
#57228 = CARTESIAN_POINT ( 'NONE',  ( 13.24687500061451750, -3.027376345333614438, 5.243569643749998122 ) ) ;
#57229 = CARTESIAN_POINT ( 'NONE',  ( 3.756430356250000546, 18.19062499938548427, 27.83122392262697886 ) ) ;
#57230 = CARTESIAN_POINT ( 'NONE',  ( 25.46249999999999858, 2.886751345948126879, 4.999999999999999112 ) ) ;
#57231 = CARTESIAN_POINT ( 'NONE',  ( 3.999999999999998668, 13.36250000000000071, 32.30940107675850470 ) ) ;
#57232 = CARTESIAN_POINT ( 'NONE',  ( 27.19687500061451857, -2.746126346562646425, 4.756430356249996549 ) ) ;
#57233 = CARTESIAN_POINT ( 'NONE',  ( 18.10312500061451502, 0.000000000000000000, 5.243569643749999010 ) ) ;
#57234 = CARTESIAN_POINT ( 'NONE',  ( 5.812500000000001776, -5.773502691896255534, -1.060575238724906372E-15 ) ) ;
#57235 = EDGE_CURVE ( 'NONE', #45966, #31631, #17724, .T. ) ;
#57236 = CARTESIAN_POINT ( 'NONE',  ( 4.169580978743460342, 2.759455464706926708, 4.458747374224691029 ) ) ;
#57237 = CARTESIAN_POINT ( 'NONE',  ( 15.56250000000000000, 2.886751345948126879, 4.999999999999999112 ) ) ;
#57238 = CARTESIAN_POINT ( 'NONE',  ( -4.243569643749999898, 9.903125000614517504, 30.00000000000000000 ) ) ;
#57239 = CARTESIAN_POINT ( 'NONE',  ( 3.275492200589926739, -3.777717676570560901, -3.275492200590059078 ) ) ;
#57240 = CARTESIAN_POINT ( 'NONE',  ( 26.93437500061451573, 6.421520780324663323E-16, -5.243569643749999010 ) ) ;
#57241 = ORIENTED_EDGE ( 'NONE', *, *, #65744, .F. ) ;
#57242 = CARTESIAN_POINT ( 'NONE',  ( 22.41562500061451502, 3.027376345333613106, -5.243569643749998122 ) ) ;
#57243 = CARTESIAN_POINT ( 'NONE',  ( 20.14687500061451786, -3.027376345333610441, -5.243569643749999898 ) ) ;
#57244 = CARTESIAN_POINT ( 'NONE',  ( 3.900000000000000799, 0.000000000000000000, 4.999999999999998224 ) ) ;
#57245 = CARTESIAN_POINT ( 'NONE',  ( 8.203125000614518214, 0.000000000000000000, 5.243569643749999010 ) ) ;
#57246 = CARTESIAN_POINT ( 'NONE',  ( 25.19062500061451715, 6.054752690667223547, 3.707466751127219781E-16 ) ) ;
#57247 = CARTESIAN_POINT ( 'NONE',  ( 12.90937500061451537, -4.541064518000417216, -2.621784821875001281 ) ) ;
#57248 = CARTESIAN_POINT ( 'NONE',  ( 17.55937500061451573, 4.541064518000418104, -2.621784821874998173 ) ) ;
#57249 = CARTESIAN_POINT ( 'NONE',  ( -2.121784821874996840, 17.17812500061451786, 33.67503911421598417 ) ) ;
#57250 = CARTESIAN_POINT ( 'NONE',  ( 18.30000000122903359, 5.773502691896255534, 3.535250795749688894E-16 ) ) ;
#57251 = CARTESIAN_POINT ( 'NONE',  ( 14.55937500061451573, 0.000000000000000000, 4.756430356249998326 ) ) ;
#57252 = CARTESIAN_POINT ( 'NONE',  ( 10.34062500061451750, 6.054752690667223547, 3.707466751127219781E-16 ) ) ;
#57253 = CARTESIAN_POINT ( 'NONE',  ( 6.346875000614517148, 6.054752690667223547, 3.707466751127219781E-16 ) ) ;
#57254 = CARTESIAN_POINT ( 'NONE',  ( 4.359375000614517326, -4.541064518000417216, -2.621784821875001281 ) ) ;
#57255 = ORIENTED_EDGE ( 'NONE', *, *, #60575, .F. ) ;
#57256 = CARTESIAN_POINT ( 'NONE',  ( 25.84687500061451360, -3.027376345333614438, 5.243569643749998122 ) ) ;
#57257 = CARTESIAN_POINT ( 'NONE',  ( 16.30312500061451786, 0.000000000000000000, 5.243569643749999010 ) ) ;
#57258 = CARTESIAN_POINT ( 'NONE',  ( 28.38750000122903216, -4.330127018922194537, 2.499999999999995559 ) ) ;
#57259 = CARTESIAN_POINT ( 'NONE',  ( 26.95312500061451644, 4.541064518000418104, -2.621784821874998173 ) ) ;
#57260 = CARTESIAN_POINT ( 'NONE',  ( 21.90937500061451715, -4.541064518000417216, -2.621784821875001281 ) ) ;
#57261 = CARTESIAN_POINT ( 'NONE',  ( 16.52812500061451573, 6.421520780324663323E-16, -5.243569643749999010 ) ) ;
#57262 = CARTESIAN_POINT ( 'NONE',  ( -4.243569643749999898, 18.05937500061451928, 30.00000000000000000 ) ) ;
#57263 = VECTOR ( 'NONE', #59413, 1000.000000000000000 ) ;
#57264 = CARTESIAN_POINT ( 'NONE',  ( 21.96562500061451573, 3.027376345333613106, -5.243569643749998122 ) ) ;
#57265 = CARTESIAN_POINT ( 'NONE',  ( 3.225000001229033408, -5.773502691896255534, -1.060575238724906372E-15 ) ) ;
#57266 = VERTEX_POINT ( 'NONE', #11930 ) ;
#57267 = CARTESIAN_POINT ( 'NONE',  ( 25.64999999999999858, -4.330127018922190985, -2.500000000000001332 ) ) ;
#57268 = CARTESIAN_POINT ( 'NONE',  ( 2.000000000000001332, 13.85000000000000142, -26.53589838486224650 ) ) ;
#57269 = CARTESIAN_POINT ( 'NONE',  ( -1.878215178125001827, 20.25312499938548072, 33.25316411605952283 ) ) ;
#57270 = PRESENTATION_LAYER_ASSIGNMENT (  '', '', ( #13656 ) ) ;
#57271 = CARTESIAN_POINT ( 'NONE',  ( 2.934375000614518392, -4.541064518000419881, 2.621784821874995952 ) ) ;
#57272 = CARTESIAN_POINT ( 'NONE',  ( 10.82812500061451644, 4.541064518000418104, 2.621784821874999949 ) ) ;
#57273 = CARTESIAN_POINT ( 'NONE',  ( 21.67500000122903359, -5.773502691896255534, -1.060575238724906372E-15 ) ) ;
#57274 = VECTOR ( 'NONE', #44374, 1000.000000000000000 ) ;
#57275 = EDGE_CURVE ( 'NONE', #6802, #3090, #55077, .T. ) ;
#57276 = CARTESIAN_POINT ( 'NONE',  ( 27.02812500061451573, 4.541064518000418104, 2.621784821874999949 ) ) ;
#57277 = CARTESIAN_POINT ( 'NONE',  ( 26.88749999999999574, -2.886751345948129988, 4.999999999999997335 ) ) ;
#57278 = CARTESIAN_POINT ( 'NONE',  ( -3.999999999999999112, 17.41250000122903430, -30.00000000000000000 ) ) ;
#57279 = CARTESIAN_POINT ( 'NONE',  ( -2.000000000000000000, 12.38750000122903394, 26.53589838486224650 ) ) ;
#57280 = CARTESIAN_POINT ( 'NONE',  ( 9.703125000614514661, -4.541064518000417216, -2.621784821875001281 ) ) ;
#57281 =( BOUNDED_CURVE ( )  B_SPLINE_CURVE ( 2, ( #68417, #57677, #23336, #58031, #29967, #63224, #18508 ),
 .UNSPECIFIED., .F., .F. ) 
 B_SPLINE_CURVE_WITH_KNOTS ( ( 3, 2, 2, 3 ),
 ( 0.7083333333333334814, 0.7111111111111112493, 0.7138888888888890172, 0.7166666666666667851 ),
 .UNSPECIFIED. ) 
 CURVE ( )  GEOMETRIC_REPRESENTATION_ITEM ( )  RATIONAL_B_SPLINE_CURVE ( ( 0.9999999999999946709, 0.8660254037844440367, 1.000000000000000000, 0.8660254037844387076, 1.000000000000000000, 0.8660254037844333785, 1.000000000000005329 ) ) 
 REPRESENTATION_ITEM ( '' )  );
#57282 = ORIENTED_EDGE ( 'NONE', *, *, #7045, .T. ) ;
#57283 = VECTOR ( 'NONE', #43847, 1000.000000000000000 ) ;
#57284 = CARTESIAN_POINT ( 'NONE',  ( 7.790625000614518569, -3.027376345333614438, 5.243569643749998122 ) ) ;
#57285 = UNCERTAINTY_MEASURE_WITH_UNIT (LENGTH_MEASURE( 1.000000000000000082E-05 ), #53357, 'distance_accuracy_value', 'NONE');
#57286 = VECTOR ( 'NONE', #22969, 1000.000000000000000 ) ;
#57287 = CARTESIAN_POINT ( 'NONE',  ( 5.315625000614516260, 3.027376345333613106, -5.243569643749998122 ) ) ;
#57288 = CARTESIAN_POINT ( 'NONE',  ( 16.65937500061452070, 4.119189519843966529, -2.378215178124998275 ) ) ;
#57289 = EDGE_CURVE ( 'NONE', #50879, #30796, #33632, .T. ) ;
#57290 = DIRECTION ( 'NONE',  ( -0.000000000000000000, -1.000000000000000000, -0.000000000000000000 ) ) ;
#57291 = CARTESIAN_POINT ( 'NONE',  ( 14.43750000000000000, -2.886751345948125991, -5.000000000000000000 ) ) ;
#57292 = CARTESIAN_POINT ( 'NONE',  ( 15.49687500061451750, -3.027376345333614438, 5.243569643749998122 ) ) ;
#57293 = CARTESIAN_POINT ( 'NONE',  ( 10.16250000122903252, 4.330127018922192761, -2.499999999999997780 ) ) ;
#57294 = CARTESIAN_POINT ( 'NONE',  ( 20.33437500061451786, 4.541064518000418104, 2.621784821874999949 ) ) ;
#57295 = CARTESIAN_POINT ( 'NONE',  ( 17.21249999999999858, 2.886751345948129099, -4.999999999999998224 ) ) ;
#57296 = CARTESIAN_POINT ( 'NONE',  ( 20.40937500061451715, 0.000000000000000000, 5.243569643749999010 ) ) ;
#57297 = CARTESIAN_POINT ( 'NONE',  ( -4.243569643749999898, 13.95312500061451821, -30.00000000000000000 ) ) ;
#57298 = CARTESIAN_POINT ( 'NONE',  ( -3.999999999999999112, 16.81250000000000000, 27.69059892324149885 ) ) ;
#57299 = CARTESIAN_POINT ( 'NONE',  ( 23.40937500061451360, 2.746126346562643317, 4.756430356249998326 ) ) ;
#57300 = CARTESIAN_POINT ( 'NONE',  ( -1.626862140677534273E-15, 15.03124999877096535, 34.00000000000000000 ) ) ;
#57301 = CARTESIAN_POINT ( 'NONE',  ( 24.70312500061451644, 4.541064518000418104, -2.621784821874998173 ) ) ;
#57302 = CARTESIAN_POINT ( 'NONE',  ( 24.82499999999999929, 6.123233995736764310E-16, -4.999999999999998224 ) ) ;
#57303 = CARTESIAN_POINT ( 'NONE',  ( 27.72187500061451715, -6.054752690667223547, -1.112240025338166033E-15 ) ) ;
#57304 = CARTESIAN_POINT ( 'NONE',  ( 23.13749999999999929, 5.773502691896255534, 3.535250795749688894E-16 ) ) ;
#57305 = CARTESIAN_POINT ( 'NONE',  ( 8.015625000614518214, 3.027376345333613106, -5.243569643749998122 ) ) ;
#57306 = CARTESIAN_POINT ( 'NONE',  ( 25.28437500061451360, -2.746126346562646425, 4.756430356249996549 ) ) ;
#57307 = CARTESIAN_POINT ( 'NONE',  ( 19.58437500061451786, -4.541064518000419881, 2.621784821874995952 ) ) ;
#57308 = CARTESIAN_POINT ( 'NONE',  ( 10.58437500061451608, -2.746126346562641984, -4.756430356249999214 ) ) ;
#57309 = VECTOR ( 'NONE', #20094, 1000.000000000000000 ) ;
#57310 = CARTESIAN_POINT ( 'NONE',  ( 4.565625000614516260, 3.027376345333611329, 5.243569643749999010 ) ) ;
#57311 = CARTESIAN_POINT ( 'NONE',  ( 8.784375000614518925, -4.541064518000419881, 2.621784821874995952 ) ) ;
#57312 = ORIENTED_EDGE ( 'NONE', *, *, #32388, .F. ) ;
#57313 = CARTESIAN_POINT ( 'NONE',  ( 19.58437500061451786, -4.541064518000419881, 2.621784821874995952 ) ) ;
#57314 = CARTESIAN_POINT ( 'NONE',  ( 13.83750000122903323, 4.330127018922191873, 2.499999999999999556 ) ) ;
#57315 = CARTESIAN_POINT ( 'NONE',  ( 29.39999999999999858, 4.330127018922192761, -2.499999999999997780 ) ) ;
#57316 = CARTESIAN_POINT ( 'NONE',  ( 3.450000000000001510, 0.000000000000000000, 4.999999999999998224 ) ) ;
#57317 = CARTESIAN_POINT ( 'NONE',  ( 1.071796769724488785, 15.55759618943233491, 34.00000000000000000 ) ) ;
#57318 = CARTESIAN_POINT ( 'NONE',  ( 27.82499999999999929, -4.330127018922194537, 2.499999999999995559 ) ) ;
#57319 = ORIENTED_EDGE ( 'NONE', *, *, #55505, .T. ) ;
#57320 = CARTESIAN_POINT ( 'NONE',  ( 9.562500000000001776, 2.886751345948129099, -4.999999999999998224 ) ) ;
#57321 = CARTESIAN_POINT ( 'NONE',  ( 10.95937500061451431, -5.492252693125287522, -1.008910452111647106E-15 ) ) ;
#57322 = CARTESIAN_POINT ( 'NONE',  ( 23.65312500061451573, -4.541064518000417216, -2.621784821875001281 ) ) ;
#57323 = CARTESIAN_POINT ( 'NONE',  ( 13.76250000000000107, 2.886751345948126879, 4.999999999999999112 ) ) ;
#57324 = CARTESIAN_POINT ( 'NONE',  ( 11.36250000122903536, -4.330127018922190985, -2.500000000000001332 ) ) ;
#57325 = CARTESIAN_POINT ( 'NONE',  ( 9.328125000614518214, 6.421520780324663323E-16, -5.243569643749999010 ) ) ;
#57326 = CARTESIAN_POINT ( 'NONE',  ( 23.17500000000000071, 4.330127018922191873, 2.499999999999999556 ) ) ;
#57327 = CARTESIAN_POINT ( 'NONE',  ( 21.32812500061451644, -4.541064518000419881, 2.621784821874995952 ) ) ;
#57328 = CARTESIAN_POINT ( 'NONE',  ( 18.78750000122903430, 4.330127018922191873, 2.499999999999999556 ) ) ;
#57329 = CARTESIAN_POINT ( 'NONE',  ( 27.52500000122903145, -5.773502691896255534, -1.060575238724906372E-15 ) ) ;
#57330 = CARTESIAN_POINT ( 'NONE',  ( -1.878215178124999163, 17.29062499938548214, 26.74683588394047007 ) ) ;
#57331 = CARTESIAN_POINT ( 'NONE',  ( 6.487499999999999822, 5.773502691896255534, 3.535250795749688894E-16 ) ) ;
#57332 = ORIENTED_EDGE ( 'NONE', *, *, #32403, .T. ) ;
#57333 = CARTESIAN_POINT ( 'NONE',  ( 23.01562500061451644, 3.027376345333611329, 5.243569643749999010 ) ) ;
#57334 = CARTESIAN_POINT ( 'NONE',  ( 28.04062500061451502, -3.027376345333614438, 5.243569643749998122 ) ) ;
#57335 = CARTESIAN_POINT ( 'NONE',  ( 28.35937500061451289, 4.541064518000418104, -2.621784821874998173 ) ) ;
#57336 = CARTESIAN_POINT ( 'NONE',  ( 18.79687500061451644, -3.027376345333610441, -5.243569643749999898 ) ) ;
#57337 = CARTESIAN_POINT ( 'NONE',  ( 13.30312500061451786, -4.541064518000417216, -2.621784821875001281 ) ) ;
#57338 = CARTESIAN_POINT ( 'NONE',  ( 4.111889464957033447, 2.844708250062874644, 4.404844785106587501 ) ) ;
#57339 = CARTESIAN_POINT ( 'NONE',  ( 27.11250000122903359, -4.330127018922190985, -2.500000000000001332 ) ) ;
#57340 = CARTESIAN_POINT ( 'NONE',  ( 22.17187500061451644, 2.746126346562643317, 4.756430356249998326 ) ) ;
#57341 = CARTESIAN_POINT ( 'NONE',  ( 16.71562500061451573, 3.027376345333611329, 5.243569643749999010 ) ) ;
#57342 = CARTESIAN_POINT ( 'NONE',  ( 3.787500001229033408, 6.123233995736764310E-16, -4.999999999999998224 ) ) ;
#57343 = CARTESIAN_POINT ( 'NONE',  ( 12.98437500061451821, 6.421520780324663323E-16, -5.243569643749999010 ) ) ;
#57344 = CARTESIAN_POINT ( 'NONE',  ( 12.00937500061451857, -4.541064518000417216, -2.621784821875001281 ) ) ;
#57345 = CARTESIAN_POINT ( 'NONE',  ( 20.03437500061451715, -4.541064518000419881, 2.621784821874995952 ) ) ;
#57346 = VERTEX_POINT ( 'NONE', #31093 ) ;
#57347 = CARTESIAN_POINT ( 'NONE',  ( -4.761366016028759418, 8.797204459235659968, 33.67116182595535889 ) ) ;
#57348 = CARTESIAN_POINT ( 'NONE',  ( 23.80312500061451786, 4.541064518000418104, -2.621784821874998173 ) ) ;
#57349 = CARTESIAN_POINT ( 'NONE',  ( 19.62187500061451573, -6.054752690667223547, -1.112240025338166033E-15 ) ) ;
#57350 = CARTESIAN_POINT ( 'NONE',  ( 23.84062500061451928, 6.054752690667223547, 3.707466751127219781E-16 ) ) ;
#57351 = CARTESIAN_POINT ( 'NONE',  ( 27.29999999999999716, 0.000000000000000000, 4.999999999999998224 ) ) ;
#57352 = CARTESIAN_POINT ( 'NONE',  ( 8.484601909799253346E-16, 17.86250000000000071, 34.61880215351700230 ) ) ;
#57353 = CARTESIAN_POINT ( 'NONE',  ( 3.196875000614516793, 6.054752690667223547, 3.707466751127219781E-16 ) ) ;
#57354 = CARTESIAN_POINT ( 'NONE',  ( 10.31250000122903288, 0.000000000000000000, 4.999999999999998224 ) ) ;
#57355 = CARTESIAN_POINT ( 'NONE',  ( 7.200000001229035718, -2.886751345948129988, 4.999999999999997335 ) ) ;
#57356 = CARTESIAN_POINT ( 'NONE',  ( 26.28750000122903430, 6.123233995736764310E-16, -4.999999999999998224 ) ) ;
#57357 = CARTESIAN_POINT ( 'NONE',  ( 4.000000000000000000, 19.64374999877096428, 30.00000000000000000 ) ) ;
#57358 = CARTESIAN_POINT ( 'NONE',  ( 15.88125000122903074, 6.123233995736764310E-16, -4.999999999999998224 ) ) ;
#57359 = CARTESIAN_POINT ( 'NONE',  ( 8.559375000614515727, 4.541064518000418104, -2.621784821874998173 ) ) ;
#57360 = CARTESIAN_POINT ( 'NONE',  ( 9.525000000000002132, 6.123233995736764310E-16, -4.999999999999998224 ) ) ;
#57361 = CARTESIAN_POINT ( 'NONE',  ( 18.40312500061451573, 4.541064518000418104, -2.621784821874998173 ) ) ;
#57362 = CARTESIAN_POINT ( 'NONE',  ( 11.59687500061451892, -3.027376345333610441, -5.243569643749999898 ) ) ;
#57363 = CARTESIAN_POINT ( 'NONE',  ( 28.38750000122903216, -4.330127018922194537, 2.499999999999995559 ) ) ;
#57364 = CARTESIAN_POINT ( 'NONE',  ( 19.65937500061451360, -4.541064518000417216, -2.621784821875001281 ) ) ;
#57365 = CARTESIAN_POINT ( 'NONE',  ( 8.146875000614516082, 6.054752690667223547, 3.707466751127219781E-16 ) ) ;
#57366 = CARTESIAN_POINT ( 'NONE',  ( 14.96250000122903323, -4.330127018922190985, -2.500000000000001332 ) ) ;
#57367 = CARTESIAN_POINT ( 'NONE',  ( 10.72500000000000142, -4.330127018922194537, 2.499999999999995559 ) ) ;
#57368 = CARTESIAN_POINT ( 'NONE',  ( 7.790625000614518569, -3.027376345333614438, 5.243569643749998122 ) ) ;
#57369 = CARTESIAN_POINT ( 'NONE',  ( 18.32812500061451644, 6.421520780324663323E-16, -5.243569643749999010 ) ) ;
#57370 = VERTEX_POINT ( 'NONE', #19258 ) ;
#57371 = CARTESIAN_POINT ( 'NONE',  ( 5.775000001229033231, 2.886751345948126879, 4.999999999999999112 ) ) ;
#57372 = CARTESIAN_POINT ( 'NONE',  ( 14.12812500061451715, -4.541064518000419881, 2.621784821874995952 ) ) ;
#57373 = CIRCLE ( 'NONE', #37333, 4.000000000000000000 ) ;
#57374 = CARTESIAN_POINT ( 'NONE',  ( 12.59062500061451573, 6.054752690667223547, 3.707466751127219781E-16 ) ) ;
#57375 = CARTESIAN_POINT ( 'NONE',  ( 23.22187500061451715, -5.492252693125287522, -1.008910452111647106E-15 ) ) ;
#57376 = CARTESIAN_POINT ( 'NONE',  ( 14.06250000000000000, 2.886751345948129099, -4.999999999999998224 ) ) ;
#57377 = CARTESIAN_POINT ( 'NONE',  ( 7.987500001229032698, 4.330127018922191873, 2.499999999999999556 ) ) ;
#57378 = CARTESIAN_POINT ( 'NONE',  ( 4.790625000614518569, -3.027376345333610441, -5.243569643749999898 ) ) ;
#57379 = CARTESIAN_POINT ( 'NONE',  ( 17.88750000122903216, 4.330127018922191873, 2.499999999999999556 ) ) ;
#57380 = CARTESIAN_POINT ( 'NONE',  ( 25.57499999999999929, -4.330127018922194537, 2.499999999999995559 ) ) ;
#57381 = CARTESIAN_POINT ( 'NONE',  ( -3.000416591977282496E-16, 10.74687500061451928, -34.90005215228797653 ) ) ;
#57382 = DIRECTION ( 'NONE',  ( -1.000000000000000000, -0.000000000000000000, -0.000000000000000000 ) ) ;
#57383 = CARTESIAN_POINT ( 'NONE',  ( 2.737500001229034474, -4.330127018922194537, 2.499999999999995559 ) ) ;
#57384 = CARTESIAN_POINT ( 'NONE',  ( -1.999999999999997113, 11.52500000000000036, -26.53589838486224295 ) ) ;
#57385 = CARTESIAN_POINT ( 'NONE',  ( -1.071796769724488563, 13.34240381056766545, 34.00000000000000000 ) ) ;
#57386 = CARTESIAN_POINT ( 'NONE',  ( 19.20937500061451786, -4.541064518000417216, -2.621784821875001281 ) ) ;
#57387 = CARTESIAN_POINT ( 'NONE',  ( -3.999999999999997335, 16.55000000122903359, 32.30940107675850470 ) ) ;
#57388 = CARTESIAN_POINT ( 'NONE',  ( 14.09062500061451750, -3.027376345333614438, 5.243569643749998122 ) ) ;
#57389 = CARTESIAN_POINT ( 'NONE',  ( 10.25625000122903252, 0.000000000000000000, 4.999999999999998224 ) ) ;
#57390 = CARTESIAN_POINT ( 'NONE',  ( 13.12500000000000178, 6.123233995736764310E-16, -4.999999999999998224 ) ) ;
#57391 = CARTESIAN_POINT ( 'NONE',  ( 27.27187500061451431, -6.054752690667223547, -1.112240025338166033E-15 ) ) ;
#57392 = CARTESIAN_POINT ( 'NONE',  ( 17.40937500061451360, 2.746126346562645981, -4.756430356249997438 ) ) ;
#57393 = CARTESIAN_POINT ( 'NONE',  ( 12.36562500061451608, -6.054752690667223547, -1.112240025338166033E-15 ) ) ;
#57394 = CARTESIAN_POINT ( 'NONE',  ( 11.52187500061451608, -6.054752690667223547, -1.112240025338166033E-15 ) ) ;
#57395 = ORIENTED_EDGE ( 'NONE', *, *, #21641, .T. ) ;
#57396 = AXIS2_PLACEMENT_3D ( 'NONE', #49267, #32632, #66994 ) ;
#57397 = CARTESIAN_POINT ( 'NONE',  ( 29.16562500061451502, 3.027376345333613106, -5.243569643749998122 ) ) ;
#57398 = CARTESIAN_POINT ( 'NONE',  ( 20.12812500061451715, 6.421520780324663323E-16, -5.243569643749999010 ) ) ;
#57399 = CARTESIAN_POINT ( 'NONE',  ( 29.31562500061451715, 3.027376345333611329, 5.243569643749999010 ) ) ;
#57400 = CARTESIAN_POINT ( 'NONE',  ( 10.78125000122903288, -4.330127018922194537, 2.499999999999995559 ) ) ;
#57401 = EDGE_CURVE ( 'NONE', #51638, #30066, #70596, .T. ) ;
#57402 = CARTESIAN_POINT ( 'NONE',  ( 9.862500000000000711, -5.773502691896255534, -1.060575238724906372E-15 ) ) ;
#57403 = CARTESIAN_POINT ( 'NONE',  ( 19.35000000122903430, -2.886751345948129988, 4.999999999999997335 ) ) ;
#57404 = CARTESIAN_POINT ( 'NONE',  ( -1.389181105737270716, 10.01354714573257532, 26.18324193183354964 ) ) ;
#57405 = CARTESIAN_POINT ( 'NONE',  ( 9.534375000614517148, -2.746126346562646425, 4.756430356249996549 ) ) ;
#57406 = ORIENTED_EDGE ( 'NONE', *, *, #17867, .F. ) ;
#57407 = CARTESIAN_POINT ( 'NONE',  ( 17.77499999999999858, 4.330127018922191873, 2.499999999999999556 ) ) ;
#57408 = CARTESIAN_POINT ( 'NONE',  ( 20.58750000000000213, -2.886751345948129988, 4.999999999999997335 ) ) ;
#57409 = CARTESIAN_POINT ( 'NONE',  ( 18.64687500061451786, -3.027376345333614438, 5.243569643749998122 ) ) ;
#57410 = CARTESIAN_POINT ( 'NONE',  ( 24.74062500061451786, 6.054752690667223547, 3.707466751127219781E-16 ) ) ;
#57411 = EDGE_CURVE ( 'NONE', #46843, #13938, #39973, .T. ) ;
#57412 = ORIENTED_EDGE ( 'NONE', *, *, #3406, .T. ) ;
#57413 = CARTESIAN_POINT ( 'NONE',  ( 8.353125000614518569, -4.541064518000417216, -2.621784821875001281 ) ) ;
#57414 = CARTESIAN_POINT ( 'NONE',  ( -2.000000000000001776, 19.04374999877096641, 33.46410161513775705 ) ) ;
#57415 = VECTOR ( 'NONE', #44337, 1000.000000000000000 ) ;
#57416 = CARTESIAN_POINT ( 'NONE',  ( 13.79999999999999893, 0.000000000000000000, 4.999999999999998224 ) ) ;
#57417 = CARTESIAN_POINT ( 'NONE',  ( -4.243569643749999898, 17.51562500061451644, 27.54997392385601529 ) ) ;
#57418 = CARTESIAN_POINT ( 'NONE',  ( 3.121875000614518836, 3.027376345333613106, -5.243569643749998122 ) ) ;
#57419 = CARTESIAN_POINT ( 'NONE',  ( 10.61250000000000071, 2.886751345948126879, 4.999999999999999112 ) ) ;
#57420 = CARTESIAN_POINT ( 'NONE',  ( 2.655984681222220721E-16, 15.45312499938548179, 25.66244784525396483 ) ) ;
#57421 = CARTESIAN_POINT ( 'NONE',  ( 25.43437500061451573, -4.541064518000419881, 2.621784821874995952 ) ) ;
#57422 = VERTEX_POINT ( 'NONE', #37372 ) ;
#57423 = CARTESIAN_POINT ( 'NONE',  ( 22.00312500061451360, 4.541064518000418104, -2.621784821874998173 ) ) ;
#57424 = CARTESIAN_POINT ( 'NONE',  ( 23.67187500061451999, -6.054752690667223547, -1.112240025338166033E-15 ) ) ;
#57425 = CARTESIAN_POINT ( 'NONE',  ( 2.121784821875001281, 17.25312500061459176, -26.32496088578401938 ) ) ;
#57426 = CARTESIAN_POINT ( 'NONE',  ( 10.53750000000000320, 5.773502691896255534, 3.535250795749688894E-16 ) ) ;
#57427 = CARTESIAN_POINT ( 'NONE',  ( 7.940625000614518036, -3.027376345333610441, -5.243569643749999898 ) ) ;
#57428 = CARTESIAN_POINT ( 'NONE',  ( 29.48437500061451644, -4.119189519843968306, 2.378215178124996054 ) ) ;
#57429 = CARTESIAN_POINT ( 'NONE',  ( 23.35312500061451857, 4.541064518000418104, -2.621784821874998173 ) ) ;
#57430 = CARTESIAN_POINT ( 'NONE',  ( 27.08437500061451431, -2.746126346562646425, 4.756430356249996549 ) ) ;
#57431 = CARTESIAN_POINT ( 'NONE',  ( 12.34687500061452070, -2.746126346562646425, 4.756430356249996549 ) ) ;
#57432 = CARTESIAN_POINT ( 'NONE',  ( 20.63437500061451857, 6.421520780324663323E-16, -5.243569643749999010 ) ) ;
#57434 = CARTESIAN_POINT ( 'NONE',  ( -2.121784821874999949, 13.03437500061451715, 26.32496088578401938 ) ) ;
#57433 =( BOUNDED_CURVE ( )  B_SPLINE_CURVE ( 2, ( #68850, #7505, #40778, #35221, #57742, #24493, #52937 ),
 .UNSPECIFIED., .F., .F. ) 
 B_SPLINE_CURVE_WITH_KNOTS ( ( 3, 2, 2, 3 ),
 ( 0.7399999999999999911, 0.7433333333333332904, 0.7466666666666667007, 0.7500000000000000000 ),
 .UNSPECIFIED. ) 
 CURVE ( )  GEOMETRIC_REPRESENTATION_ITEM ( )  RATIONAL_B_SPLINE_CURVE ( ( 1.000000000000000000, 0.8660254037844387076, 1.000000000000000000, 0.8660254037844387076, 1.000000000000000000, 0.8660254037844387076, 1.000000000000000000 ) ) 
 REPRESENTATION_ITEM ( '' )  );
#57435 = CARTESIAN_POINT ( 'NONE',  ( 18.53437500061451715, 4.541064518000418104, 2.621784821874999949 ) ) ;
#57436 = CARTESIAN_POINT ( 'NONE',  ( 27.19687500061451857, -3.027376345333614438, 5.243569643749998122 ) ) ;
#57437 = CARTESIAN_POINT ( 'NONE',  ( 4.243569643749999898, 17.79687500061451999, 32.45002607614398471 ) ) ;
#57438 = CARTESIAN_POINT ( 'NONE',  ( 8.090625000614515727, 6.054752690667223547, 3.707466751127219781E-16 ) ) ;
#57439 = LINE ( 'NONE', #6842, #17108 ) ;
#57440 = CARTESIAN_POINT ( 'NONE',  ( 4.734375000614518214, -4.541064518000419881, 2.621784821874995952 ) ) ;
#57441 = FACE_OUTER_BOUND ( 'NONE', #36696, .T. ) ;
#57442 = CARTESIAN_POINT ( 'NONE',  ( 6.290625000614517681, 6.054752690667223547, 3.707466751127219781E-16 ) ) ;
#57443 = CARTESIAN_POINT ( 'NONE',  ( 9.084375000614517859, 4.541064518000418104, 2.621784821874999949 ) ) ;
#57444 = CARTESIAN_POINT ( 'NONE',  ( 16.27500000122903501, -5.773502691896255534, -1.060575238724906372E-15 ) ) ;
#57445 = CARTESIAN_POINT ( 'NONE',  ( 5.334375000614517859, 6.421520780324663323E-16, -5.243569643749999010 ) ) ;
#57446 = CARTESIAN_POINT ( 'NONE',  ( 8.315625000614515372, -6.054752690667223547, -1.112240025338166033E-15 ) ) ;
#57447 = CARTESIAN_POINT ( 'NONE',  ( 4.940625000614516260, 6.054752690667223547, 3.707466751127219781E-16 ) ) ;
#57448 = CARTESIAN_POINT ( 'NONE',  ( 23.71875000122903288, 2.886751345948126879, 4.999999999999999112 ) ) ;
#57449 = CARTESIAN_POINT ( 'NONE',  ( 17.40937500061451715, -4.541064518000417216, -2.621784821875001281 ) ) ;
#57450 = CARTESIAN_POINT ( 'NONE',  ( 22.80000000000000071, 0.000000000000000000, 4.999999999999998224 ) ) ;
#57451 = VERTEX_POINT ( 'NONE', #54009 ) ;
#57452 = CARTESIAN_POINT ( 'NONE',  ( 25.71562500061451573, 3.027376345333611329, 5.243569643749999010 ) ) ;
#57453 = CARTESIAN_POINT ( 'NONE',  ( 9.853125000614516793, 4.541064518000418104, -2.621784821874998173 ) ) ;
#57454 = CARTESIAN_POINT ( 'NONE',  ( 26.48437500061451644, 6.421520780324663323E-16, -5.243569643749999010 ) ) ;
#57455 = CARTESIAN_POINT ( 'NONE',  ( 9.778125000614517504, 6.421520780324663323E-16, -5.243569643749999010 ) ) ;
#57456 = CARTESIAN_POINT ( 'NONE',  ( 4.243569643749999898, 10.59687500061451715, -27.54997392385601529 ) ) ;
#57457 = CARTESIAN_POINT ( 'NONE',  ( 10.31250000122903288, 0.000000000000000000, 4.999999999999998224 ) ) ;
#57458 = CARTESIAN_POINT ( 'NONE',  ( 26.20312500061451644, 0.000000000000000000, 5.243569643749999010 ) ) ;
#57459 = CARTESIAN_POINT ( 'NONE',  ( -2.121784821874996840, 12.22812500061451857, -26.32496088578401583 ) ) ;
#57460 = CARTESIAN_POINT ( 'NONE',  ( 12.30000000122903181, -2.886751345948125991, -5.000000000000000000 ) ) ;
#57461 = CARTESIAN_POINT ( 'NONE',  ( 22.75312500061451360, -4.541064518000417216, -2.621784821875001281 ) ) ;
#57462 = CARTESIAN_POINT ( 'NONE',  ( 11.88749999999999751, 5.773502691896255534, 3.535250795749688894E-16 ) ) ;
#57463 = CARTESIAN_POINT ( 'NONE',  ( 19.90312500061451573, 0.000000000000000000, 5.243569643749999010 ) ) ;
#57464 = CARTESIAN_POINT ( 'NONE',  ( 6.421875000614519102, 3.027376345333611329, 5.243569643749999010 ) ) ;
#57465 = CARTESIAN_POINT ( 'NONE',  ( 21.11249999999999716, -5.773502691896255534, -1.060575238724906372E-15 ) ) ;
#57466 = CARTESIAN_POINT ( 'NONE',  ( 7.125000001229033764, 2.886751345948126879, 4.999999999999999112 ) ) ;
#57467 = CARTESIAN_POINT ( 'NONE',  ( 15.22500000122903252, 2.886751345948126879, 4.999999999999999112 ) ) ;
#57468 = AXIS2_PLACEMENT_3D ( 'NONE', #62883, #56278, #40733 ) ;
#57469 = CARTESIAN_POINT ( 'NONE',  ( 13.49062500061451608, 6.054752690667223547, 3.707466751127219781E-16 ) ) ;
#57470 = CARTESIAN_POINT ( 'NONE',  ( 15.06562500061451537, -6.054752690667223547, -1.112240025338166033E-15 ) ) ;
#57471 = CARTESIAN_POINT ( 'NONE',  ( 26.43750000122903288, 4.330127018922191873, 2.499999999999999556 ) ) ;
#57472 = CARTESIAN_POINT ( 'NONE',  ( 20.10000000000000142, 0.000000000000000000, 4.999999999999998224 ) ) ;
#57473 = CARTESIAN_POINT ( 'NONE',  ( 22.92187500061451644, 3.027376345333613106, -5.243569643749998122 ) ) ;
#57474 = CARTESIAN_POINT ( 'NONE',  ( 45.00000000000000000, -2.499999999999999556, 3.499999999999999556 ) ) ;
#57475 = CARTESIAN_POINT ( 'NONE',  ( 10.50000000122903465, -2.886751345948125991, -5.000000000000000000 ) ) ;
#57476 = CARTESIAN_POINT ( 'NONE',  ( 7.846875000614518036, -3.027376345333614438, 5.243569643749998122 ) ) ;
#57477 = CARTESIAN_POINT ( 'NONE',  ( 26.63437500061451857, 4.541064518000418104, 2.621784821874999949 ) ) ;
#57478 =( BOUNDED_CURVE ( )  B_SPLINE_CURVE ( 2, ( #43363, #32997, #55536, #49997, #72522, #21910, #5289, #27834, #50366 ),
 .UNSPECIFIED., .F., .F. ) 
 B_SPLINE_CURVE_WITH_KNOTS ( ( 3, 2, 2, 2, 3 ),
 ( 0.6195652173913043237, 0.6231884057971014412, 0.6304347826086956763, 0.6376811594202898004, 0.6413043478260869179 ),
 .UNSPECIFIED. ) 
 CURVE ( )  GEOMETRIC_REPRESENTATION_ITEM ( )  RATIONAL_B_SPLINE_CURVE ( ( 0.9330127018922194093, 0.9330127018922194093, 1.000000000000000000, 0.8660254037844387076, 1.000000000000000000, 0.8660254037844387076, 1.000000000000000000, 0.9330127018922194093, 0.9330127018922194093 ) ) 
 REPRESENTATION_ITEM ( '' )  );
#57479 = CARTESIAN_POINT ( 'NONE',  ( 3.084375000614519191, 6.421520780324663323E-16, -5.243569643749999010 ) ) ;
#57480 = CARTESIAN_POINT ( 'NONE',  ( 20.87812500061451715, -4.541064518000419881, 2.621784821874995952 ) ) ;
#57481 = CARTESIAN_POINT ( 'NONE',  ( 27.64687500061452141, -3.027376345333614438, 5.243569643749998122 ) ) ;
#57482 = CARTESIAN_POINT ( 'NONE',  ( 3.756430356249998770, 16.76562499938548356, 32.16877607737301759 ) ) ;
#57483 = CARTESIAN_POINT ( 'NONE',  ( 19.33125000122903359, -4.330127018922194537, 2.499999999999995559 ) ) ;
#57484 = CARTESIAN_POINT ( 'NONE',  ( 6.946875000614517681, -3.027376345333614438, 5.243569643749998122 ) ) ;
#57485 = CARTESIAN_POINT ( 'NONE',  ( 20.80312500061451431, 0.000000000000000000, 5.243569643749999010 ) ) ;
#57486 = ORIENTED_EDGE ( 'NONE', *, *, #31877, .T. ) ;
#57487 = CARTESIAN_POINT ( 'NONE',  ( 2.000000000000001332, 12.50000000000000000, 33.46410161513774995 ) ) ;
#57488 = CARTESIAN_POINT ( 'NONE',  ( 27.85312500061451502, 4.541064518000418104, -2.621784821874998173 ) ) ;
#57489 = CARTESIAN_POINT ( 'NONE',  ( 4.134375000614517681, 4.541064518000418104, 2.621784821874999949 ) ) ;
#57490 = CARTESIAN_POINT ( 'NONE',  ( 6.712500000000000355, -5.773502691896255534, -1.060575238724906372E-15 ) ) ;
#57491 = CARTESIAN_POINT ( 'NONE',  ( 11.32500000000000107, 6.123233995736764310E-16, -4.999999999999998224 ) ) ;
#57492 = CARTESIAN_POINT ( 'NONE',  ( 16.87500000000000000, 4.330127018922191873, 2.499999999999999556 ) ) ;
#57493 = ORIENTED_EDGE ( 'NONE', *, *, #60829, .T. ) ;
#57494 = CARTESIAN_POINT ( 'NONE',  ( 25.53750000000000142, -2.886751345948129988, 4.999999999999997335 ) ) ;
#57495 = CARTESIAN_POINT ( 'NONE',  ( 26.52187500061451431, 3.027376345333613106, -5.243569643749998122 ) ) ;
#57496 = ADVANCED_FACE ( 'NONE', ( #3404 ), #40403, .T. ) ;
#57497 = VERTEX_POINT ( 'NONE', #22465 ) ;
#57498 = B_SPLINE_CURVE_WITH_KNOTS ( 'NONE', 3,
 ( #44561, #38262, #39372, #44190, #72621, #10561, #50090, #49364, #22365, #21632 ),
 .UNSPECIFIED., .F., .F.,
 ( 4, 3, 3, 4 ),
 ( 3.004629197474318463E-18, 7.861478909946387531E-05, 0.0001572300094823956738, 0.0002815188877693150082 ),
 .UNSPECIFIED. ) ;
#57499 = CARTESIAN_POINT ( 'NONE',  ( 14.61562500061451608, -6.054752690667223547, -1.112240025338166033E-15 ) ) ;
#57500 = CARTESIAN_POINT ( 'NONE',  ( 6.028125000614517504, -4.541064518000419881, 2.621784821874995952 ) ) ;
#57501 = CARTESIAN_POINT ( 'NONE',  ( 18.64687500061451431, -4.119189519843965641, -2.378215178125001383 ) ) ;
#57502 = CARTESIAN_POINT ( 'NONE',  ( 28.15312500061451573, -4.541064518000417216, -2.621784821875001281 ) ) ;
#57503 = CARTESIAN_POINT ( 'NONE',  ( 15.41250000122903252, -4.330127018922190985, -2.500000000000001332 ) ) ;
#57504 = CARTESIAN_POINT ( 'NONE',  ( 20.88749999999999929, 5.773502691896255534, 3.535250795749688894E-16 ) ) ;
#57505 = CARTESIAN_POINT ( 'NONE',  ( 29.66249999999999432, -5.773502691896255534, -1.060575238724906372E-15 ) ) ;
#57506 = CARTESIAN_POINT ( 'NONE',  ( 5.596875000614516260, -3.027376345333614438, 5.243569643749998122 ) ) ;
#57507 = CARTESIAN_POINT ( 'NONE',  ( 10.17187500061451999, -6.054752690667223547, -1.112240025338166033E-15 ) ) ;
#57508 = CARTESIAN_POINT ( 'NONE',  ( 19.77187500061451786, 3.027376345333613106, -5.243569643749998122 ) ) ;
#57509 = DIRECTION ( 'NONE',  ( -1.000000000000000000, -0.000000000000000000, -0.000000000000000000 ) ) ;
#57510 = ORIENTED_EDGE ( 'NONE', *, *, #55763, .F. ) ;
#57511 = CARTESIAN_POINT ( 'NONE',  ( 3.834375000614519635, -4.541064518000419881, 2.621784821874995952 ) ) ;
#57512 = CARTESIAN_POINT ( 'NONE',  ( 6.075000000000000178, 4.330127018922191873, 2.499999999999999556 ) ) ;
#57513 = CARTESIAN_POINT ( 'NONE',  ( 7.321875000614516793, 3.027376345333611329, 5.243569643749999010 ) ) ;
#57514 = AXIS2_PLACEMENT_3D ( 'NONE', #18005, #40563, #63082 ) ;
#57515 = CARTESIAN_POINT ( 'NONE',  ( 19.31250000000000000, -5.773502691896255534, -1.060575238724906372E-15 ) ) ;
#57516 = CARTESIAN_POINT ( 'NONE',  ( 15.10312500061451502, -4.541064518000417216, -2.621784821875001281 ) ) ;
#57517 = CARTESIAN_POINT ( 'NONE',  ( -2.000000000000001776, 20.00000000000000000, 33.46410161513775705 ) ) ;
#57518 = CARTESIAN_POINT ( 'NONE',  ( 24.82500000122902861, -5.773502691896255534, -1.060575238724906372E-15 ) ) ;
#57519 = CARTESIAN_POINT ( 'NONE',  ( 19.95937500061451786, 0.000000000000000000, 4.756430356249998326 ) ) ;
#57520 = CARTESIAN_POINT ( 'NONE',  ( 10.56562500061451715, -6.054752690667223547, -1.112240025338166033E-15 ) ) ;
#57521 = CARTESIAN_POINT ( 'NONE',  ( 26.63437500061451857, 4.541064518000418104, 2.621784821874999949 ) ) ;
#57522 = CARTESIAN_POINT ( 'NONE',  ( -2.121784821874999949, 19.78437500061451715, 26.32496088578401938 ) ) ;
#57523 = CARTESIAN_POINT ( 'NONE',  ( 25.73437500061451644, 4.541064518000418104, 2.621784821874999949 ) ) ;
#57524 = CARTESIAN_POINT ( 'NONE',  ( 6.787500000000001421, -2.886751345948125991, -5.000000000000000000 ) ) ;
#57525 = CARTESIAN_POINT ( 'NONE',  ( 3.999999999999998668, 12.27500000122903501, 27.69059892324149175 ) ) ;
#57526 = CARTESIAN_POINT ( 'NONE',  ( 14.80312500061451608, 4.541064518000418104, -2.621784821874998173 ) ) ;
#57527 = CARTESIAN_POINT ( 'NONE',  ( 6.262500001229034829, 0.000000000000000000, 4.999999999999998224 ) ) ;
#57528 = COLOUR_RGB ( '',0.8941176470588234615, 0.8941176470588234615, 0.8941176470588234615 ) ;
#57529 = CARTESIAN_POINT ( 'NONE',  ( 18.19687500061451502, -3.027376345333614438, 5.243569643749998122 ) ) ;
#57530 = CARTESIAN_POINT ( 'NONE',  ( 12.87187500061451750, -6.054752690667223547, -1.112240025338166033E-15 ) ) ;
#57531 = CARTESIAN_POINT ( 'NONE',  ( 1.999999999999997335, 13.71874999877096535, 33.46410161513775705 ) ) ;
#57532 = ORIENTED_EDGE ( 'NONE', *, *, #8491, .F. ) ;
#57533 = CARTESIAN_POINT ( 'NONE',  ( 12.51562500061451821, 3.027376345333613106, -5.243569643749998122 ) ) ;
#57534 = CARTESIAN_POINT ( 'NONE',  ( 27.18750000122903288, 6.123233995736764310E-16, -4.999999999999998224 ) ) ;
#57535 = CARTESIAN_POINT ( 'NONE',  ( 12.12187500061451573, 3.027376345333613106, -5.243569643749998122 ) ) ;
#57536 = CARTESIAN_POINT ( 'NONE',  ( 3.939080010846523372, -3.079553322829319928, -4.243980907203444453 ) ) ;
#57537 = CARTESIAN_POINT ( 'NONE',  ( 15.81562500061451537, 3.027376345333611329, 5.243569643749999010 ) ) ;
#57538 = CARTESIAN_POINT ( 'NONE',  ( 25.05937500061451573, -4.541064518000417216, -2.621784821875001281 ) ) ;
#57539 = CYLINDRICAL_SURFACE ( 'NONE', #47842, 9.000000000000000000 ) ;
#57540 = CARTESIAN_POINT ( 'NONE',  ( 12.56250000122903465, 0.000000000000000000, 4.999999999999998224 ) ) ;
#57541 = CARTESIAN_POINT ( 'NONE',  ( 7.809375000614519280, 0.000000000000000000, 4.756430356249998326 ) ) ;
#57542 = CARTESIAN_POINT ( 'NONE',  ( -4.243569643749998122, 16.74687500061451573, -27.54997392385601174 ) ) ;
#57543 = CARTESIAN_POINT ( 'NONE',  ( 17.67187500061451644, 3.027376345333611329, 5.243569643749999010 ) ) ;
#57544 = CARTESIAN_POINT ( 'NONE',  ( 19.27500000122903145, 2.886751345948126879, 4.999999999999999112 ) ) ;
#57545 = CARTESIAN_POINT ( 'NONE',  ( 13.54687500061451999, 6.054752690667223547, 3.707466751127219781E-16 ) ) ;
#57546 = CARTESIAN_POINT ( 'NONE',  ( -3.000416591977282496E-16, 19.24062500061451431, -34.90005215228797653 ) ) ;
#57547 = CARTESIAN_POINT ( 'NONE',  ( 20.62500000122903288, 2.886751345948126879, 4.999999999999999112 ) ) ;
#57548 = CARTESIAN_POINT ( 'NONE',  ( 14.42812500061451786, 4.541064518000418104, 2.621784821874999949 ) ) ;
#57549 = ORIENTED_EDGE ( 'NONE', *, *, #71167, .T. ) ;
#57550 = VERTEX_POINT ( 'NONE', #67194 ) ;
#57551 = CARTESIAN_POINT ( 'NONE',  ( 17.36249999999999716, 2.886751345948126879, 4.999999999999999112 ) ) ;
#57552 = DIRECTION ( 'NONE',  ( 0.000000000000000000, 0.000000000000000000, 1.000000000000000000 ) ) ;
#57553 = CARTESIAN_POINT ( 'NONE',  ( 3.740625000614516527, -3.027376345333614438, 5.243569643749998122 ) ) ;
#57554 = CARTESIAN_POINT ( 'NONE',  ( 14.47500000122903430, -5.773502691896255534, -1.060575238724906372E-15 ) ) ;
#57555 = CARTESIAN_POINT ( 'NONE',  ( 26.74687500061451573, -3.027376345333614438, 5.243569643749998122 ) ) ;
#57556 = CARTESIAN_POINT ( 'NONE',  ( 19.94062500061451715, -3.027376345333614438, 5.243569643749998122 ) ) ;
#57557 = CARTESIAN_POINT ( 'NONE',  ( 22.90312500061451573, 4.541064518000418104, -2.621784821874998173 ) ) ;
#57558 = CARTESIAN_POINT ( 'NONE',  ( 3.253125000614518036, 0.000000000000000000, 5.243569643749999010 ) ) ;
#57559 = CARTESIAN_POINT ( 'NONE',  ( 27.03750000000000142, -2.886751345948125991, -5.000000000000000000 ) ) ;
#57560 = CARTESIAN_POINT ( 'NONE',  ( 17.75625000122903074, 4.330127018922192761, -2.499999999999997780 ) ) ;
#57561 = CARTESIAN_POINT ( 'NONE',  ( 10.24687500061451750, -2.746126346562642428, -4.756430356249999214 ) ) ;
#57562 = CARTESIAN_POINT ( 'NONE',  ( 6.450000001229034829, -2.886751345948126435, -5.000000000000000000 ) ) ;
#57563 = CARTESIAN_POINT ( 'NONE',  ( -2.828200636599751609E-16, 10.10000000122903430, -34.61880215351700230 ) ) ;
#57564 = CARTESIAN_POINT ( 'NONE',  ( 4.243569643749999898, 16.48437500061451644, -30.00000000000000000 ) ) ;
#57565 = CARTESIAN_POINT ( 'NONE',  ( 7.125000001229033764, 2.886751345948126879, 4.999999999999999112 ) ) ;
#57566 = CARTESIAN_POINT ( 'NONE',  ( 5.700000000000000178, 0.000000000000000000, 4.999999999999998224 ) ) ;
#57567 = CARTESIAN_POINT ( 'NONE',  ( 4.912500001229034297, 0.000000000000000000, 4.999999999999998224 ) ) ;
#57568 = CARTESIAN_POINT ( 'NONE',  ( 8.859375000614518214, -4.541064518000417216, -2.621784821875001281 ) ) ;
#57569 = DIRECTION ( 'NONE',  ( 0.000000000000000000, 0.000000000000000000, -1.000000000000000000 ) ) ;
#57570 = CARTESIAN_POINT ( 'NONE',  ( 27.60000000122903430, -2.886751345948109559, -5.000000000000028422 ) ) ;
#57571 = CARTESIAN_POINT ( 'NONE',  ( 3.734827092922140768, -3.324314453528163682, -3.734827092927292203 ) ) ;
#57572 = CARTESIAN_POINT ( 'NONE',  ( 24.35625000122903216, -4.330127018922190985, -2.500000000000001332 ) ) ;
#57573 = EDGE_CURVE ( 'NONE', #26559, #8302, #65414, .T. ) ;
#57574 = CARTESIAN_POINT ( 'NONE',  ( 7.771875000614516971, 3.027376345333611329, 5.243569643749999010 ) ) ;
#57575 = CARTESIAN_POINT ( 'NONE',  ( 10.43437500061451750, 4.541064518000418104, 2.621784821874999949 ) ) ;
#57576 = CARTESIAN_POINT ( 'NONE',  ( 7.462500000000001243, 2.886751345948126879, 4.999999999999999112 ) ) ;
#57577 = CARTESIAN_POINT ( 'NONE',  ( 4.243569643749999010, 16.01562500061459460, 27.54997392385601174 ) ) ;
#57578 = CARTESIAN_POINT ( 'NONE',  ( 21.64687500061451786, 6.054752690667223547, 3.707466751127219781E-16 ) ) ;
#57579 = LINE ( 'NONE', #30237, #16283 ) ;
#57580 = CARTESIAN_POINT ( 'NONE',  ( 5.775000000000002132, -4.330127018922194537, 2.499999999999995559 ) ) ;
#57581 = CARTESIAN_POINT ( 'NONE',  ( 25.68750000122903288, -4.330127018922194537, 2.499999999999995559 ) ) ;
#57582 = CARTESIAN_POINT ( 'NONE',  ( 16.58437500061451431, 5.492252693125287522, 3.363034840372157021E-16 ) ) ;
#57583 = CARTESIAN_POINT ( 'NONE',  ( 23.57812500061451289, -4.541064518000419881, 2.621784821874995952 ) ) ;
#57584 = CARTESIAN_POINT ( 'NONE',  ( 12.77812500061451750, -4.541064518000419881, 2.621784821874995952 ) ) ;
#57585 = CARTESIAN_POINT ( 'NONE',  ( 26.85937500061451644, 2.746126346562645981, -4.756430356249997438 ) ) ;
#57586 = CARTESIAN_POINT ( 'NONE',  ( 12.79687500061451821, -3.027376345333614438, 5.243569643749998122 ) ) ;
#57587 = CARTESIAN_POINT ( 'NONE',  ( 28.35000000000000142, -4.330127018922190985, -2.500000000000001332 ) ) ;
#57588 = CARTESIAN_POINT ( 'NONE',  ( 23.66250000122903430, 4.330127018922192761, -2.499999999999997780 ) ) ;
#57589 = LINE ( 'NONE', #51697, #72105 ) ;
#57590 = CARTESIAN_POINT ( 'NONE',  ( 12.98437500061451821, 6.421520780324663323E-16, -5.243569643749999010 ) ) ;
#57591 = CARTESIAN_POINT ( 'NONE',  ( 27.83437500061451786, 6.421520780324663323E-16, -5.243569643749999010 ) ) ;
#57592 = CARTESIAN_POINT ( 'NONE',  ( 4.246875000614519280, -3.027376345333614438, 5.243569643749998122 ) ) ;
#57593 = CARTESIAN_POINT ( 'NONE',  ( -2.000000000000000000, 12.83750000122903501, -33.46410161513775705 ) ) ;
#57594 = CARTESIAN_POINT ( 'NONE',  ( 21.30937500061451573, 0.000000000000000000, 5.243569643749999010 ) ) ;
#57595 = CARTESIAN_POINT ( 'NONE',  ( 13.54687500061451999, 6.054752690667223547, 3.707466751127219781E-16 ) ) ;
#57596 = CARTESIAN_POINT ( 'NONE',  ( 3.756430356250000546, 17.74062499938548143, 27.83122392262697886 ) ) ;
#57597 = CARTESIAN_POINT ( 'NONE',  ( 25.34999999999999787, 4.330127018922192761, -2.499999999999997780 ) ) ;
#57598 = CARTESIAN_POINT ( 'NONE',  ( -4.000000000000000888, 13.66250000000000142, 32.30940107675850470 ) ) ;
#57599 = CARTESIAN_POINT ( 'NONE',  ( 27.53437500061451360, 4.119189519843966529, 2.378215178124999607 ) ) ;
#57600 = CARTESIAN_POINT ( 'NONE',  ( 16.34062500061451573, -3.027376345333614438, 5.243569643749998122 ) ) ;
#57601 = CARTESIAN_POINT ( 'NONE',  ( 7.312500000000000000, 2.886751345948129099, -4.999999999999998224 ) ) ;
#57602 = FACE_OUTER_BOUND ( 'NONE', #34053, .T. ) ;
#57603 = CARTESIAN_POINT ( 'NONE',  ( 15.71250000000000213, -5.773502691896255534, -1.060575238724906372E-15 ) ) ;
#57604 = CARTESIAN_POINT ( 'NONE',  ( -2.121784821874999949, 10.27812500061451750, 26.32496088578401938 ) ) ;
#57605 = DIRECTION ( 'NONE',  ( -0.000000000000000000, -1.000000000000000000, -0.000000000000000000 ) ) ;
#57606 = CARTESIAN_POINT ( 'NONE',  ( 24.08437500061451786, -4.541064518000419881, 2.621784821874995952 ) ) ;
#57607 = ORIENTED_EDGE ( 'NONE', *, *, #52924, .F. ) ;
#57608 = CARTESIAN_POINT ( 'NONE',  ( 18.44062500061451715, 6.054752690667223547, 3.707466751127219781E-16 ) ) ;
#57609 = CARTESIAN_POINT ( 'NONE',  ( 20.22187500061451715, 3.027376345333613106, -5.243569643749998122 ) ) ;
#57610 = CARTESIAN_POINT ( 'NONE',  ( 3.149999999999999911, -4.330127018922190985, -2.500000000000001332 ) ) ;
#57611 = CARTESIAN_POINT ( 'NONE',  ( 7.415625000614516793, -6.054752690667223547, -1.112240025338166033E-15 ) ) ;
#57612 = CARTESIAN_POINT ( 'NONE',  ( 20.87812500061451715, -4.541064518000419881, 2.621784821874995952 ) ) ;
#57613 = CARTESIAN_POINT ( 'NONE',  ( 13.09687500061451892, 6.054752690667223547, 3.707466751127219781E-16 ) ) ;
#57614 = CARTESIAN_POINT ( 'NONE',  ( 16.77187500061451786, 3.027376345333611329, 5.243569643749999010 ) ) ;
#57615 = CARTESIAN_POINT ( 'NONE',  ( -4.243569643749997233, 18.04062500061451857, 32.45002607614398471 ) ) ;
#57616 = CARTESIAN_POINT ( 'NONE',  ( 19.01250000122903216, -4.330127018922190985, -2.500000000000001332 ) ) ;
#57617 = CARTESIAN_POINT ( 'NONE',  ( 14.22187500061451892, -5.492252693125287522, -1.008910452111647106E-15 ) ) ;
#57618 = CARTESIAN_POINT ( 'NONE',  ( 9.065625000614515372, 3.027376345333611329, 5.243569643749999010 ) ) ;
#57619 = CARTESIAN_POINT ( 'NONE',  ( 3.046875000614519990, -3.027376345333610441, -5.243569643749999898 ) ) ;
#57620 = CARTESIAN_POINT ( 'NONE',  ( 5.146875000614517859, -3.027376345333614438, 5.243569643749998122 ) ) ;
#57621 = CARTESIAN_POINT ( 'NONE',  ( 24.98437500061451644, -4.541064518000419881, 2.621784821874995952 ) ) ;
#57622 = CARTESIAN_POINT ( 'NONE',  ( 17.46562500061451217, 3.027376345333613106, -5.243569643749998122 ) ) ;
#57623 = CARTESIAN_POINT ( 'NONE',  ( 27.41250000122903430, 0.000000000000000000, 4.999999999999998224 ) ) ;
#57624 = CARTESIAN_POINT ( 'NONE',  ( 25.82812500061451644, -4.541064518000419881, 2.621784821874995952 ) ) ;
#57625 = CARTESIAN_POINT ( 'NONE',  ( 21.60937500061451644, 4.541064518000418104, -2.621784821874998173 ) ) ;
#57626 = CARTESIAN_POINT ( 'NONE',  ( 17.31562500061451715, -6.054752690667223547, -1.112240025338166033E-15 ) ) ;
#57627 = CARTESIAN_POINT ( 'NONE',  ( -2.121784821874996840, 17.23437500061451999, 33.67503911421598417 ) ) ;
#57628 = CARTESIAN_POINT ( 'NONE',  ( 22.15312500061451573, 0.000000000000000000, 5.243569643749999010 ) ) ;
#57629 = ORIENTED_EDGE ( 'NONE', *, *, #32239, .F. ) ;
#57630 = CARTESIAN_POINT ( 'NONE',  ( 26.25000000000000000, 4.330127018922192761, -2.499999999999997780 ) ) ;
#57631 = CARTESIAN_POINT ( 'NONE',  ( -1.999999999999997113, 13.77500000000000036, -26.53589838486224295 ) ) ;
#57632 = CARTESIAN_POINT ( 'NONE',  ( 2.655984681222220721E-16, 18.71562499938548285, 25.66244784525396483 ) ) ;
#57633 = CARTESIAN_POINT ( 'NONE',  ( 3.346875000614518036, -3.027376345333614438, 5.243569643749998122 ) ) ;
#57634 = CARTESIAN_POINT ( 'NONE',  ( 10.67812500061451608, 6.421520780324663323E-16, -5.243569643749999010 ) ) ;
#57635 = CARTESIAN_POINT ( 'NONE',  ( 22.68750000122903288, 6.123233995736764310E-16, -4.999999999999998224 ) ) ;
#57636 = CARTESIAN_POINT ( 'NONE',  ( 26.69062500061451715, -3.027376345333614438, 5.243569643749998122 ) ) ;
#57637 = CARTESIAN_POINT ( 'NONE',  ( 25.50000000000000000, 0.000000000000000000, 4.999999999999998224 ) ) ;
#57638 = CARTESIAN_POINT ( 'NONE',  ( 8.484601909799253346E-16, 16.62500000122903288, -25.38119784648299770 ) ) ;
#57639 = CARTESIAN_POINT ( 'NONE',  ( -1.071796769724504328, 12.55490381179670045, 33.99999999999999289 ) ) ;
#57640 = CARTESIAN_POINT ( 'NONE',  ( 10.00312500061451715, 0.000000000000000000, 5.243569643749999010 ) ) ;
#57641 = ORIENTED_EDGE ( 'NONE', *, *, #70842, .T. ) ;
#57642 = EDGE_CURVE ( 'NONE', #44184, #65074, #16870, .T. ) ;
#57643 = CARTESIAN_POINT ( 'NONE',  ( 25.75312500061451715, 0.000000000000000000, 5.243569643749999010 ) ) ;
#57644 = CARTESIAN_POINT ( 'NONE',  ( 8.015625000614518214, 3.027376345333613106, -5.243569643749998122 ) ) ;
#57645 = CARTESIAN_POINT ( 'NONE',  ( 6.778125000614518392, 4.541064518000418104, 2.621784821874999949 ) ) ;
#57646 = CARTESIAN_POINT ( 'NONE',  ( 16.24687500061451573, 5.492252693125287522, 3.363034840372157021E-16 ) ) ;
#57647 = EDGE_CURVE ( 'NONE', #68293, #8342, #42771, .T. ) ;
#57648 = CARTESIAN_POINT ( 'NONE',  ( 0.000000000000000000, 0.000000000000000000, 50.00000000000000000 ) ) ;
#57649 = CARTESIAN_POINT ( 'NONE',  ( 13.16249999999999964, 2.886751345948129099, -4.999999999999998224 ) ) ;
#57650 = EDGE_CURVE ( 'NONE', #33928, #4907, #7383, .T. ) ;
#57651 = CARTESIAN_POINT ( 'NONE',  ( 13.54687500061451999, 6.054752690667223547, 3.707466751127219781E-16 ) ) ;
#57652 = CARTESIAN_POINT ( 'NONE',  ( 10.53750000122903252, 6.123233995736764310E-16, -4.999999999999998224 ) ) ;
#57653 = CARTESIAN_POINT ( 'NONE',  ( 17.85937500061451999, -4.541064518000417216, -2.621784821875001281 ) ) ;
#57654 = CARTESIAN_POINT ( 'NONE',  ( 17.66249999999999787, 2.886751345948129099, -4.999999999999998224 ) ) ;
#57655 = CARTESIAN_POINT ( 'NONE',  ( 8.971875000614515372, 3.027376345333613106, -5.243569643749998122 ) ) ;
#57656 = CARTESIAN_POINT ( 'NONE',  ( 4.243569643749999010, 11.06562500061451715, -32.45002607614398471 ) ) ;
#57657 = CYLINDRICAL_SURFACE ( 'NONE', #65466, 4.000000000000000000 ) ;
#57658 = CARTESIAN_POINT ( 'NONE',  ( 23.97187500061451715, -4.119189519843968306, 2.378215178124996054 ) ) ;
#57659 = CARTESIAN_POINT ( 'NONE',  ( 2.000000000000000444, 13.41874999877096641, 26.53589838486224650 ) ) ;
#57660 = CARTESIAN_POINT ( 'NONE',  ( 24.21562500061451573, 3.027376345333613106, -5.243569643749998122 ) ) ;
#57661 = SURFACE_STYLE_USAGE ( .BOTH. , #29595 ) ;
#57662 = CARTESIAN_POINT ( 'NONE',  ( 29.40937500061451715, 0.000000000000000000, 5.243569643749999010 ) ) ;
#57663 = CARTESIAN_POINT ( 'NONE',  ( 25.42500000000000071, 4.330127018922191873, 2.499999999999999556 ) ) ;
#57664 = CARTESIAN_POINT ( 'NONE',  ( 8.053125000614516082, 4.541064518000418104, -2.621784821874998173 ) ) ;
#57665 = CARTESIAN_POINT ( 'NONE',  ( 24.68437500061451573, 5.492252693125287522, 3.363034840372157021E-16 ) ) ;
#57666 = CARTESIAN_POINT ( 'NONE',  ( 18.38437500061451857, 6.421520780324663323E-16, -5.243569643749999010 ) ) ;
#57667 = CARTESIAN_POINT ( 'NONE',  ( 11.67187500061451644, 4.119189519843966529, 2.378215178124999607 ) ) ;
#57668 = CARTESIAN_POINT ( 'NONE',  ( 2.915625000614516793, -6.054752690667223547, -1.112240025338166033E-15 ) ) ;
#57669 = CARTESIAN_POINT ( 'NONE',  ( 8.934375000614517504, 6.421520780324663323E-16, -5.243569643749999010 ) ) ;
#57670 = ORIENTED_EDGE ( 'NONE', *, *, #69599, .T. ) ;
#57671 = CARTESIAN_POINT ( 'NONE',  ( 18.60937500061451644, 0.000000000000000000, 5.243569643749999010 ) ) ;
#57672 = DIRECTION ( 'NONE',  ( 0.000000000000000000, 0.000000000000000000, -1.000000000000000000 ) ) ;
#57673 = CARTESIAN_POINT ( 'NONE',  ( 27.15000000000000213, 4.330127018922192761, -2.499999999999997780 ) ) ;
#57675 = EDGE_CURVE ( 'NONE', #64110, #19257, #48186, .T. ) ;
#57674 = CARTESIAN_POINT ( 'NONE',  ( 28.95937500061451431, 0.000000000000000000, 5.243569643749999010 ) ) ;
#57676 = CARTESIAN_POINT ( 'NONE',  ( 29.62500000000000000, -4.330127018922194537, 2.499999999999995559 ) ) ;
#57677 = CARTESIAN_POINT ( 'NONE',  ( 10.83750000000000036, -2.886751345948193048, -4.999999999999883649 ) ) ;
#57678 = ORIENTED_EDGE ( 'NONE', *, *, #22404, .F. ) ;
#57679 = CARTESIAN_POINT ( 'NONE',  ( 10.31250000000000355, -5.773502691896255534, -1.060575238724906372E-15 ) ) ;
#57680 = CARTESIAN_POINT ( 'NONE',  ( 11.22187500061451537, 4.119189519843966529, 2.378215178124999607 ) ) ;
#57681 = CARTESIAN_POINT ( 'NONE',  ( 25.49062500061451786, -3.027376345333610441, -5.243569643749999898 ) ) ;
#57682 = CARTESIAN_POINT ( 'NONE',  ( 15.07499999999999929, 4.330127018922191873, 2.499999999999999556 ) ) ;
#57683 = CARTESIAN_POINT ( 'NONE',  ( 11.21250000122903501, 0.000000000000000000, 4.999999999999998224 ) ) ;
#57684 = CARTESIAN_POINT ( 'NONE',  ( 8.165625000614516793, 3.027376345333611329, 5.243569643749999010 ) ) ;
#57685 = CARTESIAN_POINT ( 'NONE',  ( 22.12500000000000000, 6.123233995736764310E-16, -4.999999999999998224 ) ) ;
#57686 = CARTESIAN_POINT ( 'NONE',  ( 20.01562500061451644, -6.054752690667223547, -1.112240025338166033E-15 ) ) ;
#57687 = CARTESIAN_POINT ( 'NONE',  ( 16.08750000122903501, 4.330127018922191873, 2.499999999999999556 ) ) ;
#57688 = CARTESIAN_POINT ( 'NONE',  ( 26.17500000122903359, -5.773502691896255534, -1.060575238724906372E-15 ) ) ;
#57689 = CARTESIAN_POINT ( 'NONE',  ( 3.756430356250000102, 17.59062499938548285, 30.00000000000000000 ) ) ;
#57690 = CARTESIAN_POINT ( 'NONE',  ( 5.025000000000002132, 6.123233995736764310E-16, -4.999999999999998224 ) ) ;
#57691 = ORIENTED_EDGE ( 'NONE', *, *, #5473, .F. ) ;
#57692 = CARTESIAN_POINT ( 'NONE',  ( 21.77812500061451928, -4.541064518000419881, 2.621784821874995952 ) ) ;
#57693 = CARTESIAN_POINT ( 'NONE',  ( 3.317784727594947913, -3.740628891154329061, -3.422312309320198143 ) ) ;
#57694 = CARTESIAN_POINT ( 'NONE',  ( 27.04687500061451644, 6.054752690667223547, 3.707466751127219781E-16 ) ) ;
#57695 = CARTESIAN_POINT ( 'NONE',  ( 18.42187500061451644, 3.027376345333613106, -5.243569643749998122 ) ) ;
#57696 = CARTESIAN_POINT ( 'NONE',  ( 15.40312500061451573, 0.000000000000000000, 5.243569643749999010 ) ) ;
#57697 = CARTESIAN_POINT ( 'NONE',  ( 30.00000000000000000, 0.000000000000000000, 0.000000000000000000 ) ) ;
#57698 = CARTESIAN_POINT ( 'NONE',  ( 25.08750000122903145, 4.330127018922191873, 2.499999999999999556 ) ) ;
#57699 = CARTESIAN_POINT ( 'NONE',  ( 22.24687500061451573, -2.746126346562646425, 4.756430356249996549 ) ) ;
#57700 = CARTESIAN_POINT ( 'NONE',  ( 16.52812500061451573, 6.421520780324663323E-16, -5.243569643749999010 ) ) ;
#57701 = CARTESIAN_POINT ( 'NONE',  ( 4.000000000000000000, 13.88750000000000107, 32.30940107675849760 ) ) ;
#57702 = CARTESIAN_POINT ( 'NONE',  ( 4.425000001229032698, 2.886751345948126879, 4.999999999999999112 ) ) ;
#57703 = CARTESIAN_POINT ( 'NONE',  ( 12.04687500061451821, -3.027376345333610441, -5.243569643749999898 ) ) ;
#57704 = CARTESIAN_POINT ( 'NONE',  ( 11.37187500061451750, 3.027376345333611329, 5.243569643749999010 ) ) ;
#57705 = CARTESIAN_POINT ( 'NONE',  ( 20.40937500061451715, 0.000000000000000000, 5.243569643749999010 ) ) ;
#57706 = VERTEX_POINT ( 'NONE', #29108 ) ;
#57707 = CARTESIAN_POINT ( 'NONE',  ( 9.937500000000001776, -2.886751345948126435, -5.000000000000000000 ) ) ;
#57708 = CARTESIAN_POINT ( 'NONE',  ( 23.27812500061451573, 6.421520780324663323E-16, -5.243569643749999010 ) ) ;
#57709 =( BOUNDED_CURVE ( )  B_SPLINE_CURVE ( 2, ( #40872, #63389, #12774, #57832, #47129, #19025, #41584 ),
 .UNSPECIFIED., .F., .F. ) 
 B_SPLINE_CURVE_WITH_KNOTS ( ( 3, 2, 2, 3 ),
 ( 0.5250000000000000222, 0.5277777777777777901, 0.5305555555555556690, 0.5333333333333334370 ),
 .UNSPECIFIED. ) 
 CURVE ( )  GEOMETRIC_REPRESENTATION_ITEM ( )  RATIONAL_B_SPLINE_CURVE ( ( 1.000000000000000000, 0.8660254037844387076, 1.000000000000000000, 0.8660254037844387076, 1.000000000000000000, 0.8660254037844333785, 1.000000000000005329 ) ) 
 REPRESENTATION_ITEM ( '' )  );
#57710 = CARTESIAN_POINT ( 'NONE',  ( 18.98437500061451644, 4.541064518000418104, 2.621784821874999949 ) ) ;
#57711 = CARTESIAN_POINT ( 'NONE',  ( 24.10312500061451502, -4.541064518000417216, -2.621784821875001281 ) ) ;
#57712 = CARTESIAN_POINT ( 'NONE',  ( 8.484601909799253346E-16, 14.71250000000000036, 34.61880215351700230 ) ) ;
#57713 = CARTESIAN_POINT ( 'NONE',  ( 2.896875000614518747, -3.027376345333614438, 5.243569643749998122 ) ) ;
#57714 = CARTESIAN_POINT ( 'NONE',  ( 9.675000001229035362, 2.886751345948129099, -4.999999999999998224 ) ) ;
#57715 = CARTESIAN_POINT ( 'NONE',  ( 3.600000001229033408, -2.886751345948129988, 4.999999999999997335 ) ) ;
#57716 = CARTESIAN_POINT ( 'NONE',  ( 45.00000000000000000, 0.000000000000000000, 0.000000000000000000 ) ) ;
#57717 = CARTESIAN_POINT ( 'NONE',  ( 28.01250000122903216, -4.330127018922190985, -2.500000000000001332 ) ) ;
#57718 = CARTESIAN_POINT ( 'NONE',  ( 1.878215178125000495, 13.72812499938548392, 26.74683588394047007 ) ) ;
#57719 = CARTESIAN_POINT ( 'NONE',  ( 9.571875000614518569, 3.027376345333611329, 5.243569643749999010 ) ) ;
#57720 = CARTESIAN_POINT ( 'NONE',  ( 45.00000000000000000, 0.000000000000000000, 4.999999999999998224 ) ) ;
#57721 = CARTESIAN_POINT ( 'NONE',  ( 17.31562500061451715, -6.054752690667223547, -1.112240025338166033E-15 ) ) ;
#57722 = CARTESIAN_POINT ( 'NONE',  ( 11.25937500061451679, 4.541064518000418104, -2.621784821874998173 ) ) ;
#57723 = CARTESIAN_POINT ( 'NONE',  ( 3.628125000614518036, 4.541064518000418104, 2.621784821874999949 ) ) ;
#57724 = CARTESIAN_POINT ( 'NONE',  ( 20.74687500061452283, 6.054752690667223547, 3.707466751127219781E-16 ) ) ;
#57725 = CARTESIAN_POINT ( 'NONE',  ( 7.734375000614517326, 4.541064518000418104, 2.621784821874999949 ) ) ;
#57726 = CARTESIAN_POINT ( 'NONE',  ( 3.178125000614515638, 4.541064518000418104, 2.621784821874999949 ) ) ;
#57727 = CARTESIAN_POINT ( 'NONE',  ( 1.510657702057710734E-15, 19.10000000122903430, 26.00000000000000000 ) ) ;
#57728 = CARTESIAN_POINT ( 'NONE',  ( 6.928125000614516082, -4.541064518000419881, 2.621784821874995952 ) ) ;
#57729 = CARTESIAN_POINT ( 'NONE',  ( 18.89062500061451644, 6.054752690667223547, 3.707466751127219781E-16 ) ) ;
#57730 = ORIENTED_EDGE ( 'NONE', *, *, #8440, .F. ) ;
#57731 = CARTESIAN_POINT ( 'NONE',  ( 6.000000001229033764, -2.886751345948125991, -5.000000000000000000 ) ) ;
#57732 = CARTESIAN_POINT ( 'NONE',  ( 13.94062500061451892, 6.054752690667223547, 3.707466751127219781E-16 ) ) ;
#57733 = CARTESIAN_POINT ( 'NONE',  ( 13.15312500061451750, 0.000000000000000000, 5.243569643749999010 ) ) ;
#57734 = CARTESIAN_POINT ( 'NONE',  ( 22.58437500061451431, 4.119189519843966529, 2.378215178124999607 ) ) ;
#57735 = CARTESIAN_POINT ( 'NONE',  ( 13.16249999999999964, 2.886751345948129099, -4.999999999999998224 ) ) ;
#57736 = CARTESIAN_POINT ( 'NONE',  ( 5.925000001229033586, -5.773502691896255534, -1.060575238724906372E-15 ) ) ;
#57737 = EDGE_CURVE ( 'NONE', #3869, #4423, #51642, .T. ) ;
#57738 = CARTESIAN_POINT ( 'NONE',  ( 18.45000000122903216, -2.886751345948129988, 4.999999999999997335 ) ) ;
#57739 = CARTESIAN_POINT ( 'NONE',  ( 24.56250000000000000, 2.886751345948126879, 4.999999999999999112 ) ) ;
#57740 = CARTESIAN_POINT ( 'NONE',  ( 2.121784821875001281, 11.90937500061451892, -26.32496088578401938 ) ) ;
#57741 = DIRECTION ( 'NONE',  ( -0.000000000000000000, -1.000000000000000000, -0.000000000000000000 ) ) ;
#57742 = CARTESIAN_POINT ( 'NONE',  ( 12.80625000122903323, 4.330127018922192761, -2.499999999999997780 ) ) ;
#57743 = CARTESIAN_POINT ( 'NONE',  ( 6.450000000000001066, 4.330127018922192761, -2.499999999999997780 ) ) ;
#57744 = CARTESIAN_POINT ( 'NONE',  ( 24.44999999999999929, 4.330127018922192761, -2.499999999999997780 ) ) ;
#57745 = CARTESIAN_POINT ( 'NONE',  ( 19.13437500061451857, -4.541064518000419881, 2.621784821874995952 ) ) ;
#57746 = CARTESIAN_POINT ( 'NONE',  ( 4.898587196589411843E-16, 20.00000000000000000, -26.00000000000000000 ) ) ;
#57747 = CARTESIAN_POINT ( 'NONE',  ( 13.75312500061451715, -4.541064518000417216, -2.621784821875001281 ) ) ;
#57748 = CARTESIAN_POINT ( 'NONE',  ( 10.48125000122903216, 6.123233995736764310E-16, -4.999999999999998224 ) ) ;
#57749 = DIRECTION ( 'NONE',  ( 0.000000000000000000, 0.000000000000000000, -1.000000000000000000 ) ) ;
#57750 = CARTESIAN_POINT ( 'NONE',  ( 25.54687500061451644, -3.027376345333610441, -5.243569643749999898 ) ) ;
#57751 = CARTESIAN_POINT ( 'NONE',  ( 17.44687500061451502, 4.119189519843966529, -2.378215178124998275 ) ) ;
#57752 = CARTESIAN_POINT ( 'NONE',  ( 9.778125000614517504, 6.421520780324663323E-16, -5.243569643749999010 ) ) ;
#57753 = CARTESIAN_POINT ( 'NONE',  ( 14.97187500061451892, 3.027376345333611329, 5.243569643749999010 ) ) ;
#57754 = EDGE_LOOP ( 'NONE', ( #46380, #29612, #22461, #15717 ) ) ;
#57755 = CARTESIAN_POINT ( 'NONE',  ( 26.39062500061451644, -3.027376345333610441, -5.243569643749999898 ) ) ;
#57756 = CARTESIAN_POINT ( 'NONE',  ( 19.71562500061451928, 3.027376345333613106, -5.243569643749998122 ) ) ;
#57757 = CARTESIAN_POINT ( 'NONE',  ( 18.93750000000000000, -2.886751345948159742, -4.999999999999942268 ) ) ;
#57758 = CARTESIAN_POINT ( 'NONE',  ( -1.071796769724504328, 14.35490381179669939, -26.00000000000001066 ) ) ;
#57759 = CARTESIAN_POINT ( 'NONE',  ( 8.925000000000002487, -4.330127018922194537, 2.499999999999995559 ) ) ;
#57760 = CARTESIAN_POINT ( 'NONE',  ( 18.71250000122903145, 4.330127018922192761, -2.499999999999997780 ) ) ;
#57761 = CARTESIAN_POINT ( 'NONE',  ( 1.071796769724491893, 10.23259618943233384, 33.99999999999999289 ) ) ;
#57762 = CARTESIAN_POINT ( 'NONE',  ( 10.05937500061451750, -5.492252693125287522, -1.008910452111647106E-15 ) ) ;
#57763 = ORIENTED_EDGE ( 'NONE', *, *, #70520, .T. ) ;
#57764 = CARTESIAN_POINT ( 'NONE',  ( 18.11250000000000071, 2.886751345948129099, -4.999999999999998224 ) ) ;
#57765 = CARTESIAN_POINT ( 'NONE',  ( 21.26249999999999574, 2.886751345948129099, -4.999999999999998224 ) ) ;
#57766 = CARTESIAN_POINT ( 'NONE',  ( 20.14687500061451786, -3.027376345333610441, -5.243569643749999898 ) ) ;
#57767 = CARTESIAN_POINT ( 'NONE',  ( 24.06562500061451715, -6.054752690667223547, -1.112240025338166033E-15 ) ) ;
#57768 = VERTEX_POINT ( 'NONE', #1043 ) ;
#57769 = CARTESIAN_POINT ( 'NONE',  ( 5.165625000614518569, -6.054752690667223547, -1.112240025338166033E-15 ) ) ;
#57770 = DIRECTION ( 'NONE',  ( -0.000000000000000000, -1.000000000000000000, -0.000000000000000000 ) ) ;
#57771 = CARTESIAN_POINT ( 'NONE',  ( 13.87500000000000178, -4.330127018922194537, 2.499999999999995559 ) ) ;
#57772 = CARTESIAN_POINT ( 'NONE',  ( 4.243569643749999898, 18.19062500061451360, 32.45002607614398471 ) ) ;
#57773 = CARTESIAN_POINT ( 'NONE',  ( 29.01562500061451644, -6.054752690667223547, -1.112240025338166033E-15 ) ) ;
#57774 = CARTESIAN_POINT ( 'NONE',  ( 11.21250000000000036, -5.773502691896255534, -1.060575238724906372E-15 ) ) ;
#57775 = CARTESIAN_POINT ( 'NONE',  ( -1.878215178124999163, 16.84062499938548285, 26.74683588394047007 ) ) ;
#57776 = CARTESIAN_POINT ( 'NONE',  ( 25.54687500061451644, -3.027376345333610441, -5.243569643749999898 ) ) ;
#57777 = ORIENTED_EDGE ( 'NONE', *, *, #38932, .T. ) ;
#57778 = CARTESIAN_POINT ( 'NONE',  ( 20.39062500061451644, -3.027376345333614438, 5.243569643749998122 ) ) ;
#57779 = CARTESIAN_POINT ( 'NONE',  ( 22.39687500061451075, -3.027376345333610441, -5.243569643749999898 ) ) ;
#57780 = EDGE_CURVE ( 'NONE', #42476, #69693, #39842, .T. ) ;
#57781 = CARTESIAN_POINT ( 'NONE',  ( 2.121784821875001281, 16.80312500061459247, -26.32496088578401938 ) ) ;
#57782 = CARTESIAN_POINT ( 'NONE',  ( 6.703125000614516438, 4.541064518000418104, -2.621784821874998173 ) ) ;
#57783 = CARTESIAN_POINT ( 'NONE',  ( 28.92187500061451644, 2.746126346562643317, 4.756430356249998326 ) ) ;
#57784 = CARTESIAN_POINT ( 'NONE',  ( 22.79062500061451502, -3.027376345333610441, -5.243569643749999898 ) ) ;
#57785 = CARTESIAN_POINT ( 'NONE',  ( 27.27187500061451786, 5.824947211148865298E-16, -4.756430356249998326 ) ) ;
#57786 = CARTESIAN_POINT ( 'NONE',  ( 12.98437500061451821, 5.824947211148865298E-16, -4.756430356249998326 ) ) ;
#57787 = CARTESIAN_POINT ( 'NONE',  ( 17.89687500061451431, -3.027376345333610441, -5.243569643749999898 ) ) ;
#57788 = CARTESIAN_POINT ( 'NONE',  ( 19.32187500061451857, 3.027376345333613106, -5.243569643749998122 ) ) ;
#57789 = CARTESIAN_POINT ( 'NONE',  ( 27.15937500061451360, 0.000000000000000000, 5.243569643749999010 ) ) ;
#57790 = CARTESIAN_POINT ( 'NONE',  ( 9.001249775931846008E-16, 15.47187500061451892, 34.90005215228797653 ) ) ;
#57791 = CARTESIAN_POINT ( 'NONE',  ( 8.540625000614518569, 6.054752690667223547, 3.707466751127219781E-16 ) ) ;
#57792 = CARTESIAN_POINT ( 'NONE',  ( -3.999999999999999112, 18.19999999999999929, -30.00000000000000000 ) ) ;
#57793 = CARTESIAN_POINT ( 'NONE',  ( 5.334375000614517859, 6.421520780324663323E-16, -5.243569643749999010 ) ) ;
#57794 = DIRECTION ( 'NONE',  ( 0.000000000000000000, 0.000000000000000000, 1.000000000000000000 ) ) ;
#57795 = CARTESIAN_POINT ( 'NONE',  ( 4.903125000614516615, 4.541064518000418104, -2.621784821874998173 ) ) ;
#57796 = CARTESIAN_POINT ( 'NONE',  ( 9.646875000614516082, -3.027376345333614438, 5.243569643749998122 ) ) ;
#57797 =( NAMED_UNIT ( * ) PLANE_ANGLE_UNIT ( ) SI_UNIT ( $, .RADIAN. ) );
#57798 = CARTESIAN_POINT ( 'NONE',  ( 17.73750000122903359, 6.123233995736764310E-16, -4.999999999999998224 ) ) ;
#57799 = CARTESIAN_POINT ( 'NONE',  ( 4.846875000614519813, -3.027376345333610441, -5.243569643749999898 ) ) ;
#57800 = CARTESIAN_POINT ( 'NONE',  ( 6.365625000614518747, 3.027376345333611329, 5.243569643749999010 ) ) ;
#57801 = CARTESIAN_POINT ( 'NONE',  ( 4.000000000000000000, 13.79374999877096641, 30.00000000000000000 ) ) ;
#57802 = CARTESIAN_POINT ( 'NONE',  ( 24.01875000122903359, 2.886751345948129099, -4.999999999999998224 ) ) ;
#57803 = CARTESIAN_POINT ( 'NONE',  ( 16.28437500061452070, 4.541064518000418104, 2.621784821874999949 ) ) ;
#57804 = CARTESIAN_POINT ( 'NONE',  ( 22.76249999999999574, 2.886751345948098901, 5.000000000000047073 ) ) ;
#57805 = ORIENTED_EDGE ( 'NONE', *, *, #60483, .F. ) ;
#57806 = CARTESIAN_POINT ( 'NONE',  ( 24.06562500061451715, -6.054752690667223547, -1.112240025338166033E-15 ) ) ;
#57807 = CARTESIAN_POINT ( 'NONE',  ( 8.728125000614518569, -4.541064518000419881, 2.621784821874995952 ) ) ;
#57808 = CARTESIAN_POINT ( 'NONE',  ( 26.67187500061451644, 3.027376345333611329, 5.243569643749999010 ) ) ;
#57809 = CARTESIAN_POINT ( 'NONE',  ( 9.103125000614515017, 0.000000000000000000, 5.243569643749999010 ) ) ;
#57810 = CARTESIAN_POINT ( 'NONE',  ( 4.474433822073803135, -2.231832360841083496, -4.606514653318270369 ) ) ;
#57811 = CARTESIAN_POINT ( 'NONE',  ( 10.83750000122903501, -4.330127018922194537, 2.499999999999995559 ) ) ;
#57812 = CARTESIAN_POINT ( 'NONE',  ( 25.67812500061451431, 4.541064518000418104, 2.621784821874999949 ) ) ;
#57813 = CARTESIAN_POINT ( 'NONE',  ( 4.243569643749999898, 13.27812500061451750, -30.00000000000000000 ) ) ;
#57814 = CARTESIAN_POINT ( 'NONE',  ( 11.81250000122903465, -4.330127018922190985, -2.500000000000001332 ) ) ;
#57815 = CARTESIAN_POINT ( 'NONE',  ( 23.20312500061451644, -4.541064518000417216, -2.621784821875001281 ) ) ;
#57816 = CARTESIAN_POINT ( 'NONE',  ( 10.57500000000000107, 4.330127018922191873, 2.499999999999999556 ) ) ;
#57817 = CARTESIAN_POINT ( 'NONE',  ( 20.54062500061451502, -3.027376345333610441, -5.243569643749999898 ) ) ;
#57818 = CARTESIAN_POINT ( 'NONE',  ( 5.334375000614517859, 6.421520780324663323E-16, -5.243569643749999010 ) ) ;
#57819 = CARTESIAN_POINT ( 'NONE',  ( 20.62499999999999645, -4.330127018922194537, 2.499999999999995559 ) ) ;
#57820 = CARTESIAN_POINT ( 'NONE',  ( 12.60000000122903430, -2.886751345948129988, 4.999999999999997335 ) ) ;
#57821 = CARTESIAN_POINT ( 'NONE',  ( 12.14062500061451821, 6.054752690667223547, 3.707466751127219781E-16 ) ) ;
#57822 = EDGE_CURVE ( 'NONE', #44451, #72067, #62618, .T. ) ;
#57823 = CARTESIAN_POINT ( 'NONE',  ( 14.99062500061451786, -3.027376345333614438, 5.243569643749998122 ) ) ;
#57824 = EDGE_CURVE ( 'NONE', #44223, #44755, #6936, .T. ) ;
#57825 = CARTESIAN_POINT ( 'NONE',  ( 26.25000000122903288, -2.886751345948125991, -5.000000000000000000 ) ) ;
#57826 = CARTESIAN_POINT ( 'NONE',  ( 21.33749999999999858, 5.773502691896255534, 3.535250795749688894E-16 ) ) ;
#57827 = CARTESIAN_POINT ( 'NONE',  ( 23.03437500061451715, 4.541064518000418104, 2.621784821874999949 ) ) ;
#57828 = DIRECTION ( 'NONE',  ( -0.000000000000000000, -1.000000000000000000, -0.000000000000000000 ) ) ;
#57829 = CARTESIAN_POINT ( 'NONE',  ( 6.675000001229034474, 2.886751345948126879, 4.999999999999999112 ) ) ;
#57830 = CARTESIAN_POINT ( 'NONE',  ( 8.334375000614516082, -4.541064518000419881, 2.621784821874995952 ) ) ;
#57831 = CARTESIAN_POINT ( 'NONE',  ( 26.44687500061451502, -3.027376345333610441, -5.243569643749999898 ) ) ;
#57832 = CARTESIAN_POINT ( 'NONE',  ( 15.37500000122903465, -5.773502691896255534, -1.060575238724906372E-15 ) ) ;
#57833 = CARTESIAN_POINT ( 'NONE',  ( 21.89062500061451289, -3.027376345333610441, -5.243569643749999898 ) ) ;
#57834 = CARTESIAN_POINT ( 'NONE',  ( 25.77187500061451075, 3.027376345333611329, 5.243569643749999010 ) ) ;
#57835 = CARTESIAN_POINT ( 'NONE',  ( 2.655984681222220721E-16, 16.01562499938548356, 25.66244784525396483 ) ) ;
#57836 = DIRECTION ( 'NONE',  ( 0.000000000000000000, 0.000000000000000000, -1.000000000000000000 ) ) ;
#57837 = CARTESIAN_POINT ( 'NONE',  ( 8.146875000614516082, 6.054752690667223547, 3.707466751127219781E-16 ) ) ;
#57838 = CARTESIAN_POINT ( 'NONE',  ( 19.90312500061451573, 0.000000000000000000, 5.243569643749999010 ) ) ;
#57839 = ORIENTED_EDGE ( 'NONE', *, *, #12677, .T. ) ;
#57840 = CARTESIAN_POINT ( 'NONE',  ( -2.000000000000000000, 12.72499999999999964, -33.46410161513775705 ) ) ;
#57841 = CARTESIAN_POINT ( 'NONE',  ( 28.41562500061451502, 3.027376345333611329, 5.243569643749999010 ) ) ;
#57842 = CARTESIAN_POINT ( 'NONE',  ( 3.084375000614519191, 6.421520780324663323E-16, -5.243569643749999010 ) ) ;
#57843 = LINE ( 'NONE', #28694, #53756 ) ;
#57844 = CARTESIAN_POINT ( 'NONE',  ( 3.688512509775060177, 3.375629639820296735, -3.780221722430626485 ) ) ;
#57845 = CARTESIAN_POINT ( 'NONE',  ( 15.93750000000000000, 5.773502691896255534, 3.535250795749688894E-16 ) ) ;
#57846 = CARTESIAN_POINT ( 'NONE',  ( 21.25312500061451715, 0.000000000000000000, 5.243569643749999010 ) ) ;
#57847 = ORIENTED_EDGE ( 'NONE', *, *, #70340, .F. ) ;
#57848 = CARTESIAN_POINT ( 'NONE',  ( 25.57499999999999929, -4.330127018922194537, 2.499999999999995559 ) ) ;
#57849 =( BOUNDED_CURVE ( )  B_SPLINE_CURVE ( 2, ( #62571, #59930, #37035, #70655, #65847, #47396, #37768, #43326, #30766 ),
 .UNSPECIFIED., .F., .F. ) 
 B_SPLINE_CURVE_WITH_KNOTS ( ( 3, 2, 2, 2, 3 ),
 ( 0.3369565217391304324, 0.3405797101449275499, 0.3478260869565217295, 0.3550724637681159646, 0.3586956521739130821 ),
 .UNSPECIFIED. ) 
 CURVE ( )  GEOMETRIC_REPRESENTATION_ITEM ( )  RATIONAL_B_SPLINE_CURVE ( ( 0.9330127018922194093, 0.9330127018922194093, 1.000000000000000000, 0.8660254037844387076, 1.000000000000000000, 0.8660254037844387076, 1.000000000000000000, 0.9330127018922188542, 0.9330127018922194093 ) ) 
 REPRESENTATION_ITEM ( '' )  );
#57850 = CARTESIAN_POINT ( 'NONE',  ( 26.03437500061451715, 6.421520780324663323E-16, -5.243569643749999010 ) ) ;
#57851 = ORIENTED_EDGE ( 'NONE', *, *, #8189, .T. ) ;
#57852 = CARTESIAN_POINT ( 'NONE',  ( 15.17812500061451608, 6.421520780324663323E-16, -5.243569643749999010 ) ) ;
#57853 = CARTESIAN_POINT ( 'NONE',  ( 4.978125000614518569, 4.541064518000418104, 2.621784821874999949 ) ) ;
#57854 = CARTESIAN_POINT ( 'NONE',  ( 18.04687500061451644, 0.000000000000000000, 4.756430356249998326 ) ) ;
#57855 = CARTESIAN_POINT ( 'NONE',  ( 28.97812500061451502, -4.541064518000419881, 2.621784821874995952 ) ) ;
#57856 = CARTESIAN_POINT ( 'NONE',  ( 15.22500000122903252, 2.886751345948126879, 4.999999999999999112 ) ) ;
#57857 = CARTESIAN_POINT ( 'NONE',  ( 20.69999999999999929, -4.330127018922190985, -2.500000000000001332 ) ) ;
#57858 = CARTESIAN_POINT ( 'NONE',  ( 28.16249999999999787, 2.886751345948126879, 4.999999999999999112 ) ) ;
#57859 = CARTESIAN_POINT ( 'NONE',  ( 4.509375000614518569, 4.541064518000418104, -2.621784821874998173 ) ) ;
#57860 = CARTESIAN_POINT ( 'NONE',  ( 9.271875000614516082, -6.054752690667223547, -1.112240025338166033E-15 ) ) ;
#57861 = CARTESIAN_POINT ( 'NONE',  ( 19.17187500061451999, -6.054752690667223547, -1.112240025338166033E-15 ) ) ;
#57862 = CARTESIAN_POINT ( 'NONE',  ( 11.53125000122903465, 4.330127018922191873, 2.499999999999999556 ) ) ;
#57863 = ORIENTED_EDGE ( 'NONE', *, *, #20206, .T. ) ;
#57864 = CARTESIAN_POINT ( 'NONE',  ( 29.05312500061451431, -4.541064518000417216, -2.621784821875001281 ) ) ;
#57865 = CARTESIAN_POINT ( 'NONE',  ( 3.037500000000002309, -2.886751345948129988, 4.999999999999997335 ) ) ;
#57866 = CARTESIAN_POINT ( 'NONE',  ( 4.134375000614517681, 4.541064518000418104, 2.621784821874999949 ) ) ;
#57867 = CARTESIAN_POINT ( 'NONE',  ( 18.03749999999999787, -2.886751345948125991, -5.000000000000000000 ) ) ;
#57868 = CARTESIAN_POINT ( 'NONE',  ( 13.94062500061451892, 6.054752690667223547, 3.707466751127219781E-16 ) ) ;
#57869 = CARTESIAN_POINT ( 'NONE',  ( -5.810221930991193690E-16, 14.15000000122903145, 26.00000000000000355 ) ) ;
#57870 = CARTESIAN_POINT ( 'NONE',  ( 45.00000000000000000, 0.000000000000000000, 0.000000000000000000 ) ) ;
#57871 = FACE_OUTER_BOUND ( 'NONE', #40946, .T. ) ;
#57872 = CARTESIAN_POINT ( 'NONE',  ( 20.25937500061451857, 4.119189519843966529, -2.378215178124998275 ) ) ;
#57873 = CARTESIAN_POINT ( 'NONE',  ( 7.903125000614515727, -4.541064518000417216, -2.621784821875001281 ) ) ;
#57874 = CARTESIAN_POINT ( 'NONE',  ( 24.49687500061451573, -3.027376345333614438, 5.243569643749998122 ) ) ;
#57875 = CARTESIAN_POINT ( 'NONE',  ( 2.121784821874999061, 18.35937500061451644, 26.32496088578401583 ) ) ;
#57876 = CARTESIAN_POINT ( 'NONE',  ( 26.89687500061451431, -3.027376345333610441, -5.243569643749999898 ) ) ;
#57877 = CARTESIAN_POINT ( 'NONE',  ( 6.524999999999999467, 4.330127018922191873, 2.499999999999999556 ) ) ;
#57878 = CARTESIAN_POINT ( 'NONE',  ( 1.999999999999998668, 13.21250000122903501, 26.53589838486224650 ) ) ;
#57879 = CARTESIAN_POINT ( 'NONE',  ( 15.40312500061451573, 0.000000000000000000, 5.243569643749999010 ) ) ;
#57880 = CARTESIAN_POINT ( 'NONE',  ( 6.112500001229034474, 4.330127018922192761, -2.499999999999997780 ) ) ;
#57881 = CARTESIAN_POINT ( 'NONE',  ( 17.67187500061451644, 3.027376345333611329, 5.243569643749999010 ) ) ;
#57882 = CARTESIAN_POINT ( 'NONE',  ( 11.40937500061451892, 0.000000000000000000, 5.243569643749999010 ) ) ;
#57883 = FACE_OUTER_BOUND ( 'NONE', #39002, .T. ) ;
#57884 = VERTEX_POINT ( 'NONE', #18360 ) ;
#57885 = CARTESIAN_POINT ( 'NONE',  ( 11.69062500061451360, 6.054752690667223547, 3.707466751127219781E-16 ) ) ;
#57886 = CARTESIAN_POINT ( 'NONE',  ( 34.99999999999999289, 2.500000000000000444, 3.499999999999999112 ) ) ;
#57887 = CARTESIAN_POINT ( 'NONE',  ( 23.47500000122903430, -5.773502691896255534, -1.060575238724906372E-15 ) ) ;
#57888 = CARTESIAN_POINT ( 'NONE',  ( 13.39687500061451608, -3.027376345333610441, -5.243569643749999898 ) ) ;
#57889 = CARTESIAN_POINT ( 'NONE',  ( 15.55312500061451608, -4.541064518000417216, -2.621784821875001281 ) ) ;
#57890 = CARTESIAN_POINT ( 'NONE',  ( 4.000000000000000000, 16.58750000000000213, -27.69059892324149885 ) ) ;
#57891 = CARTESIAN_POINT ( 'NONE',  ( 24.60937500061451644, -4.541064518000417216, -2.621784821875001281 ) ) ;
#57892 = DIRECTION ( 'NONE',  ( -0.000000000000000000, -1.000000000000000000, -0.000000000000000000 ) ) ;
#57893 = CARTESIAN_POINT ( 'NONE',  ( 12.07500000122903216, 2.886751345948126879, 4.999999999999999112 ) ) ;
#57894 = CARTESIAN_POINT ( 'NONE',  ( 4.406325135406961024, 3.605547266578323029, 3.755008945195253300 ) ) ;
#57895 = CARTESIAN_POINT ( 'NONE',  ( 22.70625000122903003, 4.330127018922192761, -2.499999999999997780 ) ) ;
#57896 = CARTESIAN_POINT ( 'NONE',  ( 4.243569643749999898, 16.44687500061451857, -27.54997392385601529 ) ) ;
#57897 = CARTESIAN_POINT ( 'NONE',  ( 18.83437500061451431, 6.421520780324663323E-16, -5.243569643749999010 ) ) ;
#57898 = CARTESIAN_POINT ( 'NONE',  ( 16.95000000122903216, 5.773502691896255534, 3.535250795749688894E-16 ) ) ;
#57899 = CARTESIAN_POINT ( 'NONE',  ( 12.38437500061451857, -4.541064518000419881, 2.621784821874995952 ) ) ;
#57900 = CYLINDRICAL_SURFACE ( 'NONE', #55959, 4.999999999999998224 ) ;
#57901 = CARTESIAN_POINT ( 'NONE',  ( 21.07500000122903572, 2.886751345948126879, 4.999999999999999112 ) ) ;
#57902 = CARTESIAN_POINT ( 'NONE',  ( 13.94062500061451892, 6.054752690667223547, 3.707466751127219781E-16 ) ) ;
#57903 = ORIENTED_EDGE ( 'NONE', *, *, #53191, .T. ) ;
#57904 = ORIENTED_EDGE ( 'NONE', *, *, #38881, .F. ) ;
#57905 = CARTESIAN_POINT ( 'NONE',  ( 17.21249999999999858, 2.886751345948129099, -4.999999999999998224 ) ) ;
#57906 = CARTESIAN_POINT ( 'NONE',  ( 4.648177544792955741E-15, 14.18750000000000000, 33.99999999999999289 ) ) ;
#57907 = LINE ( 'NONE', #36843, #56268 ) ;
#57908 = CARTESIAN_POINT ( 'NONE',  ( 15.15000000122903323, 5.773502691896255534, 3.535250795749688894E-16 ) ) ;
#57909 = CARTESIAN_POINT ( 'NONE',  ( 26.03437500061451715, 6.421520780324663323E-16, -5.243569643749999010 ) ) ;
#57910 = CARTESIAN_POINT ( 'NONE',  ( 19.19062500061452070, -3.027376345333610441, -5.243569643749999898 ) ) ;
#57911 = CARTESIAN_POINT ( 'NONE',  ( 23.09062500061451573, -3.027376345333614438, 5.243569643749998122 ) ) ;
#57912 = CARTESIAN_POINT ( 'NONE',  ( 29.43750000122903288, 6.123233995736764310E-16, -4.999999999999998224 ) ) ;
#57913 =( BOUNDED_CURVE ( )  B_SPLINE_CURVE ( 2, ( #19413, #41973, #19787, #64494, #30877, #53418, #2809 ),
 .UNSPECIFIED., .F., .F. ) 
 B_SPLINE_CURVE_WITH_KNOTS ( ( 3, 2, 2, 3 ),
 ( 0.1666666666666666852, 0.1694444444444444808, 0.1722222222222222487, 0.1750000000000000167 ),
 .UNSPECIFIED. ) 
 CURVE ( )  GEOMETRIC_REPRESENTATION_ITEM ( )  RATIONAL_B_SPLINE_CURVE ( ( 0.9999999999999986677, 0.8660254037844400399, 1.000000000000000000, 0.8660254037844387076, 1.000000000000000000, 0.8660254037844373753, 1.000000000000001332 ) ) 
 REPRESENTATION_ITEM ( '' )  );
#57914 = EDGE_CURVE ( 'NONE', #69502, #14839, #60226, .T. ) ;
#57915 = CARTESIAN_POINT ( 'NONE',  ( 27.59999999999999787, 4.330127018922192761, -2.499999999999997780 ) ) ;
#57916 = CYLINDRICAL_SURFACE ( 'NONE', #70202, 4.000000000000000000 ) ;
#57917 = CARTESIAN_POINT ( 'NONE',  ( 9.984375000614518214, 4.119189519843966529, 2.378215178124999607 ) ) ;
#57918 = FACE_OUTER_BOUND ( 'NONE', #4286, .T. ) ;
#57919 = CARTESIAN_POINT ( 'NONE',  ( 20.26875000122903359, -5.773502691896255534, -1.060575238724906372E-15 ) ) ;
#57920 = CARTESIAN_POINT ( 'NONE',  ( 4.243569643749999898, 15.54687500061451644, -27.54997392385601529 ) ) ;
#57921 = CARTESIAN_POINT ( 'NONE',  ( 7.237500001229035362, -4.330127018922194537, 2.499999999999995559 ) ) ;
#57922 = CARTESIAN_POINT ( 'NONE',  ( 5.212500000000002132, 2.886751345948126879, 4.999999999999999112 ) ) ;
#57923 = ADVANCED_FACE ( 'NONE', ( #3119 ), #64799, .F. ) ;
#57924 = CARTESIAN_POINT ( 'NONE',  ( 11.92500000000000071, 4.330127018922191873, 2.499999999999999556 ) ) ;
#57925 = CARTESIAN_POINT ( 'NONE',  ( 9.759375000614516793, -4.541064518000417216, -2.621784821875001281 ) ) ;
#57926 = CARTESIAN_POINT ( 'NONE',  ( 29.65312500061451573, 4.541064518000418104, -2.621784821874998173 ) ) ;
#57927 = CARTESIAN_POINT ( 'NONE',  ( -3.137519842735245283E-14, 12.91250000000000142, 34.00000000000000000 ) ) ;
#57928 = DIRECTION ( 'NONE',  ( -1.000000000000000000, -0.000000000000000000, -0.000000000000000000 ) ) ;
#57929 = CYLINDRICAL_SURFACE ( 'NONE', #37133, 4.999999999999998224 ) ;
#57930 = CARTESIAN_POINT ( 'NONE',  ( 8.334375000614516082, -4.541064518000419881, 2.621784821874995952 ) ) ;
#57931 = CARTESIAN_POINT ( 'NONE',  ( 11.22187500061451892, 3.027376345333613106, -5.243569643749998122 ) ) ;
#57932 = CARTESIAN_POINT ( 'NONE',  ( 6.337499999999998579, -2.886751345948125991, -5.000000000000000000 ) ) ;
#57933 = CARTESIAN_POINT ( 'NONE',  ( 4.243569643749999010, 14.21562500061459744, 27.54997392385601174 ) ) ;
#57934 = CARTESIAN_POINT ( 'NONE',  ( 3.593717626727911174, 25.10350949617167160, 28.22432905880962650 ) ) ;
#57935 = CARTESIAN_POINT ( 'NONE',  ( 5.587500000000003020, 5.773502691896255534, 3.535250795749688894E-16 ) ) ;
#57936 = CARTESIAN_POINT ( 'NONE',  ( 27.56250000122902932, -4.330127018922190985, -2.500000000000001332 ) ) ;
#57937 = CARTESIAN_POINT ( 'NONE',  ( 17.74687500061451928, -4.119189519843965641, -2.378215178125001383 ) ) ;
#57938 = CARTESIAN_POINT ( 'NONE',  ( 22.22812500061451502, -4.541064518000419881, 2.621784821874995952 ) ) ;
#57939 = CARTESIAN_POINT ( 'NONE',  ( 13.90312500061451750, 4.541064518000418104, -2.621784821874998173 ) ) ;
#57940 = CARTESIAN_POINT ( 'NONE',  ( 25.92187500061451644, 5.824947211148865298E-16, -4.756430356249998326 ) ) ;
#57941 = CARTESIAN_POINT ( 'NONE',  ( 8.671875000614518214, 3.027376345333611329, 5.243569643749999010 ) ) ;
#57942 = CARTESIAN_POINT ( 'NONE',  ( 27.29999999999999716, 0.000000000000000000, 4.999999999999998224 ) ) ;
#57943 = CARTESIAN_POINT ( 'NONE',  ( 21.41250000122903074, 4.330127018922192761, -2.499999999999997780 ) ) ;
#57944 = CARTESIAN_POINT ( 'NONE',  ( 22.68750000122903288, 6.123233995736764310E-16, -4.999999999999998224 ) ) ;
#57945 = CARTESIAN_POINT ( 'NONE',  ( 11.14687500061451608, -3.027376345333610441, -5.243569643749999898 ) ) ;
#57946 = CARTESIAN_POINT ( 'NONE',  ( 27.38437500061451857, 6.421520780324663323E-16, -5.243569643749999010 ) ) ;
#57947 = CARTESIAN_POINT ( 'NONE',  ( 3.271875000614519635, 3.027376345333611329, 5.243569643749999010 ) ) ;
#57948 = CARTESIAN_POINT ( 'NONE',  ( 22.17187500061451644, 3.027376345333611329, 5.243569643749999010 ) ) ;
#57949 = CARTESIAN_POINT ( 'NONE',  ( 11.93437500061451573, -4.541064518000419881, 2.621784821874995952 ) ) ;
#57950 = CARTESIAN_POINT ( 'NONE',  ( -3.756430356250001434, 17.51562499938548356, 32.16877607737301048 ) ) ;
#57951 = CARTESIAN_POINT ( 'NONE',  ( 26.58750000000000213, -2.886751345948125991, -5.000000000000000000 ) ) ;
#57952 = CARTESIAN_POINT ( 'NONE',  ( -3.756430356250000102, 20.06562499938548072, 30.00000000000000000 ) ) ;
#57953 = CARTESIAN_POINT ( 'NONE',  ( -2.121784821874999949, 11.68437500061451750, -33.67503911421598417 ) ) ;
#57954 = CARTESIAN_POINT ( 'NONE',  ( 27.00937500061451857, 4.119189519843966529, -2.378215178124998275 ) ) ;
#57955 = CARTESIAN_POINT ( 'NONE',  ( 14.72812500061451679, 6.421520780324663323E-16, -5.243569643749999010 ) ) ;
#57956 = CARTESIAN_POINT ( 'NONE',  ( 6.375000000000001776, 6.123233995736764310E-16, -4.999999999999998224 ) ) ;
#57957 = FACE_OUTER_BOUND ( 'NONE', #49256, .T. ) ;
#57958 = CARTESIAN_POINT ( 'NONE',  ( 15.90000000000000036, 4.330127018922192761, -2.499999999999997780 ) ) ;
#57959 = CARTESIAN_POINT ( 'NONE',  ( -3.999999999999997335, 19.25000000122903288, 32.30940107675850470 ) ) ;
#57960 = CARTESIAN_POINT ( 'NONE',  ( 15.11250000122903359, 4.330127018922192761, -2.499999999999997780 ) ) ;
#57961 = CARTESIAN_POINT ( 'NONE',  ( 23.93437500061451573, 4.541064518000418104, 2.621784821874999949 ) ) ;
#57962 = ORIENTED_EDGE ( 'NONE', *, *, #66859, .T. ) ;
#57963 = CARTESIAN_POINT ( 'NONE',  ( 19.45312500061451644, 0.000000000000000000, 5.243569643749999010 ) ) ;
#57964 = CARTESIAN_POINT ( 'NONE',  ( 19.65937500061451360, -4.541064518000417216, -2.621784821875001281 ) ) ;
#57965 = CARTESIAN_POINT ( 'NONE',  ( 4.837500000000001243, -2.886751345948129988, 4.999999999999997335 ) ) ;
#57966 = CARTESIAN_POINT ( 'NONE',  ( 7.528125000614515727, 6.421520780324663323E-16, -5.243569643749999010 ) ) ;
#57967 = CARTESIAN_POINT ( 'NONE',  ( 23.01562500061451644, 3.027376345333611329, 5.243569643749999010 ) ) ;
#57968 = CARTESIAN_POINT ( 'NONE',  ( 11.85937500061451644, 0.000000000000000000, 5.243569643749999010 ) ) ;
#57969 = CARTESIAN_POINT ( 'NONE',  ( 15.83437500061451608, 4.541064518000418104, 2.621784821874999949 ) ) ;
#57970 = CARTESIAN_POINT ( 'NONE',  ( 4.243569643749999010, 15.11562500061451608, 27.54997392385601174 ) ) ;
#57971 = CARTESIAN_POINT ( 'NONE',  ( 18.52500000122903145, -5.773502691896255534, -1.060575238724906372E-15 ) ) ;
#57972 = CARTESIAN_POINT ( 'NONE',  ( 12.83437500061451786, -4.119189519843968306, 2.378215178124996054 ) ) ;
#57973 = CARTESIAN_POINT ( 'NONE',  ( 10.11562500061451608, -6.054752690667223547, -1.112240025338166033E-15 ) ) ;
#57974 = CARTESIAN_POINT ( 'NONE',  ( 4.321875000614517681, -6.054752690667223547, -1.112240025338166033E-15 ) ) ;
#57975 = CARTESIAN_POINT ( 'NONE',  ( 28.41562500061451502, 3.027376345333611329, 5.243569643749999010 ) ) ;
#57976 = CARTESIAN_POINT ( 'NONE',  ( 26.37187500061451217, -6.054752690667223547, -1.112240025338166033E-15 ) ) ;
#57977 = CARTESIAN_POINT ( 'NONE',  ( 17.50312500061451715, 4.541064518000418104, -2.621784821874998173 ) ) ;
#57978 = CARTESIAN_POINT ( 'NONE',  ( 25.08750000122903145, 4.330127018922191873, 2.499999999999999556 ) ) ;
#57979 = CARTESIAN_POINT ( 'NONE',  ( 25.60312500061451502, 4.541064518000418104, -2.621784821874998173 ) ) ;
#57980 = CARTESIAN_POINT ( 'NONE',  ( 20.97187500061451715, -6.054752690667223547, -1.112240025338166033E-15 ) ) ;
#57981 = CARTESIAN_POINT ( 'NONE',  ( 15.25312500061451715, 4.541064518000418104, -2.621784821874998173 ) ) ;
#57982 = CARTESIAN_POINT ( 'NONE',  ( 4.243569643749999898, 16.93437500061451573, 30.00000000000000000 ) ) ;
#57983 = CARTESIAN_POINT ( 'NONE',  ( 21.92812500061451431, 6.421520780324663323E-16, -5.243569643749999010 ) ) ;
#57984 = CARTESIAN_POINT ( 'NONE',  ( 3.075000001229035718, 2.886751345948126879, 4.999999999999999112 ) ) ;
#57985 = VERTEX_POINT ( 'NONE', #65906 ) ;
#57986 = CARTESIAN_POINT ( 'NONE',  ( 24.89999999999999858, 4.330127018922192761, -2.499999999999997780 ) ) ;
#57987 = CARTESIAN_POINT ( 'NONE',  ( 3.999999999999999112, 12.12500000000000000, -30.00000000000000000 ) ) ;
#57988 = CARTESIAN_POINT ( 'NONE',  ( -3.756430356249999214, 19.24062499938548143, 27.83122392262697531 ) ) ;
#57989 = CARTESIAN_POINT ( 'NONE',  ( 28.86562500061451786, 3.027376345333611329, 5.243569643749999010 ) ) ;
#57990 = CARTESIAN_POINT ( 'NONE',  ( 6.890625000614516438, -3.027376345333614438, 5.243569643749998122 ) ) ;
#57991 = CARTESIAN_POINT ( 'NONE',  ( 21.26250000122903572, -4.330127018922190985, -2.500000000000001332 ) ) ;
#57992 = CARTESIAN_POINT ( 'NONE',  ( 26.27812500061451573, -4.541064518000419881, 2.621784821874995952 ) ) ;
#57993 = CARTESIAN_POINT ( 'NONE',  ( 4.650000001229035895, -2.886751345948125991, -5.000000000000000000 ) ) ;
#57994 = CARTESIAN_POINT ( 'NONE',  ( 24.67500000000000071, -4.330127018922194537, 2.499999999999995559 ) ) ;
#57995 = CARTESIAN_POINT ( 'NONE',  ( -3.999999999999999556, 15.12500000122903288, -32.30940107675850470 ) ) ;
#57996 = CARTESIAN_POINT ( 'NONE',  ( -3.137519842735245283E-14, 12.57500000122903572, 34.00000000000000000 ) ) ;
#57997 = CARTESIAN_POINT ( 'NONE',  ( 10.45312500061451644, 0.000000000000000000, 5.243569643749999010 ) ) ;
#57998 = ORIENTED_EDGE ( 'NONE', *, *, #44349, .F. ) ;
#57999 = EDGE_CURVE ( 'NONE', #25000, #29715, #38188, .T. ) ;
#58000 = CARTESIAN_POINT ( 'NONE',  ( 26.61562500061451786, 3.027376345333611329, 5.243569643749999010 ) ) ;
#58001 = CARTESIAN_POINT ( 'NONE',  ( 7.303125000614516082, 0.000000000000000000, 5.243569643749999010 ) ) ;
#58002 = CARTESIAN_POINT ( 'NONE',  ( 4.678125000614516971, -4.541064518000419881, 2.621784821874995952 ) ) ;
#58003 = CARTESIAN_POINT ( 'NONE',  ( 17.22187500061451715, 2.746126346562643317, 4.756430356249998326 ) ) ;
#58004 = CARTESIAN_POINT ( 'NONE',  ( 4.658538704007320064, -1.816114365443275425, 4.919044833179992082 ) ) ;
#58005 = CARTESIAN_POINT ( 'NONE',  ( 13.08750000000000036, -2.886751345948125991, -5.000000000000000000 ) ) ;
#58006 = CARTESIAN_POINT ( 'NONE',  ( 12.90937500061451537, -4.541064518000417216, -2.621784821875001281 ) ) ;
#58007 = CARTESIAN_POINT ( 'NONE',  ( 10.08750000122903323, 6.123233995736764310E-16, -4.999999999999998224 ) ) ;
#58008 = CARTESIAN_POINT ( 'NONE',  ( 16.28437500061452070, 4.541064518000418104, 2.621784821874999949 ) ) ;
#58009 = CARTESIAN_POINT ( 'NONE',  ( 16.57499999999999929, -4.330127018922194537, 2.499999999999995559 ) ) ;
#58010 = CARTESIAN_POINT ( 'NONE',  ( 7.734375000614517326, 4.541064518000418104, 2.621784821874999949 ) ) ;
#58011 = CARTESIAN_POINT ( 'NONE',  ( -4.243569643749997233, 10.84062500061451395, -27.54997392385601174 ) ) ;
#58012 = CARTESIAN_POINT ( 'NONE',  ( 1.999999999999998668, 16.69999999999999929, 26.53589838486224650 ) ) ;
#58013 = CARTESIAN_POINT ( 'NONE',  ( 22.73437500061451999, -2.746126346562641984, -4.756430356249999214 ) ) ;
#58014 = VERTEX_POINT ( 'NONE', #9754 ) ;
#58015 = CARTESIAN_POINT ( 'NONE',  ( 25.34062500061451217, -3.027376345333614438, 5.243569643749998122 ) ) ;
#58016 = CARTESIAN_POINT ( 'NONE',  ( 11.10000000000000142, 0.000000000000000000, 4.999999999999998224 ) ) ;
#58017 = CARTESIAN_POINT ( 'NONE',  ( 27.42187500061451644, 3.027376345333613106, -5.243569643749998122 ) ) ;
#58018 = CARTESIAN_POINT ( 'NONE',  ( 25.34999999999999787, 4.330127018922192761, -2.499999999999997780 ) ) ;
#58019 = CARTESIAN_POINT ( 'NONE',  ( 7.978125000614517681, 6.421520780324663323E-16, -5.243569643749999010 ) ) ;
#58020 = CARTESIAN_POINT ( 'NONE',  ( 24.72187500061451360, 4.119189519843966529, 2.378215178124999607 ) ) ;
#58021 = CARTESIAN_POINT ( 'NONE',  ( 17.59687500061451715, 6.054752690667223547, 3.707466751127219781E-16 ) ) ;
#58022 = CARTESIAN_POINT ( 'NONE',  ( 12.27187500061451608, -4.119189519843968306, 2.378215178124996054 ) ) ;
#58023 = CARTESIAN_POINT ( 'NONE',  ( 2.878125000614517592, -4.541064518000419881, 2.621784821874995952 ) ) ;
#58024 = CARTESIAN_POINT ( 'NONE',  ( 9.346875000614517148, -3.027376345333610441, -5.243569643749999898 ) ) ;
#58025 = ORIENTED_EDGE ( 'NONE', *, *, #21219, .F. ) ;
#58026 = CARTESIAN_POINT ( 'NONE',  ( 19.17187500061451999, -6.054752690667223547, -1.112240025338166033E-15 ) ) ;
#58027 = CARTESIAN_POINT ( 'NONE',  ( 3.360876423103621669, 3.702290849829691588, -3.360876423103621669 ) ) ;
#58028 = CARTESIAN_POINT ( 'NONE',  ( 26.25000000000000000, 4.330127018922192761, -2.499999999999997780 ) ) ;
#58029 = CARTESIAN_POINT ( 'NONE',  ( 29.29687500061451644, 6.054752690667223547, 3.707466751127219781E-16 ) ) ;
#58030 = CARTESIAN_POINT ( 'NONE',  ( 30.00000000000000000, 0.000000000000000000, 0.000000000000000000 ) ) ;
#58031 = CARTESIAN_POINT ( 'NONE',  ( 10.76250000000000107, -5.773502691896255534, -1.060575238724906372E-15 ) ) ;
#58032 = ORIENTED_EDGE ( 'NONE', *, *, #32425, .F. ) ;
#58033 = CARTESIAN_POINT ( 'NONE',  ( 11.47499999999999964, 4.330127018922191873, 2.499999999999999556 ) ) ;
#58034 = CARTESIAN_POINT ( 'NONE',  ( 10.73437500061451644, 5.492252693125287522, 3.363034840372157021E-16 ) ) ;
#58035 = CARTESIAN_POINT ( 'NONE',  ( 24.51562500061451289, -6.054752690667223547, -1.112240025338166033E-15 ) ) ;
#58036 = CARTESIAN_POINT ( 'NONE',  ( 13.91249999999999964, -5.773502691896255534, -1.060575238724906372E-15 ) ) ;
#58037 = CARTESIAN_POINT ( 'NONE',  ( 9.187500001229034652, 6.123233995736764310E-16, -4.999999999999998224 ) ) ;
#58038 = CARTESIAN_POINT ( 'NONE',  ( 6.965625000614518392, -6.054752690667223547, -1.112240025338166033E-15 ) ) ;
#58039 = CARTESIAN_POINT ( 'NONE',  ( 22.01249999999999574, -5.773502691896255534, -1.060575238724906372E-15 ) ) ;
#58040 = ADVANCED_FACE ( 'NONE', ( #3859 ), #53117, .T. ) ;
#58041 = CARTESIAN_POINT ( 'NONE',  ( 20.54062500061451502, -3.027376345333610441, -5.243569643749999898 ) ) ;
#58042 = LINE ( 'NONE', #7816, #21889 ) ;
#58043 = VECTOR ( 'NONE', #4295, 1000.000000000000000 ) ;
#58044 = CARTESIAN_POINT ( 'NONE',  ( 24.93750000122903288, 6.123233995736764310E-16, -4.999999999999998224 ) ) ;
#58045 = CARTESIAN_POINT ( 'NONE',  ( 3.756430356249998770, 17.10312499938548214, 32.16877607737301759 ) ) ;
#58046 = CARTESIAN_POINT ( 'NONE',  ( 6.262500000000000178, -5.773502691896255534, -1.060575238724906372E-15 ) ) ;
#58047 = ORIENTED_EDGE ( 'NONE', *, *, #3893, .T. ) ;
#58048 = CARTESIAN_POINT ( 'NONE',  ( 21.21562500061451573, 3.027376345333611329, 5.243569643749999010 ) ) ;
#58049 = CARTESIAN_POINT ( 'NONE',  ( 26.24062500061451431, -3.027376345333614438, 5.243569643749998122 ) ) ;
#58050 = CARTESIAN_POINT ( 'NONE',  ( 27.98437500061451289, 4.541064518000418104, 2.621784821874999949 ) ) ;
#58051 = CARTESIAN_POINT ( 'NONE',  ( 15.25312500061451715, 4.541064518000418104, -2.621784821874998173 ) ) ;
#58052 = CARTESIAN_POINT ( 'NONE',  ( 11.36249999999999716, 2.886751345948073588, -5.000000000000094147 ) ) ;
#58053 = CARTESIAN_POINT ( 'NONE',  ( 27.00000000122903288, -2.886751345948129988, 4.999999999999997335 ) ) ;
#58054 = CARTESIAN_POINT ( 'NONE',  ( 22.02187500061451786, 2.746126346562645981, -4.756430356249997438 ) ) ;
#58055 = CARTESIAN_POINT ( 'NONE',  ( 17.50312500061451715, 4.541064518000418104, -2.621784821874998173 ) ) ;
#58056 = CARTESIAN_POINT ( 'NONE',  ( 1.999999999999998668, 14.56250000122903288, -33.46410161513775705 ) ) ;
#58057 = CARTESIAN_POINT ( 'NONE',  ( 2.737500001229034474, -4.330127018922194537, 2.499999999999995559 ) ) ;
#58058 = CARTESIAN_POINT ( 'NONE',  ( 11.10937500061451644, -4.541064518000417216, -2.621784821875001281 ) ) ;
#58059 = CARTESIAN_POINT ( 'NONE',  ( 10.54687500061451644, -3.027376345333614438, 5.243569643749998122 ) ) ;
#58060 = CARTESIAN_POINT ( 'NONE',  ( 18.83437500061451431, 6.421520780324663323E-16, -5.243569643749999010 ) ) ;
#58061 = ORIENTED_EDGE ( 'NONE', *, *, #50010, .T. ) ;
#58062 = CARTESIAN_POINT ( 'NONE',  ( 9.975000000000001421, 6.123233995736764310E-16, -4.999999999999998224 ) ) ;
#58063 = CARTESIAN_POINT ( 'NONE',  ( 23.39062500061451289, 6.054752690667223547, 3.707466751127219781E-16 ) ) ;
#58064 = CARTESIAN_POINT ( 'NONE',  ( 19.24687500061452283, -3.027376345333610441, -5.243569643749999898 ) ) ;
#58065 = CARTESIAN_POINT ( 'NONE',  ( 23.46562500061451573, 3.027376345333611329, 5.243569643749999010 ) ) ;
#58066 = CARTESIAN_POINT ( 'NONE',  ( 4.000000000000000000, 14.78750000000000320, 32.30940107675849049 ) ) ;
#58067 = CARTESIAN_POINT ( 'NONE',  ( 2.971875000614517592, -6.054752690667223547, -1.112240025338166033E-15 ) ) ;
#58068 = CARTESIAN_POINT ( 'NONE',  ( 10.35000000122903074, -2.886751345948129988, 4.999999999999997335 ) ) ;
#58069 = CARTESIAN_POINT ( 'NONE',  ( 3.900000001229034563, 5.773502691896255534, 3.535250795749688894E-16 ) ) ;
#58070 = CARTESIAN_POINT ( 'NONE',  ( -1.999999999999997113, 19.62500000000000000, -26.53589838486224295 ) ) ;
#58071 = CARTESIAN_POINT ( 'NONE',  ( 26.17500000122903359, -5.773502691896255534, -1.060575238724906372E-15 ) ) ;
#58072 = CARTESIAN_POINT ( 'NONE',  ( -2.000000000000001776, 20.84374999877096357, 33.46410161513775705 ) ) ;
#58073 = ADVANCED_FACE ( 'NONE', ( #69012 ), #57900, .T. ) ;
#58074 = CARTESIAN_POINT ( 'NONE',  ( 10.28437500061451715, 6.421520780324663323E-16, -5.243569643749999010 ) ) ;
#58075 = CARTESIAN_POINT ( 'NONE',  ( 17.81250000000000355, 2.886751345948193936, 4.999999999999883649 ) ) ;
#58076 = CARTESIAN_POINT ( 'NONE',  ( 17.24062500061451786, -3.027376345333614438, 5.243569643749998122 ) ) ;
#58077 = CARTESIAN_POINT ( 'NONE',  ( 11.63437500061451857, 6.421520780324663323E-16, -5.243569643749999010 ) ) ;
#58078 = CARTESIAN_POINT ( 'NONE',  ( 29.13750000122903216, 4.330127018922191873, 2.499999999999999556 ) ) ;
#58079 = CARTESIAN_POINT ( 'NONE',  ( 19.69687500061451857, -3.027376345333610441, -5.243569643749999898 ) ) ;
#58080 = CARTESIAN_POINT ( 'NONE',  ( 6.796875000614516438, 6.054752690667223547, 3.707466751127219781E-16 ) ) ;
#58081 = CARTESIAN_POINT ( 'NONE',  ( 3.890625000614517326, -3.027376345333610441, -5.243569643749999898 ) ) ;
#58082 = CARTESIAN_POINT ( 'NONE',  ( 30.00000000000000000, 0.000000000000000000, 0.000000000000000000 ) ) ;
#58083 = CARTESIAN_POINT ( 'NONE',  ( 8.915625000614515017, 3.027376345333613106, -5.243569643749998122 ) ) ;
#58084 = CARTESIAN_POINT ( 'NONE',  ( 16.79062500061451857, -3.027376345333614438, 5.243569643749998122 ) ) ;
#58085 = ORIENTED_EDGE ( 'NONE', *, *, #40891, .F. ) ;
#58086 = CARTESIAN_POINT ( 'NONE',  ( 6.712500001229034119, 0.000000000000000000, 4.999999999999998224 ) ) ;
#58087 = CARTESIAN_POINT ( 'NONE',  ( 16.04062500061451857, -3.027376345333610441, -5.243569643749999898 ) ) ;
#58088 = CARTESIAN_POINT ( 'NONE',  ( 10.75312500061451715, 4.541064518000418104, -2.621784821874998173 ) ) ;
#58089 = CARTESIAN_POINT ( 'NONE',  ( 23.63437500061451502, -4.119189519843968306, 2.378215178124996054 ) ) ;
#58090 = CARTESIAN_POINT ( 'NONE',  ( 11.62500000000000000, -4.330127018922194537, 2.499999999999995559 ) ) ;
#58091 = CARTESIAN_POINT ( 'NONE',  ( 7.425000001229034474, 2.886751345948129099, -4.999999999999998224 ) ) ;
#58092 = ADVANCED_FACE ( 'NONE', ( #6591 ), #19662, .T. ) ;
#58093 = CARTESIAN_POINT ( 'NONE',  ( 14.78437500061451715, 6.421520780324663323E-16, -5.243569643749999010 ) ) ;
#58094 = AXIS2_PLACEMENT_3D ( 'NONE', #66553, #3413, #32207 ) ;
#58095 = CARTESIAN_POINT ( 'NONE',  ( 19.53750000122903430, 6.123233995736764310E-16, -4.999999999999998224 ) ) ;
#58096 = CARTESIAN_POINT ( 'NONE',  ( 24.22500000000000142, -4.330127018922194537, 2.499999999999995559 ) ) ;
#58097 = CARTESIAN_POINT ( 'NONE',  ( 2.121784821874999061, 17.85312500061451502, -33.67503911421598417 ) ) ;
#58098 = DIRECTION ( 'NONE',  ( -0.000000000000000000, -1.000000000000000000, -0.000000000000000000 ) ) ;
#58099 = DIRECTION ( 'NONE',  ( 0.000000000000000000, 0.000000000000000000, -1.000000000000000000 ) ) ;
#58100 =( BOUNDED_CURVE ( )  B_SPLINE_CURVE ( 2, ( #47989, #19153, #7727, #41707, #8093, #24710, #46530, #58316, #70517 ),
 .UNSPECIFIED., .F., .F. ) 
 B_SPLINE_CURVE_WITH_KNOTS ( ( 3, 2, 2, 2, 3 ),
 ( 0.6805555555555555802, 0.6851851851851852304, 0.6944444444444444198, 0.7037037037037037202, 0.7083333333333333703 ),
 .UNSPECIFIED. ) 
 CURVE ( )  GEOMETRIC_REPRESENTATION_ITEM ( )  RATIONAL_B_SPLINE_CURVE ( ( 0.9330127018922194093, 0.9330127018922194093, 1.000000000000000000, 0.8660254037844387076, 1.000000000000000000, 0.8660254037844387076, 1.000000000000000000, 0.9330127018922185211, 0.9330127018922192983 ) ) 
 REPRESENTATION_ITEM ( '' )  );
#58101 = DIRECTION ( 'NONE',  ( 0.000000000000000000, 0.000000000000000000, -1.000000000000000000 ) ) ;
#58102 = DIRECTION ( 'NONE',  ( 0.000000000000000000, 0.000000000000000000, 1.000000000000000000 ) ) ;
#58103 = CARTESIAN_POINT ( 'NONE',  ( 18.79687500061451644, -3.027376345333610441, -5.243569643749999898 ) ) ;
#58104 = CARTESIAN_POINT ( 'NONE',  ( 14.72812500061451679, 6.421520780324663323E-16, -5.243569643749999010 ) ) ;
#58105 = CARTESIAN_POINT ( 'NONE',  ( 8.943750001229034297, -2.886751345948129988, 4.999999999999997335 ) ) ;
#58106 = CARTESIAN_POINT ( 'NONE',  ( 22.57500000122903572, -5.773502691896255534, -1.060575238724906372E-15 ) ) ;
#58107 = CARTESIAN_POINT ( 'NONE',  ( 25.43437500061451573, -4.541064518000419881, 2.621784821874995952 ) ) ;
#58108 = CARTESIAN_POINT ( 'NONE',  ( 17.67187500061451644, -4.119189519843968306, 2.378215178124996054 ) ) ;
#58109 = CARTESIAN_POINT ( 'NONE',  ( 10.15312500061451750, -4.541064518000417216, -2.621784821875001281 ) ) ;
#58110 = CARTESIAN_POINT ( 'NONE',  ( 16.24687500061451573, 6.054752690667223547, 3.707466751127219781E-16 ) ) ;
#58111 = ORIENTED_EDGE ( 'NONE', *, *, #72508, .T. ) ;
#58112 = CARTESIAN_POINT ( 'NONE',  ( 27.70312500061451289, -4.541064518000417216, -2.621784821875001281 ) ) ;
#58113 = CARTESIAN_POINT ( 'NONE',  ( 19.49062500061451431, -3.027376345333614438, 5.243569643749998122 ) ) ;
#58114 = CARTESIAN_POINT ( 'NONE',  ( 3.999999999999999112, 13.13750000122903394, -30.00000000000000000 ) ) ;
#58115 = LINE ( 'NONE', #64030, #59645 ) ;
#58116 = CARTESIAN_POINT ( 'NONE',  ( 8.887499999999999289, -2.886751345948129988, 4.999999999999997335 ) ) ;
#58117 = CARTESIAN_POINT ( 'NONE',  ( 18.18750000122903288, 6.123233995736764310E-16, -4.999999999999998224 ) ) ;
#58118 = FACE_OUTER_BOUND ( 'NONE', #1946, .T. ) ;
#58119 = CARTESIAN_POINT ( 'NONE',  ( 10.58437500061451608, -2.746126346562642428, -4.756430356249999214 ) ) ;
#58120 = VERTEX_POINT ( 'NONE', #46129 ) ;
#58121 = CARTESIAN_POINT ( 'NONE',  ( 18.07499999999999929, 6.123233995736764310E-16, -4.999999999999998224 ) ) ;
#58122 = CARTESIAN_POINT ( 'NONE',  ( 20.62499999999999645, -4.330127018922194537, 2.499999999999995559 ) ) ;
#58123 = CARTESIAN_POINT ( 'NONE',  ( 19.39687500061451786, 6.054752690667223547, 3.707466751127219781E-16 ) ) ;
#58124 = CARTESIAN_POINT ( 'NONE',  ( 13.97812500061451679, 4.541064518000418104, 2.621784821874999949 ) ) ;
#58125 =( BOUNDED_CURVE ( )  B_SPLINE_CURVE ( 2, ( #42355, #41990, #59693, #8364, #9468, #36804, #31638 ),
 .UNSPECIFIED., .F., .F. ) 
 B_SPLINE_CURVE_WITH_KNOTS ( ( 3, 2, 2, 3 ),
 ( 0.1599999999999999756, 0.1633333333333333026, 0.1666666666666666019, 0.1699999999999999567 ),
 .UNSPECIFIED. ) 
 CURVE ( )  GEOMETRIC_REPRESENTATION_ITEM ( )  RATIONAL_B_SPLINE_CURVE ( ( 1.000000000000001332, 0.8660254037844377084, 1.000000000000000000, 0.8660254037844387076, 1.000000000000000000, 0.8660254037844409281, 0.9999999999999977796 ) ) 
 REPRESENTATION_ITEM ( '' )  );
#58126 = VERTEX_POINT ( 'NONE', #35393 ) ;
#58127 = CARTESIAN_POINT ( 'NONE',  ( 19.68750000000000000, -2.886751345948130876, 4.999999999999996447 ) ) ;
#58128 = CARTESIAN_POINT ( 'NONE',  ( 6.703125000614516438, 4.541064518000418104, -2.621784821874998173 ) ) ;
#58129 = DIRECTION ( 'NONE',  ( -1.000000000000000000, -0.000000000000000000, -0.000000000000000000 ) ) ;
#58130 = CARTESIAN_POINT ( 'NONE',  ( 11.25000000000000000, -4.330127018922190985, -2.500000000000001332 ) ) ;
#58131 = CARTESIAN_POINT ( 'NONE',  ( 28.32187500061451502, 4.119189519843966529, 2.378215178124999607 ) ) ;
#58132 = CARTESIAN_POINT ( 'NONE',  ( 2.121784821875001281, 17.70312500061451644, 33.67503911421598417 ) ) ;
#58133 = CARTESIAN_POINT ( 'NONE',  ( 29.69062500061451715, 6.054752690667223547, 3.707466751127219781E-16 ) ) ;
#58134 = CARTESIAN_POINT ( 'NONE',  ( 9.262499999999999289, 2.886751345948126879, 4.999999999999999112 ) ) ;
#58135 = CARTESIAN_POINT ( 'NONE',  ( 2.655984681222220721E-16, 18.15312499938548285, 25.66244784525396483 ) ) ;
#58136 = CARTESIAN_POINT ( 'NONE',  ( 26.48437500061451644, 6.421520780324663323E-16, -5.243569643749999010 ) ) ;
#58137 = VERTEX_POINT ( 'NONE', #41670 ) ;
#58138 = CARTESIAN_POINT ( 'NONE',  ( 21.96562500061451573, 3.027376345333613106, -5.243569643749998122 ) ) ;
#58139 = CARTESIAN_POINT ( 'NONE',  ( 22.13437500061451502, 4.541064518000418104, 2.621784821874999949 ) ) ;
#58140 = CARTESIAN_POINT ( 'NONE',  ( -4.243569643749999898, 17.55312500061459602, -30.00000000000000000 ) ) ;
#58141 = CARTESIAN_POINT ( 'NONE',  ( 5.728125000614515905, 6.421520780324663323E-16, -5.243569643749999010 ) ) ;
#58142 = CARTESIAN_POINT ( 'NONE',  ( 29.59687500061451715, -2.746126346562641984, -4.756430356249999214 ) ) ;
#58143 = CARTESIAN_POINT ( 'NONE',  ( 25.00312500061451715, -4.541064518000417216, -2.621784821875001281 ) ) ;
#58144 = CARTESIAN_POINT ( 'NONE',  ( 27.98437500061450933, -2.746126346562646425, 4.756430356249996549 ) ) ;
#58145 = CARTESIAN_POINT ( 'NONE',  ( 10.58437500061451964, -4.119189519843968306, 2.378215178124996054 ) ) ;
#58146 = CARTESIAN_POINT ( 'NONE',  ( 18.04687500061451999, 6.054752690667223547, 3.707466751127219781E-16 ) ) ;
#58147 = ADVANCED_FACE ( 'NONE', ( #53113 ), #29497, .T. ) ;
#58148 = CARTESIAN_POINT ( 'NONE',  ( 19.35937500061451644, 4.541064518000418104, -2.621784821874998173 ) ) ;
#58149 = CARTESIAN_POINT ( 'NONE',  ( 26.14687500061451431, 6.054752690667223547, 3.707466751127219781E-16 ) ) ;
#58150 = CARTESIAN_POINT ( 'NONE',  ( 9.001249775931846008E-16, 15.92187500061451821, 34.90005215228797653 ) ) ;
#58151 = CARTESIAN_POINT ( 'NONE',  ( 7.678125000614516082, 4.541064518000418104, 2.621784821874999949 ) ) ;
#58152 = CARTESIAN_POINT ( 'NONE',  ( -1.487416814333745711E-14, 16.06250000000000000, 34.00000000000000000 ) ) ;
#58153 = CARTESIAN_POINT ( 'NONE',  ( 4.471875000614518925, 3.027376345333613106, -5.243569643749998122 ) ) ;
#58154 = CARTESIAN_POINT ( 'NONE',  ( 1.071796769724491227, 17.54240381056766651, 26.00000000000000000 ) ) ;
#58155 =( BOUNDED_CURVE ( )  B_SPLINE_CURVE ( 2, ( #21040, #21765, #67224, #60557, #15858, #9964, #16585, #32502, #4795 ),
 .UNSPECIFIED., .F., .F. ) 
 B_SPLINE_CURVE_WITH_KNOTS ( ( 3, 2, 2, 2, 3 ),
 ( 0.8152173913043478937, 0.8188405797101449002, 0.8260869565217391353, 0.8333333333333333703, 0.8369565217391304879 ),
 .UNSPECIFIED. ) 
 CURVE ( )  GEOMETRIC_REPRESENTATION_ITEM ( )  RATIONAL_B_SPLINE_CURVE ( ( 0.9330127018922192983, 0.9330127018922202975, 1.000000000000000000, 0.8660254037844387076, 1.000000000000000000, 0.8660254037844387076, 1.000000000000000000, 0.9330127018922182991, 0.9330127018922192983 ) ) 
 REPRESENTATION_ITEM ( '' )  );
#58156 = CARTESIAN_POINT ( 'NONE',  ( 5.840625000614516615, 6.054752690667223547, 3.707466751127219781E-16 ) ) ;
#58157 = CARTESIAN_POINT ( 'NONE',  ( 10.05937500061451750, 0.000000000000000000, 5.243569643749999010 ) ) ;
#58158 = CARTESIAN_POINT ( 'NONE',  ( 15.90000000122903501, -2.886751345948125991, -5.000000000000000000 ) ) ;
#58159 = CARTESIAN_POINT ( 'NONE',  ( 4.471875000614518925, 3.027376345333613106, -5.243569643749998122 ) ) ;
#58160 = CARTESIAN_POINT ( 'NONE',  ( 8.653125000614515727, 0.000000000000000000, 5.243569643749999010 ) ) ;
#58161 = CARTESIAN_POINT ( 'NONE',  ( -2.000000000000001776, 13.64374999877096784, 33.46410161513775705 ) ) ;
#58162 = CARTESIAN_POINT ( 'NONE',  ( 23.64375000122903003, 5.773502691896255534, 3.535250795749688894E-16 ) ) ;
#58163 = CARTESIAN_POINT ( 'NONE',  ( 15.90937500061451892, 0.000000000000000000, 5.243569643749999010 ) ) ;
#58164 = CARTESIAN_POINT ( 'NONE',  ( -3.999999999999997335, 10.58750000000000213, 32.30940107675850470 ) ) ;
#58165 = ORIENTED_EDGE ( 'NONE', *, *, #39715, .F. ) ;
#58166 = CARTESIAN_POINT ( 'NONE',  ( 24.14062500061451289, -3.027376345333610441, -5.243569643749999898 ) ) ;
#58167 = CARTESIAN_POINT ( 'NONE',  ( 9.703125000614514661, -4.541064518000417216, -2.621784821875001281 ) ) ;
#58168 = CARTESIAN_POINT ( 'NONE',  ( 26.59687500061451360, 6.054752690667223547, 3.707466751127219781E-16 ) ) ;
#58169 = CARTESIAN_POINT ( 'NONE',  ( 8.915625000614515017, 3.027376345333613106, -5.243569643749998122 ) ) ;
#58170 = CARTESIAN_POINT ( 'NONE',  ( 3.756430356250000102, 12.64062499938548356, 30.00000000000000000 ) ) ;
#58171 = CARTESIAN_POINT ( 'NONE',  ( 11.66250000122903430, 0.000000000000000000, 4.999999999999998224 ) ) ;
#58172 = CARTESIAN_POINT ( 'NONE',  ( 24.29062500061451502, 6.054752690667223547, 3.707466751127219781E-16 ) ) ;
#58173 = CARTESIAN_POINT ( 'NONE',  ( 2.121784821875001281, 12.75312500061451715, -26.32496088578401938 ) ) ;
#58174 = CARTESIAN_POINT ( 'NONE',  ( 13.95000000122903572, -2.886751345948129988, 4.999999999999997335 ) ) ;
#58175 = CARTESIAN_POINT ( 'NONE',  ( 21.96562500061451573, 3.027376345333613106, -5.243569643749998122 ) ) ;
#58176 = CARTESIAN_POINT ( 'NONE',  ( 10.53750000000000320, 5.773502691896255534, 3.535250795749688894E-16 ) ) ;
#58177 = CARTESIAN_POINT ( 'NONE',  ( 21.17812500061451431, 4.541064518000418104, 2.621784821874999949 ) ) ;
#58178 = CARTESIAN_POINT ( 'NONE',  ( 5.971875000614517148, 3.027376345333611329, 5.243569643749999010 ) ) ;
#58179 = CARTESIAN_POINT ( 'NONE',  ( 20.06250000000000000, 2.886751345948126879, 4.999999999999999112 ) ) ;
#58180 = CARTESIAN_POINT ( 'NONE',  ( 13.68750000122903288, 6.123233995736764310E-16, -4.999999999999998224 ) ) ;
#58181 = EDGE_CURVE ( 'NONE', #1580, #55986, #49899, .T. ) ;
#58182 = CARTESIAN_POINT ( 'NONE',  ( 10.94062500061451537, -3.027376345333614438, 5.243569643749998122 ) ) ;
#58183 = CARTESIAN_POINT ( 'NONE',  ( 13.71562500061451750, -6.054752690667223547, -1.112240025338166033E-15 ) ) ;
#58184 = CARTESIAN_POINT ( 'NONE',  ( 26.17500000122903359, -5.773502691896255534, -1.060575238724906372E-15 ) ) ;
#58185 = CARTESIAN_POINT ( 'NONE',  ( 21.34687500061451715, -3.027376345333614438, 5.243569643749998122 ) ) ;
#58186 = CARTESIAN_POINT ( 'NONE',  ( 25.50000000000000000, 0.000000000000000000, 4.999999999999998224 ) ) ;
#58187 = EDGE_CURVE ( 'NONE', #33928, #31017, #6286, .T. ) ;
#58188 = CARTESIAN_POINT ( 'NONE',  ( 8.925000001229033586, 2.886751345948126879, 4.999999999999999112 ) ) ;
#58189 = EDGE_CURVE ( 'NONE', #18641, #3838, #46857, .T. ) ;
#58190 = CARTESIAN_POINT ( 'NONE',  ( 8.484375000614518214, 6.421520780324663323E-16, -5.243569643749999010 ) ) ;
#58191 = CARTESIAN_POINT ( 'NONE',  ( 24.45937500061451786, 0.000000000000000000, 5.243569643749999010 ) ) ;
#58192 = CARTESIAN_POINT ( 'NONE',  ( 4.494741915665277254, -2.190272839526016924, 4.494741915664858922 ) ) ;
#58193 = CARTESIAN_POINT ( 'NONE',  ( 22.41562500061451502, 3.027376345333613106, -5.243569643749998122 ) ) ;
#58194 = CARTESIAN_POINT ( 'NONE',  ( 26.40937500061451715, -4.541064518000417216, -2.621784821875001281 ) ) ;
#58195 = CARTESIAN_POINT ( 'NONE',  ( -1.878215178125001827, 16.20312499938548356, 33.25316411605952283 ) ) ;
#58196 = CARTESIAN_POINT ( 'NONE',  ( 19.48125000122903216, 6.123233995736764310E-16, -4.999999999999998224 ) ) ;
#58197 = CARTESIAN_POINT ( 'NONE',  ( 7.996875000614519280, -3.027376345333610441, -5.243569643749999898 ) ) ;
#58198 = CARTESIAN_POINT ( 'NONE',  ( 17.42812500061451786, 6.421520780324663323E-16, -5.243569643749999010 ) ) ;
#58199 = VERTEX_POINT ( 'NONE', #35035 ) ;
#58200 = CARTESIAN_POINT ( 'NONE',  ( 12.73125000122903394, 6.123233995736764310E-16, -4.999999999999998224 ) ) ;
#58201 = CARTESIAN_POINT ( 'NONE',  ( 27.77812500061451573, 6.421520780324663323E-16, -5.243569643749999010 ) ) ;
#58202 = CARTESIAN_POINT ( 'NONE',  ( 3.309375000614518836, 0.000000000000000000, 5.243569643749999010 ) ) ;
#58203 = CARTESIAN_POINT ( 'NONE',  ( 4.633613603196540254, 1.878729617659674167, 4.895446622381335544 ) ) ;
#58204 = CARTESIAN_POINT ( 'NONE',  ( 0.000000000000000000, 20.00000000000000000, 26.00000000000000000 ) ) ;
#58205 = CARTESIAN_POINT ( 'NONE',  ( 17.39999999999999858, 0.000000000000000000, 4.999999999999998224 ) ) ;
#58206 = CARTESIAN_POINT ( 'NONE',  ( 20.87812500061451715, -4.541064518000419881, 2.621784821874995952 ) ) ;
#58207 = EDGE_LOOP ( 'NONE', ( #2021, #20285, #46691, #34287 ) ) ;
#58208 = CARTESIAN_POINT ( 'NONE',  ( 25.68750000000000000, -2.886751345948125991, -5.000000000000000000 ) ) ;
#58209 = CARTESIAN_POINT ( 'NONE',  ( 25.58437500061451431, 6.421520780324663323E-16, -5.243569643749999010 ) ) ;
#58210 = ORIENTED_EDGE ( 'NONE', *, *, #25488, .T. ) ;
#58211 = CARTESIAN_POINT ( 'NONE',  ( 13.64062500061451644, -3.027376345333614438, 5.243569643749998122 ) ) ;
#58212 = CARTESIAN_POINT ( 'NONE',  ( 5.240625000614516971, -3.027376345333610441, -5.243569643749999898 ) ) ;
#58213 = CARTESIAN_POINT ( 'NONE',  ( 15.75937500061451502, 2.746126346562643317, 4.756430356249998326 ) ) ;
#58214 = CARTESIAN_POINT ( 'NONE',  ( 3.271875000614519635, 3.027376345333611329, 5.243569643749999010 ) ) ;
#58215 = CARTESIAN_POINT ( 'NONE',  ( 15.26250000122903216, 0.000000000000000000, 4.999999999999998224 ) ) ;
#58216 = CARTESIAN_POINT ( 'NONE',  ( 20.06250000000000000, 2.886751345948126879, 4.999999999999999112 ) ) ;
#58217 = CARTESIAN_POINT ( 'NONE',  ( 28.68749999999999645, -2.886751345948129988, 4.999999999999997335 ) ) ;
#58218 = CARTESIAN_POINT ( 'NONE',  ( 3.796875000614517326, -3.027376345333614438, 5.243569643749998122 ) ) ;
#58219 = CARTESIAN_POINT ( 'NONE',  ( 10.13437500061451679, -4.541064518000419881, 2.621784821874995952 ) ) ;
#58220 = CARTESIAN_POINT ( 'NONE',  ( 18.34687500061451715, -3.027376345333610441, -5.243569643749999898 ) ) ;
#58221 = CARTESIAN_POINT ( 'NONE',  ( -1.071796769724485010, 17.39240381056766083, -25.99999999999999289 ) ) ;
#58222 = ORIENTED_EDGE ( 'NONE', *, *, #28401, .T. ) ;
#58223 = CARTESIAN_POINT ( 'NONE',  ( 28.52812500061451573, -4.541064518000419881, 2.621784821874995952 ) ) ;
#58224 = CARTESIAN_POINT ( 'NONE',  ( 3.262500000000001510, 2.886751345948129099, -4.999999999999998224 ) ) ;
#58225 = EDGE_CURVE ( 'NONE', #30519, #29484, #64563, .T. ) ;
#58226 = CARTESIAN_POINT ( 'NONE',  ( 3.909375000614518481, -4.541064518000417216, -2.621784821875001281 ) ) ;
#58227 = CARTESIAN_POINT ( 'NONE',  ( 16.87500000000000000, 4.330127018922191873, 2.499999999999999556 ) ) ;
#58228 = CARTESIAN_POINT ( 'NONE',  ( 14.84062500061451750, 6.054752690667223547, 3.707466751127219781E-16 ) ) ;
#58229 = CARTESIAN_POINT ( 'NONE',  ( 1.999999999999997335, 19.17500000000000071, 33.46410161513775705 ) ) ;
#58230 = CARTESIAN_POINT ( 'NONE',  ( 17.90625000122903288, 0.000000000000000000, 4.999999999999998224 ) ) ;
#58231 = CARTESIAN_POINT ( 'NONE',  ( 18.41250000122903430, 0.000000000000000000, 4.999999999999998224 ) ) ;
#58232 = CARTESIAN_POINT ( 'NONE',  ( 0.000000000000000000, 10.00000000000000000, 24.00000000000000000 ) ) ;
#58233 = CARTESIAN_POINT ( 'NONE',  ( 20.48437500061451289, -4.119189519843968306, 2.378215178124996054 ) ) ;
#58234 = CARTESIAN_POINT ( 'NONE',  ( 6.515625000614516438, -6.054752690667223547, -1.112240025338166033E-15 ) ) ;
#58235 = CARTESIAN_POINT ( 'NONE',  ( 24.38437500061451502, 4.541064518000418104, 2.621784821874999949 ) ) ;
#58236 = CARTESIAN_POINT ( 'NONE',  ( -4.243569643749999898, 19.40937500061451715, 30.00000000000000000 ) ) ;
#58237 = CARTESIAN_POINT ( 'NONE',  ( 25.58437500061451431, 6.421520780324663323E-16, -5.243569643749999010 ) ) ;
#58238 = CARTESIAN_POINT ( 'NONE',  ( 7.462500000000001243, 2.886751345948126879, 4.999999999999999112 ) ) ;
#58239 = CARTESIAN_POINT ( 'NONE',  ( -2.000000000000000000, 12.83750000122903501, 26.53589838486224650 ) ) ;
#58240 = CARTESIAN_POINT ( 'NONE',  ( 13.94062500061451892, 6.054752690667223547, 3.707466751127219781E-16 ) ) ;
#58241 = CARTESIAN_POINT ( 'NONE',  ( 7.687500001229033764, -4.330127018922194537, 2.499999999999995559 ) ) ;
#58242 = CARTESIAN_POINT ( 'NONE',  ( 18.68437500061451928, -4.541064518000419881, 2.621784821874995952 ) ) ;
#58243 = CARTESIAN_POINT ( 'NONE',  ( 12.72187500061451537, 3.027376345333611329, 5.243569643749999010 ) ) ;
#58244 = CYLINDRICAL_SURFACE ( 'NONE', #57204, 4.999999999999998224 ) ;
#58245 = EDGE_LOOP ( 'NONE', ( #4695, #71340, #66339, #8766 ) ) ;
#58246 = CARTESIAN_POINT ( 'NONE',  ( 13.07812500061451821, 4.541064518000418104, 2.621784821874999949 ) ) ;
#58247 = PLANE ( 'NONE',  #54427 ) ;
#58248 = CARTESIAN_POINT ( 'NONE',  ( 22.98750000122903003, -4.330127018922194537, 2.499999999999995559 ) ) ;
#58249 = CARTESIAN_POINT ( 'NONE',  ( 13.28437500061451715, -4.541064518000419881, 2.621784821874995952 ) ) ;
#58250 = CARTESIAN_POINT ( 'NONE',  ( 14.72812500061451679, 6.421520780324663323E-16, -5.243569643749999010 ) ) ;
#58251 = CARTESIAN_POINT ( 'NONE',  ( 24.75937500061451502, 4.541064518000418104, -2.621784821874998173 ) ) ;
#58252 = DIRECTION ( 'NONE',  ( -0.000000000000000000, -1.000000000000000000, -0.000000000000000000 ) ) ;
#58253 = CARTESIAN_POINT ( 'NONE',  ( 7.612500000000000711, -5.773502691896255534, -1.060575238724906372E-15 ) ) ;
#58254 = CARTESIAN_POINT ( 'NONE',  ( 22.74375000122903145, 5.773502691896255534, 3.535250795749688401E-16 ) ) ;
#58255 = CARTESIAN_POINT ( 'NONE',  ( -4.243569643749999898, 16.67187500061451644, -32.45002607614398471 ) ) ;
#58256 = CARTESIAN_POINT ( 'NONE',  ( 16.13437500061451502, 6.421520780324663323E-16, -5.243569643749999010 ) ) ;
#58257 = CARTESIAN_POINT ( 'NONE',  ( 18.03750000122903430, -4.330127018922194537, 2.499999999999995559 ) ) ;
#58258 = CARTESIAN_POINT ( 'NONE',  ( 12.79687500061451821, -3.027376345333614438, 5.243569643749998122 ) ) ;
#58259 = CARTESIAN_POINT ( 'NONE',  ( 4.243569643749999898, 19.12812500061451715, -30.00000000000000000 ) ) ;
#58260 = CARTESIAN_POINT ( 'NONE',  ( 20.21250000122903145, 0.000000000000000000, 4.999999999999998224 ) ) ;
#58261 = CARTESIAN_POINT ( 'NONE',  ( 13.11562500061451786, 3.027376345333611329, 5.243569643749999010 ) ) ;
#58262 = AXIS2_PLACEMENT_3D ( 'NONE', #62180, #15643, #63614 ) ;
#58263 = ORIENTED_EDGE ( 'NONE', *, *, #61088, .F. ) ;
#58264 = ORIENTED_EDGE ( 'NONE', *, *, #10064, .T. ) ;
#58265 = CARTESIAN_POINT ( 'NONE',  ( 17.96250000000000213, -5.773502691896255534, -1.060575238724906372E-15 ) ) ;
#58266 = CARTESIAN_POINT ( 'NONE',  ( -1.243387493232115393E-14, 15.70624999877096784, 26.00000000000000000 ) ) ;
#58267 = CARTESIAN_POINT ( 'NONE',  ( 12.04687500061451821, -3.027376345333610441, -5.243569643749999898 ) ) ;
#58268 = FACE_OUTER_BOUND ( 'NONE', #20666, .T. ) ;
#58269 = CARTESIAN_POINT ( 'NONE',  ( 13.50000000122903288, -2.886751345948129988, 4.999999999999997335 ) ) ;
#58270 = CARTESIAN_POINT ( 'NONE',  ( 21.52500000122903145, 2.886751345948126879, 4.999999999999999112 ) ) ;
#58271 = CARTESIAN_POINT ( 'NONE',  ( 16.56562500061451715, 3.027376345333613106, -5.243569643749998122 ) ) ;
#58272 = CARTESIAN_POINT ( 'NONE',  ( 23.20312500061451644, -4.541064518000417216, -2.621784821875001281 ) ) ;
#58273 = CARTESIAN_POINT ( 'NONE',  ( 3.403125000614518836, -4.541064518000417216, -2.621784821875001281 ) ) ;
#58274 = CARTESIAN_POINT ( 'NONE',  ( 28.08749999999999858, 5.773502691896255534, 3.535250795749688894E-16 ) ) ;
#58275 = FACE_OUTER_BOUND ( 'NONE', #9533, .T. ) ;
#58276 = CARTESIAN_POINT ( 'NONE',  ( 29.17500000000000071, -4.330127018922194537, 2.499999999999995559 ) ) ;
#58277 = CARTESIAN_POINT ( 'NONE',  ( 1.071796769724491227, 17.99240381056766935, 26.00000000000000000 ) ) ;
#58278 = CARTESIAN_POINT ( 'NONE',  ( 1.071796769724489895, 14.46740381056766545, -34.00000000000000000 ) ) ;
#58279 = CARTESIAN_POINT ( 'NONE',  ( -2.121784821874996840, 15.88437500061451857, -26.32496088578401583 ) ) ;
#58280 = CARTESIAN_POINT ( 'NONE',  ( 4.012500001229033053, 0.000000000000000000, 4.999999999999998224 ) ) ;
#58281 = CARTESIAN_POINT ( 'NONE',  ( 7.124999999999999112, -4.330127018922194537, 2.499999999999995559 ) ) ;
#58282 =( BOUNDED_CURVE ( )  B_SPLINE_CURVE ( 2, ( #10692, #26967, #33223, #5155, #44327, #72025, #27690, #66856, #22138 ),
 .UNSPECIFIED., .F., .F. ) 
 B_SPLINE_CURVE_WITH_KNOTS ( ( 3, 2, 2, 2, 3 ),
 ( 0.09782608695652174335, 0.1014492753623188470, 0.1086956521739130405, 0.1159420289855072478, 0.1195652173913043514 ),
 .UNSPECIFIED. ) 
 CURVE ( )  GEOMETRIC_REPRESENTATION_ITEM ( )  RATIONAL_B_SPLINE_CURVE ( ( 0.9330127018922194093, 0.9330127018922194093, 1.000000000000000000, 0.8660254037844387076, 1.000000000000000000, 0.8660254037844387076, 1.000000000000000000, 0.9330127018922194093, 0.9330127018922194093 ) ) 
 REPRESENTATION_ITEM ( '' )  );
#58283 = CARTESIAN_POINT ( 'NONE',  ( 2.700000001229035718, -2.886751345948129988, 4.999999999999997335 ) ) ;
#58284 = CARTESIAN_POINT ( 'NONE',  ( 10.88437500061451679, 4.541064518000418104, 2.621784821874999949 ) ) ;
#58285 = CARTESIAN_POINT ( 'NONE',  ( 27.32812500061451644, 6.421520780324663323E-16, -5.243569643749999010 ) ) ;
#58286 = DIRECTION ( 'NONE',  ( -1.000000000000000000, -0.000000000000000000, -0.000000000000000000 ) ) ;
#58287 = CARTESIAN_POINT ( 'NONE',  ( 45.00000000000000000, -1.494782592887718531, -8.874999999999992895 ) ) ;
#58288 = FACE_OUTER_BOUND ( 'NONE', #41714, .T. ) ;
#58289 = CARTESIAN_POINT ( 'NONE',  ( 7.434375000614519280, -4.541064518000419881, 2.621784821874995952 ) ) ;
#58290 = CARTESIAN_POINT ( 'NONE',  ( 12.15937500061451892, 4.541064518000418104, -2.621784821874998173 ) ) ;
#58291 = EDGE_CURVE ( 'NONE', #69560, #11634, #25290, .T. ) ;
#58292 = CARTESIAN_POINT ( 'NONE',  ( 6.862500000000002487, 2.886751345948129099, -4.999999999999998224 ) ) ;
#58293 = CARTESIAN_POINT ( 'NONE',  ( 2.121784821874999061, 15.15312500061459566, 26.32496088578401583 ) ) ;
#58294 = CARTESIAN_POINT ( 'NONE',  ( 3.999999999999999112, 17.97500000000000142, 30.00000000000000000 ) ) ;
#58295 = CARTESIAN_POINT ( 'NONE',  ( 6.562500000000001776, 2.886751345948126879, 4.999999999999999112 ) ) ;
#58296 = CARTESIAN_POINT ( 'NONE',  ( 14.97187500061451537, -4.119189519843968306, 2.378215178124996054 ) ) ;
#58297 = CARTESIAN_POINT ( 'NONE',  ( 19.19062500061452070, -3.027376345333610441, -5.243569643749999898 ) ) ;
#58298 = CARTESIAN_POINT ( 'NONE',  ( 13.64062500061451644, -3.027376345333614438, 5.243569643749998122 ) ) ;
#58299 = CARTESIAN_POINT ( 'NONE',  ( 24.72187500061451360, 4.119189519843966529, 2.378215178124999607 ) ) ;
#58300 = CARTESIAN_POINT ( 'NONE',  ( 10.43437500061451750, 4.541064518000418104, 2.621784821874999949 ) ) ;
#58301 = CARTESIAN_POINT ( 'NONE',  ( 25.91250000000000142, 2.886751345948126879, 4.999999999999999112 ) ) ;
#58302 = CARTESIAN_POINT ( 'NONE',  ( 22.98750000122903003, -4.330127018922194537, 2.499999999999995559 ) ) ;
#58303 = CARTESIAN_POINT ( 'NONE',  ( 65.00000000000000000, 9.426999614876460059E-14, 7.499999999999999112 ) ) ;
#58304 = CARTESIAN_POINT ( 'NONE',  ( 12.75937500061451857, 0.000000000000000000, 5.243569643749999010 ) ) ;
#58305 = CARTESIAN_POINT ( 'NONE',  ( 27.49687500061451217, 6.054752690667223547, 3.707466751127219781E-16 ) ) ;
#58306 = DIRECTION ( 'NONE',  ( 1.000000000000000000, 0.000000000000000000, -0.000000000000000000 ) ) ;
#58307 = CARTESIAN_POINT ( 'NONE',  ( 21.12187500061451573, 3.027376345333613106, -5.243569643749998122 ) ) ;
#58308 = CARTESIAN_POINT ( 'NONE',  ( 11.52187500061451608, -6.054752690667223547, -1.112240025338166033E-15 ) ) ;
#58309 = CARTESIAN_POINT ( 'NONE',  ( 3.756430356249998770, 19.01562499938548356, 32.16877607737302469 ) ) ;
#58310 = CARTESIAN_POINT ( 'NONE',  ( 23.69999999999999929, 0.000000000000000000, 4.999999999999998224 ) ) ;
#58311 = CARTESIAN_POINT ( 'NONE',  ( 1.878215178125000495, 19.91562499938548569, 26.74683588394047007 ) ) ;
#58312 = CARTESIAN_POINT ( 'NONE',  ( 4.243569643749999898, 11.04687500061451999, -27.54997392385601529 ) ) ;
#58313 = CARTESIAN_POINT ( 'NONE',  ( 27.94687500061451502, 5.492252693125287522, 3.363034840372157021E-16 ) ) ;
#58314 = CARTESIAN_POINT ( 'NONE',  ( 14.57812500061451644, -4.541064518000419881, 2.621784821874995952 ) ) ;
#58315 = CARTESIAN_POINT ( 'NONE',  ( 4.724999999999999645, 4.330127018922191873, 2.499999999999999556 ) ) ;
#58316 = CARTESIAN_POINT ( 'NONE',  ( -1.071796769724480347, 18.21740381056766722, 34.00000000000000711 ) ) ;
#58317 = CARTESIAN_POINT ( 'NONE',  ( 15.11249999999999893, 2.886751345948126879, 4.999999999999999112 ) ) ;
#58318 = EDGE_CURVE ( 'NONE', #57884, #34155, #60660, .T. ) ;
#58319 = CARTESIAN_POINT ( 'NONE',  ( -2.121784821874996840, 10.87812500061451715, 33.67503911421598417 ) ) ;
#58320 = CARTESIAN_POINT ( 'NONE',  ( 13.95000000122903572, -2.886751345948129988, 4.999999999999997335 ) ) ;
#58321 = CARTESIAN_POINT ( 'NONE',  ( 24.94687500061451502, -3.027376345333614438, 5.243569643749998122 ) ) ;
#58322 = ORIENTED_EDGE ( 'NONE', *, *, #71773, .T. ) ;
#58323 = CARTESIAN_POINT ( 'NONE',  ( 20.16562500061451146, 3.027376345333613106, -5.243569643749998122 ) ) ;
#58324 = CARTESIAN_POINT ( 'NONE',  ( 3.778125000614519280, -4.541064518000419881, 2.621784821874995952 ) ) ;
#58325 = CARTESIAN_POINT ( 'NONE',  ( 19.17187500061451999, -6.054752690667223547, -1.112240025338166033E-15 ) ) ;
#58326 = CARTESIAN_POINT ( 'NONE',  ( 3.750000000000000000, 4.330127018922192761, -2.499999999999997780 ) ) ;
#58327 = CARTESIAN_POINT ( 'NONE',  ( 6.515625000614516438, -6.054752690667223547, -1.112240025338166033E-15 ) ) ;
#58328 = CARTESIAN_POINT ( 'NONE',  ( 20.91562500061451502, -6.054752690667223547, -1.112240025338166033E-15 ) ) ;
#58329 = CARTESIAN_POINT ( 'NONE',  ( 9.001249775931846008E-16, 16.31562500061451715, 34.90005215228797653 ) ) ;
#58330 = CARTESIAN_POINT ( 'NONE',  ( 18.86250000122903359, 0.000000000000000000, 4.999999999999998224 ) ) ;
#58331 = CARTESIAN_POINT ( 'NONE',  ( 13.02187500061451786, 2.746126346562645981, -4.756430356249997438 ) ) ;
#58332 = CARTESIAN_POINT ( 'NONE',  ( 9.965625000614517504, 3.027376345333611329, 5.243569643749999010 ) ) ;
#58333 = CARTESIAN_POINT ( 'NONE',  ( 2.859375000614519546, 0.000000000000000000, 5.243569643749999010 ) ) ;
#58334 = CARTESIAN_POINT ( 'NONE',  ( 29.05312500061451431, -4.541064518000417216, -2.621784821875001281 ) ) ;
#58335 = CARTESIAN_POINT ( 'NONE',  ( 21.98437500061451644, 6.421520780324663323E-16, -5.243569643749999010 ) ) ;
#58336 = CARTESIAN_POINT ( 'NONE',  ( 15.17812500061451608, 6.421520780324663323E-16, -5.243569643749999010 ) ) ;
#58337 = CARTESIAN_POINT ( 'NONE',  ( 24.07500000122903216, 2.886751345948129099, -4.999999999999998224 ) ) ;
#58338 =( BOUNDED_CURVE ( )  B_SPLINE_CURVE ( 2, ( #52345, #47531, #24261, #69702, #45089, #39548, #62072, #69347, #30896 ),
 .UNSPECIFIED., .F., .F. ) 
 B_SPLINE_CURVE_WITH_KNOTS ( ( 3, 2, 2, 2, 3 ),
 ( 0.5978260869565217295, 0.6014492753623188470, 0.6086956521739130821, 0.6159420289855072062, 0.6195652173913043237 ),
 .UNSPECIFIED. ) 
 CURVE ( )  GEOMETRIC_REPRESENTATION_ITEM ( )  RATIONAL_B_SPLINE_CURVE ( ( 0.9330127018922194093, 0.9330127018922194093, 1.000000000000000000, 0.8660254037844387076, 1.000000000000000000, 0.8660254037844387076, 1.000000000000000000, 0.9330127018922194093, 0.9330127018922194093 ) ) 
 REPRESENTATION_ITEM ( '' )  );
#58339 = CARTESIAN_POINT ( 'NONE',  ( 24.55312500061451786, -4.541064518000417216, -2.621784821875001281 ) ) ;
#58340 = CARTESIAN_POINT ( 'NONE',  ( 20.14687500061451786, -3.027376345333610441, -5.243569643749999898 ) ) ;
#58341 = CARTESIAN_POINT ( 'NONE',  ( 14.69062500061451537, -3.027376345333610441, -5.243569643749999898 ) ) ;
#58342 = CARTESIAN_POINT ( 'NONE',  ( 4.243569643749999898, 18.24687500061451928, 32.45002607614398471 ) ) ;
#58343 = CARTESIAN_POINT ( 'NONE',  ( 23.01562500061451644, 3.027376345333611329, 5.243569643749999010 ) ) ;
#58344 = LINE ( 'NONE', #6677, #29060 ) ;
#58345 = ORIENTED_EDGE ( 'NONE', *, *, #39744, .F. ) ;
#58346 = CARTESIAN_POINT ( 'NONE',  ( 24.56250000000000000, 2.886751345948126879, 4.999999999999999112 ) ) ;
#58347 = CARTESIAN_POINT ( 'NONE',  ( 3.999999999999999112, 10.77500000000000213, -30.00000000000000000 ) ) ;
#58348 = CARTESIAN_POINT ( 'NONE',  ( 3.756430356250000546, 19.99062499938548143, 27.83122392262697886 ) ) ;
#58349 = CARTESIAN_POINT ( 'NONE',  ( 26.61562500061451786, 3.027376345333611329, 5.243569643749999010 ) ) ;
#58350 = CARTESIAN_POINT ( 'NONE',  ( 6.703125000614516438, 4.541064518000418104, -2.621784821874998173 ) ) ;
#58351 = CARTESIAN_POINT ( 'NONE',  ( 18.82500000122903216, 2.886751345948126879, 4.999999999999999112 ) ) ;
#58352 = CARTESIAN_POINT ( 'NONE',  ( 25.90312500061451573, -4.541064518000417216, -2.621784821875001281 ) ) ;
#58353 = CARTESIAN_POINT ( 'NONE',  ( 25.57499999999999929, -4.330127018922194537, 2.499999999999995559 ) ) ;
#58354 = CARTESIAN_POINT ( 'NONE',  ( 4.000000000000000000, 15.35000000122903252, -27.69059892324149530 ) ) ;
#58355 = CARTESIAN_POINT ( 'NONE',  ( 29.05312500061451431, -4.541064518000417216, -2.621784821875001281 ) ) ;
#58356 = CARTESIAN_POINT ( 'NONE',  ( 10.19062500061451892, -3.027376345333610441, -5.243569643749999898 ) ) ;
#58357 = VERTEX_POINT ( 'NONE', #65658 ) ;
#58358 = CARTESIAN_POINT ( 'NONE',  ( 26.12812500061451360, 4.541064518000418104, 2.621784821874999949 ) ) ;
#58359 = CARTESIAN_POINT ( 'NONE',  ( 7.453125000614516438, -4.541064518000417216, -2.621784821875001281 ) ) ;
#58360 = VECTOR ( 'NONE', #61035, 1000.000000000000000 ) ;
#58361 = CARTESIAN_POINT ( 'NONE',  ( 3.440625000614518036, -3.027376345333610441, -5.243569643749999898 ) ) ;
#58362 = CARTESIAN_POINT ( 'NONE',  ( 17.10937500061451999, 4.119189519843966529, -2.378215178124998275 ) ) ;
#58363 = FACE_OUTER_BOUND ( 'NONE', #68349, .T. ) ;
#58364 = VECTOR ( 'NONE', #37409, 1000.000000000000000 ) ;
#58365 = CARTESIAN_POINT ( 'NONE',  ( 12.48750000000000249, -2.886751345948129988, 4.999999999999997335 ) ) ;
#58367 = CARTESIAN_POINT ( 'NONE',  ( 12.64687500061451608, 6.054752690667223547, 3.707466751127219781E-16 ) ) ;
#58366 = AXIS2_PLACEMENT_3D ( 'NONE', #31991, #47892, #30886 ) ;
#58368 = CARTESIAN_POINT ( 'NONE',  ( 9.825000001229033941, 2.886751345948126879, 4.999999999999999112 ) ) ;
#58369 = CARTESIAN_POINT ( 'NONE',  ( 17.78437500061451715, -4.541064518000419881, 2.621784821874995952 ) ) ;
#58370 = CARTESIAN_POINT ( 'NONE',  ( 18.63749999999999929, 5.773502691896255534, 3.535250795749688894E-16 ) ) ;
#58371 = CARTESIAN_POINT ( 'NONE',  ( 7.396875000614519635, -3.027376345333614438, 5.243569643749998122 ) ) ;
#58372 = CARTESIAN_POINT ( 'NONE',  ( -4.243569643749999898, 11.66562500061451679, -32.45002607614398471 ) ) ;
#58373 = CARTESIAN_POINT ( 'NONE',  ( 23.78437500061451360, 5.492252693125287522, 3.363034840372157021E-16 ) ) ;
#58374 = ORIENTED_EDGE ( 'NONE', *, *, #33319, .T. ) ;
#58375 = CARTESIAN_POINT ( 'NONE',  ( 23.46562500061451573, 3.027376345333611329, 5.243569643749999010 ) ) ;
#58376 = CARTESIAN_POINT ( 'NONE',  ( 26.39999999999999858, 0.000000000000000000, 4.999999999999998224 ) ) ;
#58377 = CARTESIAN_POINT ( 'NONE',  ( 25.84687500061451360, -3.027376345333614438, 5.243569643749998122 ) ) ;
#58378 = CARTESIAN_POINT ( 'NONE',  ( 28.39687500061452141, 6.054752690667223547, 3.707466751127219781E-16 ) ) ;
#58379 = CARTESIAN_POINT ( 'NONE',  ( 21.75000000000000000, 4.330127018922192761, -2.499999999999997780 ) ) ;
#58380 = CARTESIAN_POINT ( 'NONE',  ( 6.853125000614516793, 0.000000000000000000, 5.243569643749999010 ) ) ;
#58381 = CARTESIAN_POINT ( 'NONE',  ( 23.55937500061451573, -5.492252693125287522, -1.008910452111647106E-15 ) ) ;
#58382 = CARTESIAN_POINT ( 'NONE',  ( 16.09687500061452070, -3.027376345333610441, -5.243569643749999898 ) ) ;
#58383 = CARTESIAN_POINT ( 'NONE',  ( 9.646875000614514306, -4.119189519843965641, -2.378215178125001383 ) ) ;
#58384 = CARTESIAN_POINT ( 'NONE',  ( 3.628125000614518036, 4.541064518000418104, 2.621784821874999949 ) ) ;
#58385 = CARTESIAN_POINT ( 'NONE',  ( 7.321875000614516793, 3.027376345333611329, 5.243569643749999010 ) ) ;
#58386 = ORIENTED_EDGE ( 'NONE', *, *, #70897, .F. ) ;
#58387 = CARTESIAN_POINT ( 'NONE',  ( 18.87187500061451573, 3.027376345333613106, -5.243569643749998122 ) ) ;
#58388 = CARTESIAN_POINT ( 'NONE',  ( -3.871985432722222509, 25.03371007018978744, 28.96247042170731589 ) ) ;
#58389 = CARTESIAN_POINT ( 'NONE',  ( 27.33750000000000213, -2.886751345948129988, 4.999999999999997335 ) ) ;
#58390 = CARTESIAN_POINT ( 'NONE',  ( 28.05937500061451573, 0.000000000000000000, 5.243569643749999010 ) ) ;
#58391 = CARTESIAN_POINT ( 'NONE',  ( -2.498395430326213790E-14, 19.30624999877096926, 26.00000000000000000 ) ) ;
#58392 = CARTESIAN_POINT ( 'NONE',  ( 10.20000000000000107, 0.000000000000000000, 4.999999999999998224 ) ) ;
#58393 = EDGE_LOOP ( 'NONE', ( #21856, #15822, #29625, #67210 ) ) ;
#58394 = CARTESIAN_POINT ( 'NONE',  ( 9.862500000000000711, -5.773502691896255534, -1.060575238724906372E-15 ) ) ;
#58395 = CARTESIAN_POINT ( 'NONE',  ( 12.42187500061451466, 5.824947211148865298E-16, -4.756430356249998326 ) ) ;
#58396 = CARTESIAN_POINT ( 'NONE',  ( 21.77812500061451928, -4.541064518000419881, 2.621784821874995952 ) ) ;
#58397 = CARTESIAN_POINT ( 'NONE',  ( 12.52500000000000213, -4.330127018922194537, 2.499999999999995559 ) ) ;
#58398 = CARTESIAN_POINT ( 'NONE',  ( 8.962500001229033231, 0.000000000000000000, 4.999999999999998224 ) ) ;
#58399 = CARTESIAN_POINT ( 'NONE',  ( 7.340625000614518392, -3.027376345333614438, 5.243569643749998122 ) ) ;
#58400 = CARTESIAN_POINT ( 'NONE',  ( 21.67500000000000071, 6.123233995736764310E-16, -4.999999999999998224 ) ) ;
#58401 = EDGE_CURVE ( 'NONE', #27655, #53683, #70167, .T. ) ;
#58402 = CARTESIAN_POINT ( 'NONE',  ( 20.50312500061451715, -4.541064518000417216, -2.621784821875001281 ) ) ;
#58403 = CARTESIAN_POINT ( 'NONE',  ( 14.77500000000000036, -4.330127018922194537, 2.499999999999995559 ) ) ;
#58404 = CARTESIAN_POINT ( 'NONE',  ( 24.45000000122903572, -2.886751345948125991, -5.000000000000000000 ) ) ;
#58405 = CARTESIAN_POINT ( 'NONE',  ( -1.878215178124999163, 18.64062499938548356, 26.74683588394047007 ) ) ;
#58406 = CARTESIAN_POINT ( 'NONE',  ( 4.312500000000000000, 2.886751345948126879, 4.999999999999999112 ) ) ;
#58407 = ORIENTED_EDGE ( 'NONE', *, *, #32675, .T. ) ;
#58408 = CARTESIAN_POINT ( 'NONE',  ( 20.69062500061451715, 6.054752690667223547, 3.707466751127219781E-16 ) ) ;
#58409 = CARTESIAN_POINT ( 'NONE',  ( 26.05312500061451431, 4.541064518000418104, -2.621784821874998173 ) ) ;
#58410 = CARTESIAN_POINT ( 'NONE',  ( 26.63437500061451857, 4.541064518000418104, 2.621784821874999949 ) ) ;
#58411 = CARTESIAN_POINT ( 'NONE',  ( 14.12812500061451715, -4.541064518000419881, 2.621784821874995952 ) ) ;
#58412 = CARTESIAN_POINT ( 'NONE',  ( 29.69062500061451715, 6.054752690667223547, 3.707466751127219781E-16 ) ) ;
#58413 = CARTESIAN_POINT ( 'NONE',  ( 8.953125000614518214, 4.541064518000418104, -2.621784821874998173 ) ) ;
#58414 = CARTESIAN_POINT ( 'NONE',  ( -2.121784821874999949, 9.828125000614592821, -33.67503911421598417 ) ) ;
#58415 = CARTESIAN_POINT ( 'NONE',  ( 26.10000000122903430, -2.886751345948129988, 4.999999999999997335 ) ) ;
#58416 = CARTESIAN_POINT ( 'NONE',  ( 18.45937500061451431, 4.119189519843966529, -2.378215178124998275 ) ) ;
#58417 = CARTESIAN_POINT ( 'NONE',  ( 17.42812500061451786, 6.421520780324663323E-16, -5.243569643749999010 ) ) ;
#58418 = CARTESIAN_POINT ( 'NONE',  ( 28.66875000122903216, 2.886751345948161962, 4.999999999999938716 ) ) ;
#58419 = CARTESIAN_POINT ( 'NONE',  ( 29.85937500061451644, 0.000000000000000000, 5.243569643749999010 ) ) ;
#58420 = CARTESIAN_POINT ( 'NONE',  ( 9.609375000614518214, 0.000000000000000000, 5.243569643749999010 ) ) ;
#58421 = CARTESIAN_POINT ( 'NONE',  ( 9.196875000614518569, -3.027376345333614438, 5.243569643749998122 ) ) ;
#58422 = CARTESIAN_POINT ( 'NONE',  ( 17.93437500061451928, 6.421520780324663323E-16, -5.243569643749999010 ) ) ;
#58423 = ORIENTED_EDGE ( 'NONE', *, *, #66261, .T. ) ;
#58424 = CARTESIAN_POINT ( 'NONE',  ( 24.15000000122903145, 5.773502691896255534, 3.535250795749688401E-16 ) ) ;
#58425 = CARTESIAN_POINT ( 'NONE',  ( 22.56562500061451715, 3.027376345333611329, 5.243569643749999010 ) ) ;
#58426 = VECTOR ( 'NONE', #60447, 1000.000000000000000 ) ;
#58427 = CARTESIAN_POINT ( 'NONE',  ( 16.58437500061451786, 6.421520780324663323E-16, -5.243569643749999010 ) ) ;
#58428 = CARTESIAN_POINT ( 'NONE',  ( 21.81562500061451004, -6.054752690667223547, -1.112240025338166033E-15 ) ) ;
#58429 = CARTESIAN_POINT ( 'NONE',  ( -2.000000000000000000, 14.07500000000000107, 26.53589838486224650 ) ) ;
#58430 = CARTESIAN_POINT ( 'NONE',  ( 28.64062500061451289, -3.027376345333610441, -5.243569643749999898 ) ) ;
#58431 = CARTESIAN_POINT ( 'NONE',  ( 10.16250000122903252, 4.330127018922192761, -2.499999999999997780 ) ) ;
#58432 = VECTOR ( 'NONE', #53249, 1000.000000000000000 ) ;
#58433 = VERTEX_POINT ( 'NONE', #38314 ) ;
#58434 = CARTESIAN_POINT ( 'NONE',  ( 4.012500001229033053, 0.000000000000000000, 4.999999999999998224 ) ) ;
#58435 = CARTESIAN_POINT ( 'NONE',  ( -2.000000000000000000, 18.57500000000000284, -33.46410161513775705 ) ) ;
#58436 = CARTESIAN_POINT ( 'NONE',  ( 25.35000000122903074, -2.886751345948125991, -5.000000000000000000 ) ) ;
#58437 = CARTESIAN_POINT ( 'NONE',  ( 1.999999999999997335, 20.46874999877096712, 33.46410161513775705 ) ) ;
#58438 = CARTESIAN_POINT ( 'NONE',  ( 9.121875000614517504, 3.027376345333611329, 5.243569643749999010 ) ) ;
#58439 = CARTESIAN_POINT ( 'NONE',  ( 24.60000000000000142, 0.000000000000000000, 4.999999999999998224 ) ) ;
#58440 = CARTESIAN_POINT ( 'NONE',  ( 14.20312500061451644, -4.541064518000417216, -2.621784821875001281 ) ) ;
#58441 = CARTESIAN_POINT ( 'NONE',  ( 10.77187500061451786, 3.027376345333613106, -5.243569643749998122 ) ) ;
#58442 = CARTESIAN_POINT ( 'NONE',  ( 3.065625000614517592, 3.027376345333613106, -5.243569643749998122 ) ) ;
#58443 = CARTESIAN_POINT ( 'NONE',  ( 16.73437500061451644, 4.541064518000418104, 2.621784821874999949 ) ) ;
#58444 = CARTESIAN_POINT ( 'NONE',  ( 8.521875000614516082, 3.027376345333613106, -5.243569643749998122 ) ) ;
#58445 = CARTESIAN_POINT ( 'NONE',  ( 1.071796769724493892, 17.61740381056766580, -34.00000000000000000 ) ) ;
#58446 = CARTESIAN_POINT ( 'NONE',  ( 8.428125000614517859, 6.421520780324663323E-16, -5.243569643749999010 ) ) ;
#58447 = CARTESIAN_POINT ( 'NONE',  ( 18.14062500061451644, -3.027376345333614438, 5.243569643749998122 ) ) ;
#58448 = ORIENTED_EDGE ( 'NONE', *, *, #71031, .F. ) ;
#58449 = CARTESIAN_POINT ( 'NONE',  ( 15.10312500061451502, -4.541064518000417216, -2.621784821875001281 ) ) ;
#58450 = CARTESIAN_POINT ( 'NONE',  ( 11.16562500061451679, 3.027376345333613106, -5.243569643749998122 ) ) ;
#58451 = CARTESIAN_POINT ( 'NONE',  ( 23.29687500061451644, -2.746126346562642428, -4.756430356249999214 ) ) ;
#58452 = CARTESIAN_POINT ( 'NONE',  ( 11.21250000000000036, -5.773502691896255534, -1.060575238724906372E-15 ) ) ;
#58453 = CARTESIAN_POINT ( 'NONE',  ( 6.712500001229034119, 0.000000000000000000, 4.999999999999998224 ) ) ;
#58454 = EDGE_CURVE ( 'NONE', #44755, #8380, #26881, .T. ) ;
#58455 = CARTESIAN_POINT ( 'NONE',  ( 14.29687500061451821, -3.027376345333610441, -5.243569643749999898 ) ) ;
#58456 = CARTESIAN_POINT ( 'NONE',  ( 16.57500000122903216, 2.886751345948126879, 4.999999999999999112 ) ) ;
#58457 = CARTESIAN_POINT ( 'NONE',  ( 24.97499999999999787, 4.330127018922191873, 2.499999999999999556 ) ) ;
#58458 = VECTOR ( 'NONE', #15747, 1000.000000000000000 ) ;
#58459 = CARTESIAN_POINT ( 'NONE',  ( -4.243569643749999898, 18.90312500061451573, -30.00000000000000000 ) ) ;
#58460 = CARTESIAN_POINT ( 'NONE',  ( 16.23750000122903359, -4.330127018922194537, 2.499999999999995559 ) ) ;
#58461 = DIRECTION ( 'NONE',  ( 0.000000000000000000, 0.000000000000000000, 1.000000000000000000 ) ) ;
#58462 = CARTESIAN_POINT ( 'NONE',  ( 4.898734551532200499, 1.001199177798645534, 4.898734551532190729 ) ) ;
#58463 = CARTESIAN_POINT ( 'NONE',  ( 30.00000000000000000, 0.000000000000000000, 0.000000000000000000 ) ) ;
#58464 = CARTESIAN_POINT ( 'NONE',  ( 18.90937500061451360, 4.541064518000418104, -2.621784821874998173 ) ) ;
#58465 = CARTESIAN_POINT ( 'NONE',  ( 28.57499999999999929, 4.330127018922191873, 2.499999999999999556 ) ) ;
#58466 = CARTESIAN_POINT ( 'NONE',  ( 13.11562500061451786, 3.027376345333611329, 5.243569643749999010 ) ) ;
#58467 = CARTESIAN_POINT ( 'NONE',  ( 9.281250001229032875, 4.330127018922191873, 2.499999999999999556 ) ) ;
#58468 = CARTESIAN_POINT ( 'NONE',  ( 23.37187500061451573, 3.027376345333613106, -5.243569643749998122 ) ) ;
#58469 = CARTESIAN_POINT ( 'NONE',  ( 16.20937500061451431, 2.746126346562643317, 4.756430356249998326 ) ) ;
#58470 = CARTESIAN_POINT ( 'NONE',  ( 9.103125000614515017, 0.000000000000000000, 5.243569643749999010 ) ) ;
#58471 = AXIS2_PLACEMENT_3D ( 'NONE', #38809, #32163, #15888 ) ;
#58472 = CARTESIAN_POINT ( 'NONE',  ( 16.65937500061452070, 4.541064518000418104, -2.621784821874998173 ) ) ;
#58473 = ORIENTED_EDGE ( 'NONE', *, *, #38317, .T. ) ;
#58474 = CARTESIAN_POINT ( 'NONE',  ( 27.12187500061451573, 3.027376345333611329, 5.243569643749999010 ) ) ;
#58475 = CARTESIAN_POINT ( 'NONE',  ( 26.54062500061451146, 6.054752690667223547, 3.707466751127219781E-16 ) ) ;
#58476 = CARTESIAN_POINT ( 'NONE',  ( 18.81562500061452070, 3.027376345333613106, -5.243569643749998122 ) ) ;
#58477 = CARTESIAN_POINT ( 'NONE',  ( 3.095752589150487122, 3.926369699671143909, -3.475442218917008663 ) ) ;
#58478 = EDGE_CURVE ( 'NONE', #44169, #46196, #47505, .T. ) ;
#58479 = CARTESIAN_POINT ( 'NONE',  ( 4.897546610576117843, 1.006994139586731674, -5.145967878999484491 ) ) ;
#58480 = CARTESIAN_POINT ( 'NONE',  ( 9.750000000000001776, 0.000000000000000000, 4.999999999999998224 ) ) ;
#58481 = CARTESIAN_POINT ( 'NONE',  ( 19.57500000122903216, 2.886751345948129099, -4.999999999999998224 ) ) ;
#58482 = CARTESIAN_POINT ( 'NONE',  ( 29.32499999999999929, 6.123233995736764310E-16, -4.999999999999998224 ) ) ;
#58483 = CARTESIAN_POINT ( 'NONE',  ( 10.62187500061451395, 5.824947211148865298E-16, -4.756430356249998326 ) ) ;
#58484 = ORIENTED_EDGE ( 'NONE', *, *, #69660, .T. ) ;
#58485 = CARTESIAN_POINT ( 'NONE',  ( 17.06250000000000000, -5.773502691896255534, -1.060575238724906372E-15 ) ) ;
#58486 =( BOUNDED_CURVE ( )  B_SPLINE_CURVE ( 2, ( #27748, #50287, #72811, #36460, #48283, #24278, #58975, #13186, #3217 ),
 .UNSPECIFIED., .F., .F. ) 
 B_SPLINE_CURVE_WITH_KNOTS ( ( 3, 2, 2, 2, 3 ),
 ( 0.7065217391304348116, 0.7101449275362319291, 0.7173913043478260532, 0.7246376811594202882, 0.7282608695652174058 ),
 .UNSPECIFIED. ) 
 CURVE ( )  GEOMETRIC_REPRESENTATION_ITEM ( )  RATIONAL_B_SPLINE_CURVE ( ( 0.9330127018922194093, 0.9330127018922194093, 1.000000000000000000, 0.8660254037844387076, 1.000000000000000000, 0.8660254037844387076, 1.000000000000000000, 0.9330127018922194093, 0.9330127018922194093 ) ) 
 REPRESENTATION_ITEM ( '' )  );
#58487 = CARTESIAN_POINT ( 'NONE',  ( 21.82499999999999574, 4.330127018922191873, 2.499999999999999556 ) ) ;
#58488 = CARTESIAN_POINT ( 'NONE',  ( 19.77187500061451786, 3.027376345333613106, -5.243569643749998122 ) ) ;
#58489 = CARTESIAN_POINT ( 'NONE',  ( 12.77812500061451750, -4.541064518000419881, 2.621784821874995952 ) ) ;
#58490 = ORIENTED_EDGE ( 'NONE', *, *, #21207, .T. ) ;
#58491 = CARTESIAN_POINT ( 'NONE',  ( 4.715625000614516615, -6.054752690667223547, -1.112240025338166033E-15 ) ) ;
#58492 = CYLINDRICAL_SURFACE ( 'NONE', #20572, 4.999999999999998224 ) ;
#58493 = CARTESIAN_POINT ( 'NONE',  ( 12.97499999999999964, -4.330127018922194537, 2.499999999999995559 ) ) ;
#58494 = CARTESIAN_POINT ( 'NONE',  ( 28.95937500061451075, -5.492252693125287522, -1.008910452111647106E-15 ) ) ;
#58495 = CARTESIAN_POINT ( 'NONE',  ( -4.243569643749999898, 16.16562500061451857, 27.54997392385601529 ) ) ;
#58496 = CARTESIAN_POINT ( 'NONE',  ( 28.71562500061451573, 3.027376345333613106, -5.243569643749998122 ) ) ;
#58497 = CARTESIAN_POINT ( 'NONE',  ( 9.150000000000002132, 4.330127018922192761, -2.499999999999997780 ) ) ;
#58498 = CARTESIAN_POINT ( 'NONE',  ( 1.878215178125000495, 17.66562499938548214, 26.74683588394047007 ) ) ;
#58499 = CARTESIAN_POINT ( 'NONE',  ( 23.22187500061451715, -6.054752690667223547, -1.112240025338166033E-15 ) ) ;
#58500 = ORIENTED_EDGE ( 'NONE', *, *, #57737, .F. ) ;
#58501 = CARTESIAN_POINT ( 'NONE',  ( 21.25312500061451715, 0.000000000000000000, 5.243569643749999010 ) ) ;
#58502 = CARTESIAN_POINT ( 'NONE',  ( 22.65937500061451715, 0.000000000000000000, 5.243569643749999010 ) ) ;
#58503 = CARTESIAN_POINT ( 'NONE',  ( -4.243569643749999898, 16.61562500061459602, -32.45002607614398471 ) ) ;
#58504 = CARTESIAN_POINT ( 'NONE',  ( 7.078125000614516438, 6.421520780324663323E-16, -5.243569643749999010 ) ) ;
#58505 = CARTESIAN_POINT ( 'NONE',  ( 26.37187500061451573, -5.492252693125287522, -1.008910452111647106E-15 ) ) ;
#58506 = CARTESIAN_POINT ( 'NONE',  ( 23.80312500061451786, 4.541064518000418104, -2.621784821874998173 ) ) ;
#58507 = CARTESIAN_POINT ( 'NONE',  ( 11.22187500061451892, 2.746126346562645981, -4.756430356249997438 ) ) ;
#58508 = CARTESIAN_POINT ( 'NONE',  ( 17.22187500061451715, 3.027376345333611329, 5.243569643749999010 ) ) ;
#58509 = CARTESIAN_POINT ( 'NONE',  ( 24.75937500061451502, 4.541064518000418104, -2.621784821874998173 ) ) ;
#58510 = CARTESIAN_POINT ( 'NONE',  ( 4.243569643749999898, 15.13437500061451679, 30.00000000000000000 ) ) ;
#58511 = CARTESIAN_POINT ( 'NONE',  ( 6.778125000614518392, 4.541064518000418104, 2.621784821874999949 ) ) ;
#58512 = CARTESIAN_POINT ( 'NONE',  ( -1.999999999999997113, 18.27499999999999858, -26.53589838486224295 ) ) ;
#58513 = CARTESIAN_POINT ( 'NONE',  ( 3.046875000614519990, -3.027376345333610441, -5.243569643749999898 ) ) ;
#58514 = CARTESIAN_POINT ( 'NONE',  ( -1.999999999999999112, 13.55000000000000071, 26.53589838486224650 ) ) ;
#58515 = AXIS2_PLACEMENT_3D ( 'NONE', #45955, #18209, #29326 ) ;
#58516 = CARTESIAN_POINT ( 'NONE',  ( 5.428125000614517859, 4.541064518000418104, 2.621784821874999949 ) ) ;
#58517 = CARTESIAN_POINT ( 'NONE',  ( 10.35937500061451644, 4.541064518000418104, -2.621784821874998173 ) ) ;
#58518 = CARTESIAN_POINT ( 'NONE',  ( 17.85000000122903430, 5.773502691896255534, 3.535250795749688894E-16 ) ) ;
#58519 = CARTESIAN_POINT ( 'NONE',  ( 29.24062500061451431, 6.054752690667223547, 3.707466751127219781E-16 ) ) ;
#58520 = CARTESIAN_POINT ( 'NONE',  ( 6.928125000614516082, -4.541064518000419881, 2.621784821874995952 ) ) ;
#58521 = CARTESIAN_POINT ( 'NONE',  ( 1.999999999999997335, 14.16874999877096641, 33.46410161513775705 ) ) ;
#58522 = CARTESIAN_POINT ( 'NONE',  ( 20.60625000122902861, 0.000000000000000000, 4.999999999999998224 ) ) ;
#58523 = CARTESIAN_POINT ( 'NONE',  ( 17.37187500061451573, -6.054752690667223547, -1.112240025338166033E-15 ) ) ;
#58524 = CARTESIAN_POINT ( 'NONE',  ( 4.000000000000000000, 19.23124999877096641, 27.69059892324149885 ) ) ;
#58525 = ORIENTED_EDGE ( 'NONE', *, *, #15234, .T. ) ;
#58526 = CARTESIAN_POINT ( 'NONE',  ( 22.52812500061451573, 4.541064518000418104, 2.621784821874999949 ) ) ;
#58527 = CARTESIAN_POINT ( 'NONE',  ( 10.15312500061451750, -4.541064518000417216, -2.621784821875001281 ) ) ;
#58528 = CARTESIAN_POINT ( 'NONE',  ( 27.53437500061451360, 4.541064518000418104, 2.621784821874999949 ) ) ;
#58529 = CARTESIAN_POINT ( 'NONE',  ( 11.05312500061451608, -4.541064518000417216, -2.621784821875001281 ) ) ;
#58530 = DIRECTION ( 'NONE',  ( 0.000000000000000000, 0.000000000000000000, 1.000000000000000000 ) ) ;
#58531 = CARTESIAN_POINT ( 'NONE',  ( 9.525000001229033231, -5.773502691896255534, -1.060575238724906372E-15 ) ) ;
#58532 = CARTESIAN_POINT ( 'NONE',  ( 25.97812500061451502, 6.421520780324663323E-16, -5.243569643749999010 ) ) ;
#58533 = CARTESIAN_POINT ( 'NONE',  ( 4.243569643749999898, 11.44062500061451715, -27.54997392385601529 ) ) ;
#58534 = CARTESIAN_POINT ( 'NONE',  ( 12.97500000122903252, 2.886751345948126879, 4.999999999999999112 ) ) ;
#58535 = CARTESIAN_POINT ( 'NONE',  ( 22.15312500061451573, 0.000000000000000000, 5.243569643749999010 ) ) ;
#58536 = CARTESIAN_POINT ( 'NONE',  ( 17.61562500061451786, 3.027376345333611329, 5.243569643749999010 ) ) ;
#58537 = CARTESIAN_POINT ( 'NONE',  ( 1.626862140677534273E-15, 18.76250000000000284, -26.00000000000000355 ) ) ;
#58538 = CARTESIAN_POINT ( 'NONE',  ( 17.88749999999999929, -2.886751345948129988, 4.999999999999997335 ) ) ;
#58539 = CARTESIAN_POINT ( 'NONE',  ( 12.93750000122903465, 4.330127018922191873, 2.499999999999999556 ) ) ;
#58540 =( BOUNDED_CURVE ( )  B_SPLINE_CURVE ( 2, ( #61890, #71895, #43822, #10197, #11295, #55269, #21633, #27194, #55629 ),
 .UNSPECIFIED., .F., .F. ) 
 B_SPLINE_CURVE_WITH_KNOTS ( ( 3, 2, 2, 2, 3 ),
 ( 0.05434782608695652717, 0.05797101449275362389, 0.06521739130434782428, 0.07246376811594203160, 0.07608695652173913526 ),
 .UNSPECIFIED. ) 
 CURVE ( )  GEOMETRIC_REPRESENTATION_ITEM ( )  RATIONAL_B_SPLINE_CURVE ( ( 0.9330127018922194093, 0.9330127018922194093, 1.000000000000000000, 0.8660254037844387076, 1.000000000000000000, 0.8660254037844387076, 1.000000000000000000, 0.9330127018922191873, 0.9330127018922192983 ) ) 
 REPRESENTATION_ITEM ( '' )  );
#58541 = CARTESIAN_POINT ( 'NONE',  ( 9.628125000614517148, -4.541064518000419881, 2.621784821874995952 ) ) ;
#58542 = CARTESIAN_POINT ( 'NONE',  ( 13.64062500061451644, -3.027376345333614438, 5.243569643749998122 ) ) ;
#58543 = EDGE_CURVE ( 'NONE', #20630, #59956, #4607, .T. ) ;
#58544 = CARTESIAN_POINT ( 'NONE',  ( 23.28750000122903430, 4.330127018922191873, 2.499999999999999556 ) ) ;
#58545 = CARTESIAN_POINT ( 'NONE',  ( 20.93437500061451573, -4.541064518000419881, 2.621784821874995952 ) ) ;
#58546 = CARTESIAN_POINT ( 'NONE',  ( 21.60937500061451644, 4.541064518000418104, -2.621784821874998173 ) ) ;
#58547 = CYLINDRICAL_SURFACE ( 'NONE', #13478, 4.999999999999998224 ) ;
#58548 = AXIS2_PLACEMENT_3D ( 'NONE', #27595, #21907, #72518 ) ;
#58549 = ADVANCED_FACE ( 'NONE', ( #26510 ), #20214, .T. ) ;
#58550 = CARTESIAN_POINT ( 'NONE',  ( 7.725000001229034297, -5.773502691896255534, -1.060575238724906372E-15 ) ) ;
#58551 = CARTESIAN_POINT ( 'NONE',  ( 7.134375000614516793, 6.421520780324663323E-16, -5.243569643749999010 ) ) ;
#58552 = CARTESIAN_POINT ( 'NONE',  ( 26.33437500061451431, -4.541064518000419881, 2.621784821874995952 ) ) ;
#58553 = EDGE_CURVE ( 'NONE', #20715, #17509, #37588, .T. ) ;
#58554 =( BOUNDED_CURVE ( )  B_SPLINE_CURVE ( 2, ( #15441, #66809, #9551, #38732, #3653, #26176, #48717, #71239, #43177 ),
 .UNSPECIFIED., .F., .F. ) 
 B_SPLINE_CURVE_WITH_KNOTS ( ( 3, 2, 2, 2, 3 ),
 ( 0.9456521739130434590, 0.9492753623188405765, 0.9565217391304348116, 0.9637681159420289356, 0.9662083003288912675 ),
 .UNSPECIFIED. ) 
 CURVE ( )  GEOMETRIC_REPRESENTATION_ITEM ( )  RATIONAL_B_SPLINE_CURVE ( ( 0.9330127018922194093, 0.9330127018922194093, 1.000000000000000000, 0.8660254037844387076, 1.000000000000000000, 0.8660254037844387076, 1.000000000000000000, 0.9548846649268474263, 0.9401540970596797830 ) ) 
 REPRESENTATION_ITEM ( '' )  );
#58555 = CARTESIAN_POINT ( 'NONE',  ( 2.859375000614519546, 0.000000000000000000, 5.243569643749999010 ) ) ;
#58556 = CARTESIAN_POINT ( 'NONE',  ( 21.40312500061451573, -4.541064518000417216, -2.621784821875001281 ) ) ;
#58557 = CARTESIAN_POINT ( 'NONE',  ( 26.10937500061451644, 4.541064518000418104, -2.621784821874998173 ) ) ;
#58558 = CARTESIAN_POINT ( 'NONE',  ( 3.756430356250000546, 16.84062499938548285, 27.83122392262697886 ) ) ;
#58559 = CARTESIAN_POINT ( 'NONE',  ( 19.25625000122903430, 0.000000000000000000, 4.999999999999998224 ) ) ;
#58560 = AXIS2_PLACEMENT_3D ( 'NONE', #16319, #45136, #5613 ) ;
#58561 = CARTESIAN_POINT ( 'NONE',  ( -3.999999999999999112, 13.32500000122903216, -32.30940107675850470 ) ) ;
#58562 = CARTESIAN_POINT ( 'NONE',  ( 4.359375000614517326, -4.541064518000417216, -2.621784821875001281 ) ) ;
#58563 = CARTESIAN_POINT ( 'NONE',  ( 17.24062500061451786, -3.027376345333614438, 5.243569643749998122 ) ) ;
#58564 = VERTEX_POINT ( 'NONE', #48679 ) ;
#58565 = LINE ( 'NONE', #64848, #48967 ) ;
#58566 = CARTESIAN_POINT ( 'NONE',  ( 26.31562500061451715, -6.054752690667223547, -1.112240025338166033E-15 ) ) ;
#58567 = CARTESIAN_POINT ( 'NONE',  ( 4.659375000614518925, 0.000000000000000000, 5.243569643749999010 ) ) ;
#58568 = CARTESIAN_POINT ( 'NONE',  ( 7.320879633048903241E-15, 17.63749999999999574, -34.00000000000000000 ) ) ;
#58569 = DIRECTION ( 'NONE',  ( -0.000000000000000000, -1.000000000000000000, -0.000000000000000000 ) ) ;
#58570 = CARTESIAN_POINT ( 'NONE',  ( 17.13749999999999929, -2.886751345948125991, -5.000000000000000000 ) ) ;
#58571 = CARTESIAN_POINT ( 'NONE',  ( 21.21562500061451573, 3.027376345333611329, 5.243569643749999010 ) ) ;
#58572 = ORIENTED_EDGE ( 'NONE', *, *, #4888, .F. ) ;
#58573 = CARTESIAN_POINT ( 'NONE',  ( 23.81250000000000000, -5.773502691896255534, -1.060575238724906372E-15 ) ) ;
#58574 = CARTESIAN_POINT ( 'NONE',  ( 25.20937500061451431, 4.541064518000418104, -2.621784821874998173 ) ) ;
#58575 = EDGE_LOOP ( 'NONE', ( #33390, #49623, #29350, #22431 ) ) ;
#58576 = CARTESIAN_POINT ( 'NONE',  ( 13.46250000122903323, 0.000000000000000000, 4.999999999999998224 ) ) ;
#58577 = CARTESIAN_POINT ( 'NONE',  ( 13.00312500061451537, 4.541064518000418104, -2.621784821874998173 ) ) ;
#58578 = CARTESIAN_POINT ( 'NONE',  ( 6.215625000614517504, 3.027376345333613106, -5.243569643749998122 ) ) ;
#58579 = CARTESIAN_POINT ( 'NONE',  ( 16.62187500061451573, 4.119189519843966529, 2.378215178124999607 ) ) ;
#58580 = CARTESIAN_POINT ( 'NONE',  ( 28.82812500061451644, 4.541064518000418104, 2.621784821874999949 ) ) ;
#58581 =( BOUNDED_CURVE ( )  B_SPLINE_CURVE ( 2, ( #11590, #61100, #10498, #153, #67742, #44853, #72919, #23019, #27129 ),
 .UNSPECIFIED., .F., .F. ) 
 B_SPLINE_CURVE_WITH_KNOTS ( ( 3, 2, 2, 2, 3 ),
 ( 0.5694444444444444198, 0.5740740740740740700, 0.5833333333333333703, 0.5925925925925925597, 0.5972222222222222099 ),
 .UNSPECIFIED. ) 
 CURVE ( )  GEOMETRIC_REPRESENTATION_ITEM ( )  RATIONAL_B_SPLINE_CURVE ( ( 0.9330127018922194093, 0.9330127018922194093, 1.000000000000000000, 0.8660254037844387076, 1.000000000000000000, 0.8660254037844387076, 1.000000000000000000, 0.9330127018922194093, 0.9330127018922194093 ) ) 
 REPRESENTATION_ITEM ( '' )  );
#58582 = CARTESIAN_POINT ( 'NONE',  ( 14.77500000122903501, 2.886751345948126879, 4.999999999999999112 ) ) ;
#58583 = CARTESIAN_POINT ( 'NONE',  ( 19.42499999999999716, 6.123233995736764310E-16, -4.999999999999998224 ) ) ;
#58584 = CARTESIAN_POINT ( 'NONE',  ( 26.32499999999999929, 4.330127018922191873, 2.499999999999999556 ) ) ;
#58585 = CARTESIAN_POINT ( 'NONE',  ( 2.934375000614518392, -4.541064518000419881, 2.621784821874995952 ) ) ;
#58586 = CARTESIAN_POINT ( 'NONE',  ( 8.484375000614518214, 6.421520780324663323E-16, -5.243569643749999010 ) ) ;
#58587 = CARTESIAN_POINT ( 'NONE',  ( 19.62187500061451573, -6.054752690667223547, -1.112240025338166033E-15 ) ) ;
#58588 = CARTESIAN_POINT ( 'NONE',  ( 1.626862140677534273E-15, 13.92500000122903181, 34.00000000000000000 ) ) ;
#58589 = ORIENTED_EDGE ( 'NONE', *, *, #15386, .F. ) ;
#58590 = CARTESIAN_POINT ( 'NONE',  ( 29.50312500061451360, -4.541064518000417216, -2.621784821875001281 ) ) ;
#58591 = CARTESIAN_POINT ( 'NONE',  ( 3.600000000000002309, -4.330127018922190985, -2.500000000000001332 ) ) ;
#58593 = ADVANCED_FACE ( 'NONE', ( #36853 ), #54949, .F. ) ;
#58592 = CARTESIAN_POINT ( 'NONE',  ( 5.146875000614517859, -3.027376345333614438, 5.243569643749998122 ) ) ;
#58594 = CARTESIAN_POINT ( 'NONE',  ( 17.21249999999999858, 2.886751345948129099, -4.999999999999998224 ) ) ;
#58595 = CARTESIAN_POINT ( 'NONE',  ( 14.57812500061451644, -4.541064518000419881, 2.621784821874995952 ) ) ;
#58596 = PLANE ( 'NONE',  #20632 ) ;
#58597 = CARTESIAN_POINT ( 'NONE',  ( 17.96250000122903501, 0.000000000000000000, 4.999999999999998224 ) ) ;
#58598 = CARTESIAN_POINT ( 'NONE',  ( 19.27500000122903145, 2.886751345948126879, 4.999999999999999112 ) ) ;
#58599 = CARTESIAN_POINT ( 'NONE',  ( -2.498395430326213790E-14, 19.30624999877096926, 26.00000000000000000 ) ) ;
#58600 = CARTESIAN_POINT ( 'NONE',  ( 16.73437500061451644, 4.119189519843966529, 2.378215178124999607 ) ) ;
#58601 = CARTESIAN_POINT ( 'NONE',  ( 8.615625000614517859, 3.027376345333611329, 5.243569643749999010 ) ) ;
#58602 = CARTESIAN_POINT ( 'NONE',  ( 23.67187500061451999, -6.054752690667223547, -1.112240025338166033E-15 ) ) ;
#58603 = CARTESIAN_POINT ( 'NONE',  ( -4.243569643749999898, 18.95937500061451431, 30.00000000000000000 ) ) ;
#58604 = CARTESIAN_POINT ( 'NONE',  ( 24.57187500061451502, -6.054752690667223547, -1.112240025338166033E-15 ) ) ;
#58605 = CARTESIAN_POINT ( 'NONE',  ( 7.050000000000000711, 0.000000000000000000, 4.999999999999998224 ) ) ;
#58606 = CARTESIAN_POINT ( 'NONE',  ( 1.999999999999998668, 13.66250000122903607, 26.53589838486224650 ) ) ;
#58607 = CARTESIAN_POINT ( 'NONE',  ( 13.71562500061451750, -6.054752690667223547, -1.112240025338166033E-15 ) ) ;
#58608 = CARTESIAN_POINT ( 'NONE',  ( 6.487500001229034474, 6.123233995736764310E-16, -4.999999999999998224 ) ) ;
#58609 = CARTESIAN_POINT ( 'NONE',  ( 10.80937500061451928, 4.541064518000418104, -2.621784821874998173 ) ) ;
#58610 = FACE_OUTER_BOUND ( 'NONE', #15536, .T. ) ;
#58611 = ORIENTED_EDGE ( 'NONE', *, *, #28491, .T. ) ;
#58612 = CARTESIAN_POINT ( 'NONE',  ( 12.55312500061451786, 4.541064518000418104, -2.621784821874998173 ) ) ;
#58613 = CARTESIAN_POINT ( 'NONE',  ( 3.428129095426660555, -3.639779116804093828, -3.774531229163594848 ) ) ;
#58614 = CARTESIAN_POINT ( 'NONE',  ( 23.06250000122903288, -4.330127018922190985, -2.500000000000001332 ) ) ;
#58615 = CARTESIAN_POINT ( 'NONE',  ( 10.58437500061451964, -4.541064518000419881, 2.621784821874995952 ) ) ;
#58616 = CARTESIAN_POINT ( 'NONE',  ( 14.12812500061451715, -4.541064518000419881, 2.621784821874995952 ) ) ;
#58617 = CARTESIAN_POINT ( 'NONE',  ( 28.59375000122903288, 5.773502691896255534, 3.535250795749688894E-16 ) ) ;
#58618 = CARTESIAN_POINT ( 'NONE',  ( 24.15937500061451715, -4.541064518000417216, -2.621784821875001281 ) ) ;
#58619 = CARTESIAN_POINT ( 'NONE',  ( 4.000000000000000000, 15.80000000122903181, 32.30940107675849760 ) ) ;
#58620 = AXIS2_PLACEMENT_3D ( 'NONE', #69037, #58286, #7692 ) ;
#58621 = CARTESIAN_POINT ( 'NONE',  ( 0.000000000000000000, 20.00000000000000000, 26.00000000000000000 ) ) ;
#58622 = CARTESIAN_POINT ( 'NONE',  ( 14.69999999999999929, 0.000000000000000000, 4.999999999999998224 ) ) ;
#58623 = CARTESIAN_POINT ( 'NONE',  ( -4.243569643749999898, 14.87187500061451928, -32.45002607614398471 ) ) ;
#58624 = CARTESIAN_POINT ( 'NONE',  ( 14.63437500061451679, -4.541064518000419881, 2.621784821874995952 ) ) ;
#58625 = CARTESIAN_POINT ( 'NONE',  ( 18.45000000122903216, -2.886751345948129988, 4.999999999999997335 ) ) ;
#58626 = CARTESIAN_POINT ( 'NONE',  ( 12.94687500061451857, -3.027376345333610441, -5.243569643749999898 ) ) ;
#58627 = CARTESIAN_POINT ( 'NONE',  ( -4.243569643749999898, 10.40937500061451892, 30.00000000000000000 ) ) ;
#58628 = CARTESIAN_POINT ( 'NONE',  ( 18.86250000122903359, 0.000000000000000000, 4.999999999999998224 ) ) ;
#58629 = CARTESIAN_POINT ( 'NONE',  ( 12.14062500061451821, 6.054752690667223547, 3.707466751127219781E-16 ) ) ;
#58630 = VERTEX_POINT ( 'NONE', #59742 ) ;
#58631 = ORIENTED_EDGE ( 'NONE', *, *, #63906, .T. ) ;
#58632 = CARTESIAN_POINT ( 'NONE',  ( 18.03749999999999787, -2.886751345948125991, -5.000000000000000000 ) ) ;
#58633 = CARTESIAN_POINT ( 'NONE',  ( 4.000000000000000000, 18.33124999877096784, 27.69059892324149885 ) ) ;
#58634 = CARTESIAN_POINT ( 'NONE',  ( 11.52187500061451608, -6.054752690667223547, -1.112240025338166033E-15 ) ) ;
#58635 = CYLINDRICAL_SURFACE ( 'NONE', #52723, 4.999999999999998224 ) ;
#58636 = CARTESIAN_POINT ( 'NONE',  ( 12.22500000122903430, -5.773502691896255534, -1.060575238724906372E-15 ) ) ;
#58637 = CARTESIAN_POINT ( 'NONE',  ( 20.58750000122903145, 4.330127018922191873, 2.499999999999999556 ) ) ;
#58638 = CARTESIAN_POINT ( 'NONE',  ( 16.94062500061451715, -3.027376345333610441, -5.243569643749999898 ) ) ;
#58639 = CARTESIAN_POINT ( 'NONE',  ( 21.32812500061451644, -4.541064518000419881, 2.621784821874995952 ) ) ;
#58640 = CARTESIAN_POINT ( 'NONE',  ( 28.50000000122903288, -2.886751345948125991, -5.000000000000000000 ) ) ;
#58641 = CARTESIAN_POINT ( 'NONE',  ( 28.16249999999999787, 2.886751345948126879, 4.999999999999999112 ) ) ;
#58642 = CARTESIAN_POINT ( 'NONE',  ( 28.27499999999999858, -4.330127018922194537, 2.499999999999995559 ) ) ;
#58643 = CARTESIAN_POINT ( 'NONE',  ( 7.359375000614516438, 0.000000000000000000, 4.756430356249998326 ) ) ;
#58644 = CARTESIAN_POINT ( 'NONE',  ( 27.19687500061451857, -3.027376345333614438, 5.243569643749998122 ) ) ;
#58645 = CARTESIAN_POINT ( 'NONE',  ( 20.19375000122903430, -2.886751345948074920, 5.000000000000092371 ) ) ;
#58646 = CARTESIAN_POINT ( 'NONE',  ( -3.000416591977282496E-16, 15.24687500061451928, -34.90005215228797653 ) ) ;
#58647 = CARTESIAN_POINT ( 'NONE',  ( 3.600000001229033408, -2.886751345948129988, 4.999999999999997335 ) ) ;
#58648 = CARTESIAN_POINT ( 'NONE',  ( 6.450000000000001066, 4.330127018922192761, -2.499999999999997780 ) ) ;
#58649 = EDGE_CURVE ( 'NONE', #66176, #69731, #55504, .T. ) ;
#58650 = CARTESIAN_POINT ( 'NONE',  ( 25.72499999999999787, 6.123233995736764310E-16, -4.999999999999998224 ) ) ;
#58651 = CARTESIAN_POINT ( 'NONE',  ( 9.271875000614516082, -6.054752690667223547, -1.112240025338166033E-15 ) ) ;
#58652 = CARTESIAN_POINT ( 'NONE',  ( 28.94062500061452070, -3.027376345333614438, 5.243569643749998122 ) ) ;
#58653 = DIRECTION ( 'NONE',  ( 0.000000000000000000, 0.000000000000000000, 1.000000000000000000 ) ) ;
#58654 = CARTESIAN_POINT ( 'NONE',  ( -3.040073828171254267, 9.532700238123338110, -24.81292056264607737 ) ) ;
#58655 = CARTESIAN_POINT ( 'NONE',  ( 0.000000000000000000, 27.50000000000000000, 30.00000000000000000 ) ) ;
#58656 = CARTESIAN_POINT ( 'NONE',  ( 7.171875000614517326, 3.027376345333613106, -5.243569643749998122 ) ) ;
#58657 = CARTESIAN_POINT ( 'NONE',  ( 11.82187500061451679, 3.027376345333611329, 5.243569643749999010 ) ) ;
#58658 = CARTESIAN_POINT ( 'NONE',  ( 3.862500000000001155, 2.886751345948126879, 4.999999999999999112 ) ) ;
#58659 = VECTOR ( 'NONE', #40782, 1000.000000000000000 ) ;
#58660 = CARTESIAN_POINT ( 'NONE',  ( 2.121784821875001281, 14.10312500061459495, 33.67503911421598417 ) ) ;
#58661 = CARTESIAN_POINT ( 'NONE',  ( 2.441062857229242322, 25.34009520733920340, 26.82048057073465230 ) ) ;
#58662 = CARTESIAN_POINT ( 'NONE',  ( 5.400000000000002132, -4.330127018922190985, -2.500000000000001332 ) ) ;
#58663 = CARTESIAN_POINT ( 'NONE',  ( 15.57187500061451679, 5.824947211148865298E-16, -4.756430356249998326 ) ) ;
#58664 = CARTESIAN_POINT ( 'NONE',  ( 19.75312500061451360, 4.541064518000418104, -2.621784821874998173 ) ) ;
#58665 = CARTESIAN_POINT ( 'NONE',  ( 12.32812500061451821, -4.541064518000419881, 2.621784821874995952 ) ) ;
#58666 = CARTESIAN_POINT ( 'NONE',  ( 22.62187500061451573, -4.119189519843968306, 2.378215178124996054 ) ) ;
#58667 = CARTESIAN_POINT ( 'NONE',  ( 9.121875000614517504, 3.027376345333611329, 5.243569643749999010 ) ) ;
#58668 = CARTESIAN_POINT ( 'NONE',  ( 25.53750000000000142, -2.886751345948129988, 4.999999999999997335 ) ) ;
#58669 = CARTESIAN_POINT ( 'NONE',  ( 22.57500000122903572, -5.773502691896255534, -1.060575238724906372E-15 ) ) ;
#58670 = CARTESIAN_POINT ( 'NONE',  ( 28.76250000000000284, -5.773502691896255534, -1.060575238724906372E-15 ) ) ;
#58671 = CARTESIAN_POINT ( 'NONE',  ( 9.834375000614517859, 6.421520780324663323E-16, -5.243569643749999010 ) ) ;
#58672 = CARTESIAN_POINT ( 'NONE',  ( 25.77187500061451075, 3.027376345333611329, 5.243569643749999010 ) ) ;
#58673 = CARTESIAN_POINT ( 'NONE',  ( 3.496875000614518836, -3.027376345333610441, -5.243569643749999898 ) ) ;
#58674 = CARTESIAN_POINT ( 'NONE',  ( 20.82187500061451857, 3.027376345333611329, 5.243569643749999010 ) ) ;
#58675 = CARTESIAN_POINT ( 'NONE',  ( 10.99687500061451750, -3.027376345333614438, 5.243569643749998122 ) ) ;
#58676 = CARTESIAN_POINT ( 'NONE',  ( -3.756430356250000102, 13.31562499938548427, 30.00000000000000000 ) ) ;
#58677 = CARTESIAN_POINT ( 'NONE',  ( 23.58749999999999858, 5.773502691896255534, 3.535250795749688894E-16 ) ) ;
#58678 = CARTESIAN_POINT ( 'NONE',  ( -4.000000000000000888, 12.76250000000000284, 32.30940107675850470 ) ) ;
#58679 = CARTESIAN_POINT ( 'NONE',  ( 4.243569643749999898, 13.29687500061451644, -27.54997392385601529 ) ) ;
#58680 = CARTESIAN_POINT ( 'NONE',  ( 24.15937500061451715, -4.119189519843965641, -2.378215178125001383 ) ) ;
#58681 = CARTESIAN_POINT ( 'NONE',  ( 15.92812500061451608, -4.541064518000419881, 2.621784821874995952 ) ) ;
#58682 = CARTESIAN_POINT ( 'NONE',  ( 5.737499999999998934, -2.886751345948129988, 4.999999999999997335 ) ) ;
#58683 = LINE ( 'NONE', #12900, #30126 ) ;
#58684 = DIRECTION ( 'NONE',  ( 0.000000000000000000, 0.000000000000000000, 1.000000000000000000 ) ) ;
#58685 = CARTESIAN_POINT ( 'NONE',  ( 14.02499999999999858, 6.123233995736764310E-16, -4.999999999999998224 ) ) ;
#58686 = CARTESIAN_POINT ( 'NONE',  ( -2.828200636599751609E-16, 19.55000000122903359, 25.38119784648299770 ) ) ;
#58687 = CARTESIAN_POINT ( 'NONE',  ( 13.65000000122903323, -2.886751345948125991, -5.000000000000000000 ) ) ;
#58688 = CARTESIAN_POINT ( 'NONE',  ( 24.87187500061451573, 3.027376345333611329, 5.243569643749999010 ) ) ;
#58689 = CARTESIAN_POINT ( 'NONE',  ( 20.25000000122903288, -2.886751345948096681, 5.000000000000054179 ) ) ;
#58690 = ORIENTED_EDGE ( 'NONE', *, *, #27502, .F. ) ;
#58691 = CARTESIAN_POINT ( 'NONE',  ( 18.55312500061451431, 0.000000000000000000, 5.243569643749999010 ) ) ;
#58692 = CARTESIAN_POINT ( 'NONE',  ( 3.290625000614516793, -3.027376345333614438, 5.243569643749998122 ) ) ;
#58693 = CARTESIAN_POINT ( 'NONE',  ( 19.20937500061451786, -4.541064518000417216, -2.621784821875001281 ) ) ;
#58694 = CARTESIAN_POINT ( 'NONE',  ( 28.32187500061451502, 3.027376345333613106, -5.243569643749998122 ) ) ;
#58695 = CARTESIAN_POINT ( 'NONE',  ( 4.228125000614517681, -4.541064518000419881, 2.621784821874995952 ) ) ;
#58696 = CARTESIAN_POINT ( 'NONE',  ( 22.71562500061451573, -6.054752690667223547, -1.112240025338166033E-15 ) ) ;
#58697 = EDGE_CURVE ( 'NONE', #29564, #28631, #44960, .T. ) ;
#58698 = CARTESIAN_POINT ( 'NONE',  ( 9.001249775931846008E-16, 14.96562500061451750, 34.90005215228797653 ) ) ;
#58699 = CARTESIAN_POINT ( 'NONE',  ( 19.42500000122903714, -5.773502691896255534, -1.060575238724906372E-15 ) ) ;
#58700 = CARTESIAN_POINT ( 'NONE',  ( 12.98437500061451821, 5.824947211148865298E-16, -4.756430356249998326 ) ) ;
#58701 = CARTESIAN_POINT ( 'NONE',  ( 6.065625000614517148, -6.054752690667223547, -1.112240025338166033E-15 ) ) ;
#58702 = CARTESIAN_POINT ( 'NONE',  ( 3.196875000614516793, 6.054752690667223547, 3.707466751127219781E-16 ) ) ;
#58703 = CARTESIAN_POINT ( 'NONE',  ( 3.271875000614519635, 3.027376345333611329, 5.243569643749999010 ) ) ;
#58704 = CARTESIAN_POINT ( 'NONE',  ( 21.83437500061451786, -4.541064518000419881, 2.621784821874995952 ) ) ;
#58705 = CARTESIAN_POINT ( 'NONE',  ( 15.59062500061451573, -3.027376345333610441, -5.243569643749999898 ) ) ;
#58706 = CARTESIAN_POINT ( 'NONE',  ( 23.81250000122903288, 0.000000000000000000, 4.999999999999998224 ) ) ;
#58707 = CARTESIAN_POINT ( 'NONE',  ( 25.19062500061451715, 6.054752690667223547, 3.707466751127219781E-16 ) ) ;
#58708 = CARTESIAN_POINT ( 'NONE',  ( 19.88437500061451857, 4.541064518000418104, 2.621784821874999949 ) ) ;
#58709 = CARTESIAN_POINT ( 'NONE',  ( 15.96562500061451573, -6.054752690667223547, -1.112240025338166033E-15 ) ) ;
#58710 = CARTESIAN_POINT ( 'NONE',  ( 4.243569643749999010, 16.07187500061451857, 27.54997392385601174 ) ) ;
#58711 = CARTESIAN_POINT ( 'NONE',  ( 20.20312500061451644, 4.541064518000418104, -2.621784821874998173 ) ) ;
#58712 = CARTESIAN_POINT ( 'NONE',  ( 29.09062500061451573, -3.027376345333610441, -5.243569643749999898 ) ) ;
#58713 = VERTEX_POINT ( 'NONE', #38695 ) ;
#58714 = CARTESIAN_POINT ( 'NONE',  ( 25.31250000000000000, 2.886751345948129099, -4.999999999999998224 ) ) ;
#58715 = CARTESIAN_POINT ( 'NONE',  ( 4.000000000000000000, 11.63750000000000284, -27.69059892324149530 ) ) ;
#58716 = CARTESIAN_POINT ( 'NONE',  ( 3.756430356250000102, 19.05312499938548143, 30.00000000000000000 ) ) ;
#58717 = CARTESIAN_POINT ( 'NONE',  ( 26.95312500061451644, 4.541064518000418104, -2.621784821874998173 ) ) ;
#58718 = CARTESIAN_POINT ( 'NONE',  ( 7.153125000614518392, 4.541064518000418104, -2.621784821874998173 ) ) ;
#58719 = CARTESIAN_POINT ( 'NONE',  ( 20.85000000122903430, -2.886751345948125991, -5.000000000000000000 ) ) ;
#58720 = CARTESIAN_POINT ( 'NONE',  ( 25.37812500061451715, -4.541064518000419881, 2.621784821874995952 ) ) ;
#58721 = CARTESIAN_POINT ( 'NONE',  ( 24.71250000000000213, -5.773502691896255534, -1.060575238724906372E-15 ) ) ;
#58722 = CARTESIAN_POINT ( 'NONE',  ( -2.828200636599751609E-16, 15.50000000122903465, -34.61880215351700230 ) ) ;
#58723 =( BOUNDED_CURVE ( )  B_SPLINE_CURVE ( 2, ( #42494, #42857, #9966, #54669, #4073 ),
 .UNSPECIFIED., .F., .F. ) 
 B_SPLINE_CURVE_WITH_KNOTS ( ( 3, 2, 3 ),
 ( 0.000000000000000000, 0.009259259259259258745, 0.01388888888888888985 ),
 .UNSPECIFIED. ) 
 CURVE ( )  GEOMETRIC_REPRESENTATION_ITEM ( )  RATIONAL_B_SPLINE_CURVE ( ( 1.000000000000000000, 0.8660254037844387076, 1.000000000000000000, 0.9330127018922192983, 0.9330127018922194093 ) ) 
 REPRESENTATION_ITEM ( '' )  );
#58724 = CARTESIAN_POINT ( 'NONE',  ( 26.84062500061451573, -3.027376345333610441, -5.243569643749999898 ) ) ;
#58725 = CARTESIAN_POINT ( 'NONE',  ( 11.16562500061451679, 3.027376345333613106, -5.243569643749998122 ) ) ;
#58726 = ORIENTED_EDGE ( 'NONE', *, *, #66521, .T. ) ;
#58727 = CARTESIAN_POINT ( 'NONE',  ( 25.41562500061451146, -6.054752690667223547, -1.112240025338166033E-15 ) ) ;
#58728 = CARTESIAN_POINT ( 'NONE',  ( 6.365625000614518747, 3.027376345333611329, 5.243569643749999010 ) ) ;
#58729 = CARTESIAN_POINT ( 'NONE',  ( 15.12187500061451750, -5.492252693125287522, -1.008910452111647106E-15 ) ) ;
#58730 = CARTESIAN_POINT ( 'NONE',  ( 30.00000000000000000, 0.000000000000000000, 0.000000000000000000 ) ) ;
#58731 = CARTESIAN_POINT ( 'NONE',  ( 12.44999999999999929, 0.000000000000000000, 4.999999999999998224 ) ) ;
#58732 = EDGE_CURVE ( 'NONE', #41163, #29206, #27245, .T. ) ;
#58733 = CARTESIAN_POINT ( 'NONE',  ( 13.58437500061451786, 4.541064518000418104, 2.621784821874999949 ) ) ;
#58734 = CARTESIAN_POINT ( 'NONE',  ( 8.287500001229034297, 6.123233995736764310E-16, -4.999999999999998224 ) ) ;
#58735 = CARTESIAN_POINT ( 'NONE',  ( 17.10937500061451999, 4.541064518000418104, -2.621784821874998173 ) ) ;
#58736 = CARTESIAN_POINT ( 'NONE',  ( 16.19999999999999929, -4.330127018922190985, -2.500000000000001332 ) ) ;
#58737 = CARTESIAN_POINT ( 'NONE',  ( 8.259375000614518569, 0.000000000000000000, 5.243569643749999010 ) ) ;
#58738 = CARTESIAN_POINT ( 'NONE',  ( 4.243569643749999010, 11.51562500061451644, -32.45002607614398471 ) ) ;
#58739 = DIRECTION ( 'NONE',  ( -1.000000000000000000, -0.000000000000000000, -0.000000000000000000 ) ) ;
#58740 = CARTESIAN_POINT ( 'NONE',  ( 23.52187500061451431, -4.119189519843968306, 2.378215178124996054 ) ) ;
#58741 = ORIENTED_EDGE ( 'NONE', *, *, #18853, .F. ) ;
#58742 = CARTESIAN_POINT ( 'NONE',  ( 24.02812500061451573, -4.541064518000419881, 2.621784821874995952 ) ) ;
#58743 = CARTESIAN_POINT ( 'NONE',  ( 5.000000000000000000, 39.99999999999999289, 15.00000000000000178 ) ) ;
#58744 = CARTESIAN_POINT ( 'NONE',  ( -3.999999999999997335, 17.45000000122903572, 32.30940107675850470 ) ) ;
#58745 = CARTESIAN_POINT ( 'NONE',  ( 26.93437500061451573, 6.421520780324663323E-16, -5.243569643749999010 ) ) ;
#58746 = CARTESIAN_POINT ( 'NONE',  ( 28.69687500061451502, -3.027376345333610441, -5.243569643749999898 ) ) ;
#58747 = CARTESIAN_POINT ( 'NONE',  ( 3.515625000614516882, 3.027376345333613106, -5.243569643749998122 ) ) ;
#58748 = CARTESIAN_POINT ( 'NONE',  ( 23.14687500061451786, -4.119189519843965641, -2.378215178125001383 ) ) ;
#58749 = CARTESIAN_POINT ( 'NONE',  ( 16.77187500061451786, 3.027376345333611329, 5.243569643749999010 ) ) ;
#58750 = CARTESIAN_POINT ( 'NONE',  ( 8.371875000614515727, 5.824947211148865298E-16, -4.756430356249998326 ) ) ;
#58751 = CARTESIAN_POINT ( 'NONE',  ( 29.55000000122903003, 5.773502691896255534, 3.535250795749688894E-16 ) ) ;
#58752 = CARTESIAN_POINT ( 'NONE',  ( 9.271875000614516082, -6.054752690667223547, -1.112240025338166033E-15 ) ) ;
#58753 = CARTESIAN_POINT ( 'NONE',  ( 19.95937500061451786, 0.000000000000000000, 5.243569643749999010 ) ) ;
#58754 = CARTESIAN_POINT ( 'NONE',  ( -1.042719862598425307, 25.50793469220265663, 33.87077893255365524 ) ) ;
#58755 = CARTESIAN_POINT ( 'NONE',  ( 26.32499999999999929, 4.330127018922191873, 2.499999999999999556 ) ) ;
#58756 = CARTESIAN_POINT ( 'NONE',  ( 28.09687500061451360, -3.027376345333614438, 5.243569643749998122 ) ) ;
#58757 = CARTESIAN_POINT ( 'NONE',  ( 29.66249999999999787, -5.773502691896255534, -1.060575238724906372E-15 ) ) ;
#58758 = CARTESIAN_POINT ( 'NONE',  ( 5.700000001229034829, 5.773502691896255534, 3.535250795749688401E-16 ) ) ;
#58759 = ORIENTED_EDGE ( 'NONE', *, *, #1232, .F. ) ;
#58760 = CARTESIAN_POINT ( 'NONE',  ( 7.650000000000000355, -4.330127018922190985, -2.500000000000001332 ) ) ;
#58761 = CARTESIAN_POINT ( 'NONE',  ( 8.521875000614517859, 4.119189519843966529, 2.378215178124999607 ) ) ;
#58762 = CARTESIAN_POINT ( 'NONE',  ( 20.91562500061451502, -6.054752690667223547, -1.112240025338166033E-15 ) ) ;
#58763 = CARTESIAN_POINT ( 'NONE',  ( 12.67499999999999893, 6.123233995736764310E-16, -4.999999999999998224 ) ) ;
#58764 = CARTESIAN_POINT ( 'NONE',  ( 7.800000001229035362, -2.886751345948125991, -5.000000000000000000 ) ) ;
#58765 = CARTESIAN_POINT ( 'NONE',  ( 7.153125000614518392, 4.541064518000418104, -2.621784821874998173 ) ) ;
#58766 =( BOUNDED_CURVE ( )  B_SPLINE_CURVE ( 2, ( #16888, #50886, #17253, #26908, #44265, #32438, #33517 ),
 .UNSPECIFIED., .F., .F. ) 
 B_SPLINE_CURVE_WITH_KNOTS ( ( 3, 2, 2, 3 ),
 ( 0.5250000000000000222, 0.5277777777777777901, 0.5305555555555556690, 0.5333333333333334370 ),
 .UNSPECIFIED. ) 
 CURVE ( )  GEOMETRIC_REPRESENTATION_ITEM ( )  RATIONAL_B_SPLINE_CURVE ( ( 1.000000000000000000, 0.8660254037844387076, 1.000000000000000000, 0.8660254037844387076, 1.000000000000000000, 0.8660254037844333785, 1.000000000000005329 ) ) 
 REPRESENTATION_ITEM ( '' )  );
#58767 = CARTESIAN_POINT ( 'NONE',  ( 21.63749999999999929, -2.886751345948125991, -5.000000000000000000 ) ) ;
#58768 = CARTESIAN_POINT ( 'NONE',  ( 21.55312500061451431, 4.541064518000418104, -2.621784821874998173 ) ) ;
#58769 = CARTESIAN_POINT ( 'NONE',  ( 14.84999999999999964, -4.330127018922190985, -2.500000000000001332 ) ) ;
#58770 = CARTESIAN_POINT ( 'NONE',  ( 25.91250000122903074, 4.330127018922192761, -2.499999999999997780 ) ) ;
#58771 = CARTESIAN_POINT ( 'NONE',  ( -3.756430356249999214, 20.47812499938548569, 27.83122392262697176 ) ) ;
#58772 = CARTESIAN_POINT ( 'NONE',  ( 4.087500000000001243, -2.886751345948125991, -5.000000000000000000 ) ) ;
#58773 = ORIENTED_EDGE ( 'NONE', *, *, #65919, .F. ) ;
#58774 = CARTESIAN_POINT ( 'NONE',  ( 19.41562500061451146, 3.027376345333611329, 5.243569643749999010 ) ) ;
#58775 = CARTESIAN_POINT ( 'NONE',  ( 26.84062500061451573, -3.027376345333610441, -5.243569643749999898 ) ) ;
#58776 = CARTESIAN_POINT ( 'NONE',  ( 26.70937500061451431, 0.000000000000000000, 5.243569643749999010 ) ) ;
#58777 = CARTESIAN_POINT ( 'NONE',  ( 10.08749999999999858, 5.773502691896255534, 3.535250795749688894E-16 ) ) ;
#58778 = CARTESIAN_POINT ( 'NONE',  ( 14.91562500061451679, 3.027376345333611329, 5.243569643749999010 ) ) ;
#58779 = CARTESIAN_POINT ( 'NONE',  ( 28.86562500061451786, 3.027376345333611329, 5.243569643749999010 ) ) ;
#58780 = CARTESIAN_POINT ( 'NONE',  ( 10.00312500061451715, 0.000000000000000000, 5.243569643749999010 ) ) ;
#58781 = CARTESIAN_POINT ( 'NONE',  ( -4.243569643749999898, 10.35312500061459673, -30.00000000000000000 ) ) ;
#58782 = CARTESIAN_POINT ( 'NONE',  ( -4.243569643749999898, 12.17187500061451999, 27.54997392385601529 ) ) ;
#58783 = CARTESIAN_POINT ( 'NONE',  ( 25.50000000122903288, 5.773502691896255534, 3.535250795749688894E-16 ) ) ;
#58784 = CARTESIAN_POINT ( 'NONE',  ( 20.10937500061451289, -4.119189519843965641, -2.378215178125001383 ) ) ;
#58785 = CARTESIAN_POINT ( 'NONE',  ( 17.91562500061451502, 3.027376345333612662, -5.243569643749998122 ) ) ;
#58786 = CARTESIAN_POINT ( 'NONE',  ( 8.175000000000002487, 6.123233995736764310E-16, -4.999999999999998224 ) ) ;
#58787 = CARTESIAN_POINT ( 'NONE',  ( 10.99687500061451750, -3.027376345333614438, 5.243569643749998122 ) ) ;
#58788 = CARTESIAN_POINT ( 'NONE',  ( 10.24687500061451750, -3.027376345333610441, -5.243569643749999898 ) ) ;
#58789 = CARTESIAN_POINT ( 'NONE',  ( 17.37187500061451573, -6.054752690667223547, -1.112240025338166033E-15 ) ) ;
#58790 = VERTEX_POINT ( 'NONE', #22768 ) ;
#58791 = CARTESIAN_POINT ( 'NONE',  ( 1.071796769724489895, 13.56740381056766687, 26.00000000000000355 ) ) ;
#58792 = CARTESIAN_POINT ( 'NONE',  ( 21.44062500061452070, -3.027376345333610441, -5.243569643749999898 ) ) ;
#58793 = CARTESIAN_POINT ( 'NONE',  ( 16.39687500061451786, -3.027376345333614438, 5.243569643749998122 ) ) ;
#58794 = CARTESIAN_POINT ( 'NONE',  ( 23.16562500061451502, -6.054752690667223547, -1.112240025338166033E-15 ) ) ;
#58795 = CARTESIAN_POINT ( 'NONE',  ( 8.484601909799253346E-16, 13.36250000000000071, 34.61880215351700230 ) ) ;
#58796 = CARTESIAN_POINT ( 'NONE',  ( 27.74062500061451431, -3.027376345333610441, -5.243569643749999898 ) ) ;
#58797 = CARTESIAN_POINT ( 'NONE',  ( 8.362500001229031810, 4.330127018922192761, -2.499999999999997780 ) ) ;
#58798 = ORIENTED_EDGE ( 'NONE', *, *, #53989, .T. ) ;
#58799 = CARTESIAN_POINT ( 'NONE',  ( 4.125000001229034652, -5.773502691896255534, -1.060575238724906372E-15 ) ) ;
#58800 = CARTESIAN_POINT ( 'NONE',  ( 2.000000000000001332, 17.89999999999999858, -26.53589838486224650 ) ) ;
#58801 = CARTESIAN_POINT ( 'NONE',  ( 24.67500000122903359, 2.886751345948126879, 4.999999999999999112 ) ) ;
#58802 = CARTESIAN_POINT ( 'NONE',  ( 1.878215178125000495, 13.27812499938548285, 26.74683588394047007 ) ) ;
#58803 = CARTESIAN_POINT ( 'NONE',  ( 8.034375000614518925, 6.421520780324663323E-16, -5.243569643749999010 ) ) ;
#58804 = CARTESIAN_POINT ( 'NONE',  ( 4.000000000000000000, 15.23750000000000071, 32.30940107675849760 ) ) ;
#58805 = CARTESIAN_POINT ( 'NONE',  ( 13.86562500061451431, 3.027376345333613106, -5.243569643749998122 ) ) ;
#58806 = CARTESIAN_POINT ( 'NONE',  ( 8.371875000614515727, -6.054752690667223547, -1.112240025338166033E-15 ) ) ;
#58807 = CARTESIAN_POINT ( 'NONE',  ( 27.48750000122903359, -4.330127018922194537, 2.499999999999995559 ) ) ;
#58808 = CARTESIAN_POINT ( 'NONE',  ( 16.62187500061451573, 3.027376345333612662, -5.243569643749998122 ) ) ;
#58809 = CARTESIAN_POINT ( 'NONE',  ( 5.446875000614518569, 6.054752690667223547, 3.707466751127219781E-16 ) ) ;
#58810 = DIRECTION ( 'NONE',  ( -1.000000000000000000, -0.000000000000000000, -0.000000000000000000 ) ) ;
#58811 = CARTESIAN_POINT ( 'NONE',  ( 6.628125000614517148, 6.421520780324663323E-16, -5.243569643749999010 ) ) ;
#58812 = CARTESIAN_POINT ( 'NONE',  ( 16.90312500061451573, -4.541064518000417216, -2.621784821875001281 ) ) ;
#58813 = ORIENTED_EDGE ( 'NONE', *, *, #24066, .T. ) ;
#58814 = EDGE_CURVE ( 'NONE', #10190, #65143, #40143, .T. ) ;
#58815 = CARTESIAN_POINT ( 'NONE',  ( 13.60312500061451679, 0.000000000000000000, 5.243569643749999010 ) ) ;
#58816 = CARTESIAN_POINT ( 'NONE',  ( 6.187500001229032875, 4.330127018922191873, 2.499999999999999556 ) ) ;
#58817 = CARTESIAN_POINT ( 'NONE',  ( 11.84062500061451750, -3.027376345333614438, 5.243569643749998122 ) ) ;
#58818 = CARTESIAN_POINT ( 'NONE',  ( 21.15937500061451715, 4.119189519843966529, -2.378215178124998275 ) ) ;
#58819 = CARTESIAN_POINT ( 'NONE',  ( 10.98750000000000071, 5.773502691896255534, 3.535250795749688894E-16 ) ) ;
#58820 = CARTESIAN_POINT ( 'NONE',  ( 6.412500001229036073, -4.330127018922190985, -2.500000000000001332 ) ) ;
#58821 = ADVANCED_FACE ( 'NONE', ( #66770 ), #34579, .T. ) ;
#58822 = CARTESIAN_POINT ( 'NONE',  ( 15.08437500061451786, -4.541064518000419881, 2.621784821874995952 ) ) ;
#58823 = CARTESIAN_POINT ( 'NONE',  ( 15.30000000122903359, -2.886751345948129988, 4.999999999999997335 ) ) ;
#58824 = CARTESIAN_POINT ( 'NONE',  ( 24.44999999999999929, 4.330127018922192761, -2.499999999999997780 ) ) ;
#58825 = CARTESIAN_POINT ( 'NONE',  ( -2.121784821874996840, 18.52812500061451928, -26.32496088578401583 ) ) ;
#58826 = CARTESIAN_POINT ( 'NONE',  ( 30.00000000000000000, 0.000000000000000000, 0.000000000000000000 ) ) ;
#58827 = CARTESIAN_POINT ( 'NONE',  ( 1.071796769724484344, 14.84509619066137098, -25.99999999999999645 ) ) ;
#58828 = DIRECTION ( 'NONE',  ( 1.000000000000000000, 0.000000000000000000, 0.000000000000000000 ) ) ;
#58829 = DIRECTION ( 'NONE',  ( 0.000000000000000000, 0.000000000000000000, 1.000000000000000000 ) ) ;
#58830 = FACE_OUTER_BOUND ( 'NONE', #38389, .T. ) ;
#58831 = CARTESIAN_POINT ( 'NONE',  ( 15.64687500061451608, -3.027376345333610441, -5.243569643749999898 ) ) ;
#58832 = EDGE_CURVE ( 'NONE', #54070, #2091, #63035, .T. ) ;
#58833 = CARTESIAN_POINT ( 'NONE',  ( 28.16249999999999787, 2.886751345948126879, 4.999999999999999112 ) ) ;
#58834 = CARTESIAN_POINT ( 'NONE',  ( 13.86562500061451431, 3.027376345333613106, -5.243569643749998122 ) ) ;
#58835 = CARTESIAN_POINT ( 'NONE',  ( 28.54687500061451644, -4.119189519843965641, -2.378215178125001383 ) ) ;
#58836 = CARTESIAN_POINT ( 'NONE',  ( 23.93437500061451573, 4.541064518000418104, 2.621784821874999949 ) ) ;
#58837 = CARTESIAN_POINT ( 'NONE',  ( 15.45937500061451608, -5.492252693125287522, -1.008910452111647106E-15 ) ) ;
#58838 = CARTESIAN_POINT ( 'NONE',  ( 10.04062500061451502, -3.027376345333614438, 5.243569643749998122 ) ) ;
#58839 = CARTESIAN_POINT ( 'NONE',  ( 14.44687500061451679, 6.054752690667223547, 3.707466751127219781E-16 ) ) ;
#58840 = VERTEX_POINT ( 'NONE', #45320 ) ;
#58841 = CARTESIAN_POINT ( 'NONE',  ( 25.88437500061451502, -4.541064518000419881, 2.621784821874995952 ) ) ;
#58842 = CARTESIAN_POINT ( 'NONE',  ( 27.81562500061452070, 3.027376345333613106, -5.243569643749998122 ) ) ;
#58843 = CARTESIAN_POINT ( 'NONE',  ( 18.21562500061451573, -6.054752690667223547, -1.112240025338166033E-15 ) ) ;
#58844 = CARTESIAN_POINT ( 'NONE',  ( 28.49062500061451431, -3.027376345333614438, 5.243569643749998122 ) ) ;
#58845 = CARTESIAN_POINT ( 'NONE',  ( 4.849693137238607399, 1.216928655869232712, -5.100445426819982586 ) ) ;
#58846 = CARTESIAN_POINT ( 'NONE',  ( 8.550000000000002487, -4.330127018922190985, -2.500000000000001332 ) ) ;
#58847 = CARTESIAN_POINT ( 'NONE',  ( 19.68750000122903288, 4.330127018922191873, 2.499999999999999556 ) ) ;
#58848 = CARTESIAN_POINT ( 'NONE',  ( -1.999999999999997113, 10.17500000000000249, 33.46410161513775705 ) ) ;
#58849 = CARTESIAN_POINT ( 'NONE',  ( 8.409375000614517148, 2.746126346562645981, -4.756430356249997438 ) ) ;
#58850 = ORIENTED_EDGE ( 'NONE', *, *, #54130, .T. ) ;
#58851 = CARTESIAN_POINT ( 'NONE',  ( 15.11249999999999893, 2.886751345948126879, 4.999999999999999112 ) ) ;
#58852 = CARTESIAN_POINT ( 'NONE',  ( 18.30000000000000071, 0.000000000000000000, 4.999999999999998224 ) ) ;
#58853 = CARTESIAN_POINT ( 'NONE',  ( 16.47187500061452070, -6.054752690667223547, -1.112240025338166033E-15 ) ) ;
#58854 = CARTESIAN_POINT ( 'NONE',  ( 13.45312500061451466, 4.541064518000418104, -2.621784821874998173 ) ) ;
#58855 = ORIENTED_EDGE ( 'NONE', *, *, #58478, .F. ) ;
#58856 = DIRECTION ( 'NONE',  ( -1.000000000000000000, -0.000000000000000000, -0.000000000000000000 ) ) ;
#58857 = CARTESIAN_POINT ( 'NONE',  ( 6.215625000614517504, 3.027376345333613106, -5.243569643749998122 ) ) ;
#58858 = CARTESIAN_POINT ( 'NONE',  ( 1.071796769724491893, 12.03259618943233455, 33.99999999999999289 ) ) ;
#58859 = CARTESIAN_POINT ( 'NONE',  ( 11.81250000000000000, 2.886751345948129099, -4.999999999999998224 ) ) ;
#58860 = CARTESIAN_POINT ( 'NONE',  ( 29.52187500061451431, 5.824947211148865298E-16, -4.756430356249998326 ) ) ;
#58861 = CARTESIAN_POINT ( 'NONE',  ( 2.121784821875001281, 15.00312500061451715, 33.67503911421598417 ) ) ;
#58862 = CARTESIAN_POINT ( 'NONE',  ( 26.27812500061451573, -4.541064518000419881, 2.621784821874995952 ) ) ;
#58863 = CARTESIAN_POINT ( 'NONE',  ( 7.687500000000000000, -2.886751345948125991, -5.000000000000000000 ) ) ;
#58864 = CARTESIAN_POINT ( 'NONE',  ( 3.756430356250000102, 17.59062499938548285, 30.00000000000000000 ) ) ;
#58865 = CARTESIAN_POINT ( 'NONE',  ( 23.97187500061451360, 3.027376345333611329, 5.243569643749999010 ) ) ;
#58866 = CARTESIAN_POINT ( 'NONE',  ( 20.72812500061451502, 4.541064518000418104, 2.621784821874999949 ) ) ;
#58867 = CARTESIAN_POINT ( 'NONE',  ( -4.243569643749999898, 15.26562500061459282, -32.45002607614398471 ) ) ;
#58868 = CARTESIAN_POINT ( 'NONE',  ( 23.77500000122903145, 2.886751345948126879, 4.999999999999999112 ) ) ;
#58869 = CARTESIAN_POINT ( 'NONE',  ( 6.965625000614518392, -6.054752690667223547, -1.112240025338166033E-15 ) ) ;
#58870 = CARTESIAN_POINT ( 'NONE',  ( 25.65937500061451715, 4.119189519843966529, -2.378215178124998275 ) ) ;
#58871 = CARTESIAN_POINT ( 'NONE',  ( 24.25312500061451715, 4.541064518000418104, -2.621784821874998173 ) ) ;
#58872 = CARTESIAN_POINT ( 'NONE',  ( 10.99687500061451750, -2.746126346562646425, 4.756430356249996549 ) ) ;
#58873 = CARTESIAN_POINT ( 'NONE',  ( -3.756430356250001434, 16.50312499938548783, 32.16877607737301048 ) ) ;
#58874 = CARTESIAN_POINT ( 'NONE',  ( 16.17187500061451644, 3.027376345333613106, -5.243569643749998122 ) ) ;
#58875 = CARTESIAN_POINT ( 'NONE',  ( 25.13437500061451502, 6.421520780324663323E-16, -5.243569643749999010 ) ) ;
#58876 = CARTESIAN_POINT ( 'NONE',  ( 2.121784821874999061, 14.30937500061451750, 26.32496088578401583 ) ) ;
#58877 = CARTESIAN_POINT ( 'NONE',  ( 6.103125000614515905, -4.541064518000417216, -2.621784821875001281 ) ) ;
#58878 = CARTESIAN_POINT ( 'NONE',  ( 28.86562500061451786, 3.027376345333611329, 5.243569643749999010 ) ) ;
#58879 = CARTESIAN_POINT ( 'NONE',  ( 3.084375000614519191, 6.421520780324663323E-16, -5.243569643749999010 ) ) ;
#58880 = CARTESIAN_POINT ( 'NONE',  ( 26.58749999999999858, -2.886751345948126435, -5.000000000000000000 ) ) ;
#58881 = CARTESIAN_POINT ( 'NONE',  ( 0.2033016277077263623, 10.00000000000000355, -36.00000000000001421 ) ) ;
#58882 = CARTESIAN_POINT ( 'NONE',  ( 3.440625000614518036, -3.027376345333610441, -5.243569643749999898 ) ) ;
#58883 = CARTESIAN_POINT ( 'NONE',  ( 6.421875000614519102, 3.027376345333611329, 5.243569643749999010 ) ) ;
#58884 = SURFACE_STYLE_USAGE ( .BOTH. , #63355 ) ;
#58885 = CARTESIAN_POINT ( 'NONE',  ( 17.77500000122903145, 2.886751345948129099, -4.999999999999998224 ) ) ;
#58886 = CARTESIAN_POINT ( 'NONE',  ( 4.059375000614519280, 4.541064518000418104, -2.621784821874998173 ) ) ;
#58887 = CARTESIAN_POINT ( 'NONE',  ( 5.390625000614518214, 6.054752690667223547, 3.707466751127219781E-16 ) ) ;
#58888 = CARTESIAN_POINT ( 'NONE',  ( 4.000000000000000000, 12.89374999877096606, 30.00000000000000000 ) ) ;
#58889 = CARTESIAN_POINT ( 'NONE',  ( 21.95625000122903003, 0.000000000000000000, 4.999999999999998224 ) ) ;
#58890 = CARTESIAN_POINT ( 'NONE',  ( 13.32187500061451502, -6.054752690667223547, -1.112240025338166033E-15 ) ) ;
#58891 = DIRECTION ( 'NONE',  ( 0.000000000000000000, 0.000000000000000000, -1.000000000000000000 ) ) ;
#58892 = ORIENTED_EDGE ( 'NONE', *, *, #18647, .T. ) ;
#58893 = CARTESIAN_POINT ( 'NONE',  ( 23.31562500061451715, 3.027376345333613106, -5.243569643749998122 ) ) ;
#58894 = CARTESIAN_POINT ( 'NONE',  ( 7.790625000614518569, -3.027376345333614438, 5.243569643749998122 ) ) ;
#58895 = CARTESIAN_POINT ( 'NONE',  ( 23.52187500061451786, 3.027376345333611329, 5.243569643749999010 ) ) ;
#58896 = CARTESIAN_POINT ( 'NONE',  ( 7.528125000614515727, 6.421520780324663323E-16, -5.243569643749999010 ) ) ;
#58897 = CARTESIAN_POINT ( 'NONE',  ( 10.16250000122903252, 4.330127018922192761, -2.499999999999997780 ) ) ;
#58898 = CARTESIAN_POINT ( 'NONE',  ( 25.64062500061451644, 6.054752690667223547, 3.707466751127219781E-16 ) ) ;
#58899 = CARTESIAN_POINT ( 'NONE',  ( -2.121784821874996840, 10.42812500061451786, -26.32496088578401583 ) ) ;
#58900 = CARTESIAN_POINT ( 'NONE',  ( 9.600000001229034297, -2.886751345948125991, -5.000000000000000000 ) ) ;
#58901 = CARTESIAN_POINT ( 'NONE',  ( 21.17812500061451431, 4.541064518000418104, 2.621784821874999949 ) ) ;
#58902 = CARTESIAN_POINT ( 'NONE',  ( 18.21562500061451573, -6.054752690667223547, -1.112240025338166033E-15 ) ) ;
#58903 = B_SPLINE_CURVE_WITH_KNOTS ( 'NONE', 3,
 ( #71211, #20588, #26147, #9158, #43514, #38324, #9886, #61224, #27253, #21327 ),
 .UNSPECIFIED., .F., .F.,
 ( 4, 3, 3, 4 ),
 ( 0.000000000000000000, 0.0001572280391461213552, 0.0003263780256893500592, 0.0004955716359015445178 ),
 .UNSPECIFIED. ) ;
#58904 = CARTESIAN_POINT ( 'NONE',  ( 28.43437500061451573, 4.119189519843966529, 2.378215178124999607 ) ) ;
#58905 = EDGE_CURVE ( 'NONE', #44084, #38296, #22051, .T. ) ;
#58906 = CARTESIAN_POINT ( 'NONE',  ( 17.51249999999999929, -5.773502691896255534, -1.060575238724906372E-15 ) ) ;
#58907 = CARTESIAN_POINT ( 'NONE',  ( 13.05000000122903536, -2.886751345948129988, 4.999999999999997335 ) ) ;
#58908 = CARTESIAN_POINT ( 'NONE',  ( 10.45312500061451644, 0.000000000000000000, 5.243569643749999010 ) ) ;
#58909 = CARTESIAN_POINT ( 'NONE',  ( 12.62812500061451537, 4.541064518000418104, 2.621784821874999949 ) ) ;
#58910 = CARTESIAN_POINT ( 'NONE',  ( 22.65000000122903856, -2.886751345948125991, -5.000000000000000000 ) ) ;
#58911 = CARTESIAN_POINT ( 'NONE',  ( 21.04687500061451644, -3.027376345333610441, -5.243569643749999898 ) ) ;
#58912 = CARTESIAN_POINT ( 'NONE',  ( 20.93437500061451573, -4.541064518000419881, 2.621784821874995952 ) ) ;
#58913 = CARTESIAN_POINT ( 'NONE',  ( 3.559376264448871563, 3.511538523441492199, -3.894120815303806271 ) ) ;
#58914 = CARTESIAN_POINT ( 'NONE',  ( 7.612500001229035362, 0.000000000000000000, 4.999999999999998224 ) ) ;
#58915 = CARTESIAN_POINT ( 'NONE',  ( 6.721875000614518925, 3.027376345333613106, -5.243569643749998122 ) ) ;
#58916 = CARTESIAN_POINT ( 'NONE',  ( 22.88437500061451857, 6.421520780324663323E-16, -5.243569643749999010 ) ) ;
#58917 =( BOUNDED_CURVE ( )  B_SPLINE_CURVE ( 2, ( #8584, #70279, #30749, #70639, #53652, #7856, #19650, #13378, #2319 ),
 .UNSPECIFIED., .F., .F. ) 
 B_SPLINE_CURVE_WITH_KNOTS ( ( 3, 2, 2, 2, 3 ),
 ( 0.7638888888888889506, 0.7685185185185184897, 0.7777777777777777901, 0.7870370370370370905, 0.7916666666666667407 ),
 .UNSPECIFIED. ) 
 CURVE ( )  GEOMETRIC_REPRESENTATION_ITEM ( )  RATIONAL_B_SPLINE_CURVE ( ( 0.9330127018922192983, 0.9330127018922200755, 1.000000000000000000, 0.8660254037844387076, 1.000000000000000000, 0.8660254037844387076, 1.000000000000000000, 0.9330127018922185211, 0.9330127018922192983 ) ) 
 REPRESENTATION_ITEM ( '' )  );
#58918 = CARTESIAN_POINT ( 'NONE',  ( 4.479244028039631509, 2.221994555042201114, -4.723416822329412845 ) ) ;
#58919 = CARTESIAN_POINT ( 'NONE',  ( 20.54062500061451502, -3.027376345333610441, -5.243569643749999898 ) ) ;
#58920 = CARTESIAN_POINT ( 'NONE',  ( 23.82187500061451502, 3.027376345333613106, -5.243569643749998122 ) ) ;
#58921 = CARTESIAN_POINT ( 'NONE',  ( 3.756430356250000102, 18.60312499938548214, 30.00000000000000000 ) ) ;
#58922 = CYLINDRICAL_SURFACE ( 'NONE', #53906, 4.999999999999998224 ) ;
#58923 = CARTESIAN_POINT ( 'NONE',  ( -1.071796769724491005, 13.27009619066136636, -34.00000000000000000 ) ) ;
#58924 = CARTESIAN_POINT ( 'NONE',  ( 5.334375000614517859, 6.421520780324663323E-16, -5.243569643749999010 ) ) ;
#58925 = CARTESIAN_POINT ( 'NONE',  ( 17.87812500061451715, 6.421520780324663323E-16, -5.243569643749999010 ) ) ;
#58926 = ORIENTED_EDGE ( 'NONE', *, *, #65415, .T. ) ;
#58927 = CARTESIAN_POINT ( 'NONE',  ( 25.27499999999999858, 6.123233995736764310E-16, -4.999999999999998224 ) ) ;
#58928 = CARTESIAN_POINT ( 'NONE',  ( 25.41562500061451146, -6.054752690667223547, -1.112240025338166033E-15 ) ) ;
#58929 = CARTESIAN_POINT ( 'NONE',  ( 3.534375000614518036, 6.421520780324663323E-16, -5.243569643749999010 ) ) ;
#58930 = PRODUCT_DEFINITION ( 'UNKNOWN', '', #9662, #24025 ) ;
#58931 = CARTESIAN_POINT ( 'NONE',  ( 4.765225409100392717, 1.514895174305637138, 4.789578167053410773 ) ) ;
#58932 = CARTESIAN_POINT ( 'NONE',  ( 1.592000809091587073E-14, 16.40000000122903501, -34.00000000000000000 ) ) ;
#58933 = CARTESIAN_POINT ( 'NONE',  ( 15.56250000000000000, 2.886751345948126879, 4.999999999999999112 ) ) ;
#58934 = CARTESIAN_POINT ( 'NONE',  ( 19.82812500061451644, 4.541064518000418104, 2.621784821874999949 ) ) ;
#58935 = EDGE_LOOP ( 'NONE', ( #10394, #17877, #70224, #39710 ) ) ;
#58936 = CARTESIAN_POINT ( 'NONE',  ( 23.69999999999999929, 0.000000000000000000, 4.999999999999998224 ) ) ;
#58937 = CARTESIAN_POINT ( 'NONE',  ( 27.12187500061451573, 3.027376345333611329, 5.243569643749999010 ) ) ;
#58938 = ORIENTED_EDGE ( 'NONE', *, *, #73107, .T. ) ;
#58939 = CYLINDRICAL_SURFACE ( 'NONE', #47777, 4.999999999999998224 ) ;
#58940 = CARTESIAN_POINT ( 'NONE',  ( 12.25312500061451537, 0.000000000000000000, 5.243569643749999010 ) ) ;
#58941 = CARTESIAN_POINT ( 'NONE',  ( 17.52187500061451431, 4.119189519843966529, 2.378215178124999607 ) ) ;
#58942 = CARTESIAN_POINT ( 'NONE',  ( 28.37812500061451715, 4.541064518000418104, 2.621784821874999949 ) ) ;
#58943 = CARTESIAN_POINT ( 'NONE',  ( 12.41250000122903430, 4.330127018922192761, -2.499999999999997780 ) ) ;
#58944 = CARTESIAN_POINT ( 'NONE',  ( 18.89999999999999858, -4.330127018922190985, -2.500000000000001332 ) ) ;
#58945 = CARTESIAN_POINT ( 'NONE',  ( 26.43750000000000000, -2.886751345948129988, 4.999999999999997335 ) ) ;
#58946 = CARTESIAN_POINT ( 'NONE',  ( 3.234375000614516438, 4.541064518000418104, 2.621784821874999949 ) ) ;
#58947 = CARTESIAN_POINT ( 'NONE',  ( 5.784375000614517148, 6.421520780324663323E-16, -5.243569643749999010 ) ) ;
#58948 = CARTESIAN_POINT ( 'NONE',  ( 19.73437500061451644, 6.421520780324663323E-16, -5.243569643749999010 ) ) ;
#58949 = CARTESIAN_POINT ( 'NONE',  ( 19.95000000122903216, -2.886751345948159742, -4.999999999999942268 ) ) ;
#58950 = ORIENTED_EDGE ( 'NONE', *, *, #22378, .T. ) ;
#58951 = CARTESIAN_POINT ( 'NONE',  ( 28.82812500061451644, 4.541064518000418104, 2.621784821874999949 ) ) ;
#58952 = CARTESIAN_POINT ( 'NONE',  ( 29.33437500061451431, 4.541064518000418104, 2.621784821874999949 ) ) ;
#58953 = CARTESIAN_POINT ( 'NONE',  ( 4.546875000614517326, 6.054752690667223547, 3.707466751127219781E-16 ) ) ;
#58954 = CARTESIAN_POINT ( 'NONE',  ( 16.27499999999999858, 6.123233995736764310E-16, -4.999999999999998224 ) ) ;
#58955 = CARTESIAN_POINT ( 'NONE',  ( 14.87812500061451537, 4.541064518000418104, 2.621784821874999949 ) ) ;
#58956 = CARTESIAN_POINT ( 'NONE',  ( -1.487416814333745711E-14, 15.16250000000000142, -26.00000000000000000 ) ) ;
#58957 = LINE ( 'NONE', #31263, #12413 ) ;
#58958 = CARTESIAN_POINT ( 'NONE',  ( -3.137519842735245283E-14, 12.57500000122903572, 34.00000000000000000 ) ) ;
#58959 = CARTESIAN_POINT ( 'NONE',  ( 17.73750000122903359, 6.123233995736764310E-16, -4.999999999999998224 ) ) ;
#58960 = CYLINDRICAL_SURFACE ( 'NONE', #19461, 3.999999999999996447 ) ;
#58961 = CARTESIAN_POINT ( 'NONE',  ( 16.58437500061451786, 5.824947211148865298E-16, -4.756430356249998326 ) ) ;
#58962 = CARTESIAN_POINT ( 'NONE',  ( 7.228125000614517681, 4.541064518000418104, 2.621784821874999949 ) ) ;
#58963 = CARTESIAN_POINT ( 'NONE',  ( 23.14687500061451786, -3.027376345333614438, 5.243569643749998122 ) ) ;
#58964 = CARTESIAN_POINT ( 'NONE',  ( 30.00000000000000000, 0.000000000000000000, 0.000000000000000000 ) ) ;
#58965 = CARTESIAN_POINT ( 'NONE',  ( 24.53437500061451715, -4.541064518000419881, 2.621784821874995952 ) ) ;
#58966 = CARTESIAN_POINT ( 'NONE',  ( 5.212500000000002132, 2.886751345948126879, 4.999999999999999112 ) ) ;
#58967 = CARTESIAN_POINT ( 'NONE',  ( 1.999999999999998668, 10.51250000122903572, 26.53589838486224650 ) ) ;
#58968 = CARTESIAN_POINT ( 'NONE',  ( 15.36562500061451608, 3.027376345333611329, 5.243569643749999010 ) ) ;
#58969 = CARTESIAN_POINT ( 'NONE',  ( 4.912500001229034297, 0.000000000000000000, 4.999999999999998224 ) ) ;
#58970 = ADVANCED_FACE ( 'NONE', ( #39787 ), #73029, .T. ) ;
#58971 = CARTESIAN_POINT ( 'NONE',  ( 10.54687500061451644, -3.027376345333614438, 5.243569643749998122 ) ) ;
#58972 = CARTESIAN_POINT ( 'NONE',  ( -3.457895701286862522, 3.616202803579613434, -27.97416577253550685 ) ) ;
#58973 = VERTEX_POINT ( 'NONE', #68220 ) ;
#58974 = CARTESIAN_POINT ( 'NONE',  ( 12.25312500061451537, 0.000000000000000000, 5.243569643749999010 ) ) ;
#58975 = CARTESIAN_POINT ( 'NONE',  ( 2.000000000000001332, 12.16250000122903430, -26.53589838486224650 ) ) ;
#58976 = CARTESIAN_POINT ( 'NONE',  ( 22.95000000122903216, -2.886751345948129988, 4.999999999999997335 ) ) ;
#58977 = CARTESIAN_POINT ( 'NONE',  ( 9.459375000614517859, 4.541064518000418104, -2.621784821874998173 ) ) ;
#58978 = AXIS2_PLACEMENT_3D ( 'NONE', #53866, #65665, #19861 ) ;
#58979 = CARTESIAN_POINT ( 'NONE',  ( 13.04062500061451502, 6.054752690667223547, 3.707466751127219781E-16 ) ) ;
#58980 = CARTESIAN_POINT ( 'NONE',  ( 28.70625000122903003, 0.000000000000000000, 4.999999999999998224 ) ) ;
#58981 = CARTESIAN_POINT ( 'NONE',  ( 24.38437500061451502, 4.541064518000418104, 2.621784821874999949 ) ) ;
#58982 = DIRECTION ( 'NONE',  ( 0.000000000000000000, 0.000000000000000000, 1.000000000000000000 ) ) ;
#58983 =( BOUNDED_CURVE ( )  B_SPLINE_CURVE ( 2, ( #48865, #20771, #43327, #15590, #44431, #16325, #66959, #21869, #11158 ),
 .UNSPECIFIED., .F., .F. ) 
 B_SPLINE_CURVE_WITH_KNOTS ( ( 3, 2, 2, 2, 3 ),
 ( 0.06944444444444444753, 0.07407407407407406996, 0.08333333333333332871, 0.09259259259259258745, 0.09722222222222222376 ),
 .UNSPECIFIED. ) 
 CURVE ( )  GEOMETRIC_REPRESENTATION_ITEM ( )  RATIONAL_B_SPLINE_CURVE ( ( 0.9330127018922192983, 0.9330127018922194093, 1.000000000000000000, 0.8660254037844387076, 1.000000000000000000, 0.8660254037844387076, 1.000000000000000000, 0.9330127018922191873, 0.9330127018922192983 ) ) 
 REPRESENTATION_ITEM ( '' )  );
#58984 = CARTESIAN_POINT ( 'NONE',  ( 4.350000001229034297, 5.773502691896255534, 3.535250795749688401E-16 ) ) ;
#58985 = FACE_OUTER_BOUND ( 'NONE', #52463, .T. ) ;
#58986 = CARTESIAN_POINT ( 'NONE',  ( 9.001249775931846008E-16, 13.67187500061451999, -25.09994784771203058 ) ) ;
#58987 = CARTESIAN_POINT ( 'NONE',  ( 15.94687500061451502, -3.027376345333614438, 5.243569643749998122 ) ) ;
#58988 = CARTESIAN_POINT ( 'NONE',  ( 16.72500000122903430, -5.773502691896255534, -1.060575238724906372E-15 ) ) ;
#58989 = CARTESIAN_POINT ( 'NONE',  ( 11.70937500061451608, 4.541064518000418104, -2.621784821874998173 ) ) ;
#58990 = CARTESIAN_POINT ( 'NONE',  ( 2.121784821874999061, 18.30312500061451431, -33.67503911421598417 ) ) ;
#58991 = CARTESIAN_POINT ( 'NONE',  ( 19.61250000122903359, 4.330127018922192761, -2.499999999999997780 ) ) ;
#58992 = CARTESIAN_POINT ( 'NONE',  ( 13.64062500061451644, -3.027376345333614438, 5.243569643749998122 ) ) ;
#58993 = ORIENTED_EDGE ( 'NONE', *, *, #70507, .T. ) ;
#58994 = CARTESIAN_POINT ( 'NONE',  ( 15.00000000000000000, 4.330127018922192761, -2.499999999999997780 ) ) ;
#58995 = CARTESIAN_POINT ( 'NONE',  ( 13.35937500061451821, -4.541064518000417216, -2.621784821875001281 ) ) ;
#58996 = ADVANCED_FACE ( 'NONE', ( #67854 ), #62303, .F. ) ;
#58997 = FACE_OUTER_BOUND ( 'NONE', #72844, .T. ) ;
#58998 = CARTESIAN_POINT ( 'NONE',  ( 12.45000000122903394, 5.773502691896255534, 3.535250795749688894E-16 ) ) ;
#58999 = CARTESIAN_POINT ( 'NONE',  ( 20.28750000122903074, -4.330127018922194537, 2.499999999999995559 ) ) ;
#59000 = CARTESIAN_POINT ( 'NONE',  ( 17.80312500061451786, -4.541064518000417216, -2.621784821875001281 ) ) ;
#59001 = CARTESIAN_POINT ( 'NONE',  ( 20.69062500061451715, 6.054752690667223547, 3.707466751127219781E-16 ) ) ;
#59002 = CARTESIAN_POINT ( 'NONE',  ( 27.41250000122903430, 0.000000000000000000, 4.999999999999998224 ) ) ;
#59003 =( BOUNDED_CURVE ( )  B_SPLINE_CURVE ( 2, ( #19607, #70601, #58769, #42164, #58403, #24795, #47338 ),
 .UNSPECIFIED., .F., .F. ) 
 B_SPLINE_CURVE_WITH_KNOTS ( ( 3, 2, 2, 3 ),
 ( 0.5583333333333333481, 0.5611111111111111160, 0.5638888888888889950, 0.5666666666666667629 ),
 .UNSPECIFIED. ) 
 CURVE ( )  GEOMETRIC_REPRESENTATION_ITEM ( )  RATIONAL_B_SPLINE_CURVE ( ( 1.000000000000000000, 0.8660254037844387076, 1.000000000000000000, 0.8660254037844387076, 1.000000000000000000, 0.8660254037844333785, 1.000000000000005329 ) ) 
 REPRESENTATION_ITEM ( '' )  );
#59004 = CARTESIAN_POINT ( 'NONE',  ( 25.94999999999999929, 0.000000000000000000, 4.999999999999998224 ) ) ;
#59005 = CARTESIAN_POINT ( 'NONE',  ( 3.709174336338540989, 3.352913023424228811, 4.031500572517469294 ) ) ;
#59006 = CARTESIAN_POINT ( 'NONE',  ( 7.884375000614517681, -4.119189519843968306, 2.378215178124996054 ) ) ;
#59007 = CARTESIAN_POINT ( 'NONE',  ( 28.84687500061452070, 6.054752690667223547, 3.707466751127219781E-16 ) ) ;
#59008 = CARTESIAN_POINT ( 'NONE',  ( 28.83750000000000213, -2.886751345948155745, -4.999999999999948486 ) ) ;
#59009 = CARTESIAN_POINT ( 'NONE',  ( 4.243569643749999898, 13.74687500061451750, -27.54997392385601529 ) ) ;
#59010 = EDGE_CURVE ( 'NONE', #18738, #34725, #17227, .T. ) ;
#59011 = CARTESIAN_POINT ( 'NONE',  ( 3.412500001229032964, 4.330127018922192761, -2.499999999999997780 ) ) ;
#59012 = CARTESIAN_POINT ( 'NONE',  ( 5.100000000000000533, 4.330127018922192761, -2.499999999999997780 ) ) ;
#59013 = CARTESIAN_POINT ( 'NONE',  ( 2.662500001229036073, 0.000000000000000000, 4.999999999999998224 ) ) ;
#59014 = CARTESIAN_POINT ( 'NONE',  ( 8.446875000614518569, -3.027376345333610441, -5.243569643749999898 ) ) ;
#59015 = CARTESIAN_POINT ( 'NONE',  ( 27.55312500061451786, 0.000000000000000000, 5.243569643749999010 ) ) ;
#59016 =( BOUNDED_CURVE ( )  B_SPLINE_CURVE ( 2, ( #19120, #13584, #14322, #53118, #19858, #3253, #36857 ),
 .UNSPECIFIED., .F., .F. ) 
 B_SPLINE_CURVE_WITH_KNOTS ( ( 3, 2, 2, 3 ),
 ( 0.1099999999999999312, 0.1133333333333333137, 0.1166666666666666963, 0.1200000000000000788 ),
 .UNSPECIFIED. ) 
 CURVE ( )  GEOMETRIC_REPRESENTATION_ITEM ( )  RATIONAL_B_SPLINE_CURVE ( ( 1.000000000000002887, 0.8660254037844359321, 1.000000000000000000, 0.8660254037844387076, 1.000000000000000000, 0.8660254037844353769, 1.000000000000003331 ) ) 
 REPRESENTATION_ITEM ( '' )  );
#59017 = CARTESIAN_POINT ( 'NONE',  ( 30.00000000000000000, 0.000000000000000000, 0.000000000000000000 ) ) ;
#59018 = CARTESIAN_POINT ( 'NONE',  ( 5.362500001229033586, 0.000000000000000000, 4.999999999999998224 ) ) ;
#59019 = CARTESIAN_POINT ( 'NONE',  ( 16.91250000122903430, 4.330127018922192761, -2.499999999999997780 ) ) ;
#59020 = CARTESIAN_POINT ( 'NONE',  ( 5.746875000614517504, -3.027376345333610441, -5.243569643749999898 ) ) ;
#59021 = CARTESIAN_POINT ( 'NONE',  ( 12.42187500061451821, -6.054752690667223547, -1.112240025338166033E-15 ) ) ;
#59022 = CARTESIAN_POINT ( 'NONE',  ( 3.374999999999999556, 4.330127018922191873, 2.499999999999999556 ) ) ;
#59023 = CARTESIAN_POINT ( 'NONE',  ( -3.000416591977282496E-16, 15.64062500061459282, 25.09994784771203058 ) ) ;
#59024 = CARTESIAN_POINT ( 'NONE',  ( 2.000000000000000444, 13.47500000000000142, 26.53589838486224650 ) ) ;
#59025 = CARTESIAN_POINT ( 'NONE',  ( 7.687500000000000000, -2.886751345948125991, -5.000000000000000000 ) ) ;
#59026 = CARTESIAN_POINT ( 'NONE',  ( 16.32187500061451502, -4.119189519843968306, 2.378215178124996054 ) ) ;
#59027 = CARTESIAN_POINT ( 'NONE',  ( 21.17812500061451431, 4.541064518000418104, 2.621784821874999949 ) ) ;
#59028 = CARTESIAN_POINT ( 'NONE',  ( 14.01562500061451644, 3.027376345333611329, 5.243569643749999010 ) ) ;
#59029 = CARTESIAN_POINT ( 'NONE',  ( 22.73437500061451999, -2.746126346562642428, -4.756430356249999214 ) ) ;
#59030 = CARTESIAN_POINT ( 'NONE',  ( 8.784375000614518925, -4.541064518000419881, 2.621784821874995952 ) ) ;
#59031 = CARTESIAN_POINT ( 'NONE',  ( 26.25000000000000000, 4.330127018922192761, -2.499999999999997780 ) ) ;
#59032 = CARTESIAN_POINT ( 'NONE',  ( 21.00000000122903288, 5.773502691896255534, 3.535250795749688894E-16 ) ) ;
#59033 = CARTESIAN_POINT ( 'NONE',  ( 27.89062500061451289, 6.054752690667223547, 3.707466751127219781E-16 ) ) ;
#59034 = CARTESIAN_POINT ( 'NONE',  ( 9.528763966825557376E-15, 17.07500000122903572, 34.00000000000000000 ) ) ;
#59035 = CARTESIAN_POINT ( 'NONE',  ( 9.159375000614515372, 0.000000000000000000, 5.243569643749999010 ) ) ;
#59036 = CARTESIAN_POINT ( 'NONE',  ( 14.44687500061451679, 6.054752690667223547, 3.707466751127219781E-16 ) ) ;
#59037 = CARTESIAN_POINT ( 'NONE',  ( 27.00937500061451857, 4.541064518000418104, -2.621784821874998173 ) ) ;
#59038 = CARTESIAN_POINT ( 'NONE',  ( 24.65625000122903288, 0.000000000000000000, 4.999999999999998224 ) ) ;
#59039 = CARTESIAN_POINT ( 'NONE',  ( 20.37187500061451573, 3.027376345333611329, 5.243569643749999010 ) ) ;
#59040 = CARTESIAN_POINT ( 'NONE',  ( 10.77187500061451786, 3.027376345333613106, -5.243569643749998122 ) ) ;
#59041 = CARTESIAN_POINT ( 'NONE',  ( -3.756430356249999214, 19.69062499938548427, 27.83122392262697531 ) ) ;
#59042 = CARTESIAN_POINT ( 'NONE',  ( 24.11249999999999716, 2.886751345948126879, 4.999999999999999112 ) ) ;
#59043 = CARTESIAN_POINT ( 'NONE',  ( 4.000000000000000000, 13.88750000000000107, 27.69059892324149530 ) ) ;
#59044 = CARTESIAN_POINT ( 'NONE',  ( -4.243569643749997233, 12.24687500061451928, -27.54997392385601174 ) ) ;
#59045 = CARTESIAN_POINT ( 'NONE',  ( 25.05937500061451573, -4.119189519843965641, -2.378215178125001383 ) ) ;
#59046 = CARTESIAN_POINT ( 'NONE',  ( 14.84062500061451750, 6.054752690667223547, 3.707466751127219781E-16 ) ) ;
#59047 = CARTESIAN_POINT ( 'NONE',  ( 3.562500000000000444, -5.773502691896255534, -1.060575238724906372E-15 ) ) ;
#59048 = CARTESIAN_POINT ( 'NONE',  ( 25.05000000000000071, 0.000000000000000000, 4.999999999999998224 ) ) ;
#59049 = CARTESIAN_POINT ( 'NONE',  ( 25.64999999999999858, -4.330127018922190985, -2.500000000000001332 ) ) ;
#59050 = CARTESIAN_POINT ( 'NONE',  ( 13.38750000000000107, -2.886751345948129988, 4.999999999999997335 ) ) ;
#59051 = CARTESIAN_POINT ( 'NONE',  ( -3.999999999999997335, 17.00000000122903288, 32.30940107675850470 ) ) ;
#59052 = CARTESIAN_POINT ( 'NONE',  ( 14.21250000122903323, 4.330127018922192761, -2.499999999999997780 ) ) ;
#59053 = CARTESIAN_POINT ( 'NONE',  ( 25.24687500061451573, 6.054752690667223547, 3.707466751127219781E-16 ) ) ;
#59054 = CARTESIAN_POINT ( 'NONE',  ( 15.72187500061451892, 3.027376345333613106, -5.243569643749998122 ) ) ;
#59055 = CARTESIAN_POINT ( 'NONE',  ( 25.10625000122903216, 0.000000000000000000, 4.999999999999998224 ) ) ;
#59056 = ORIENTED_EDGE ( 'NONE', *, *, #45249, .T. ) ;
#59057 = CARTESIAN_POINT ( 'NONE',  ( 19.60312500061451502, -4.541064518000417216, -2.621784821875001281 ) ) ;
#59058 = CARTESIAN_POINT ( 'NONE',  ( 5.353125000614515905, 4.541064518000418104, -2.621784821874998173 ) ) ;
#59059 = CARTESIAN_POINT ( 'NONE',  ( 17.29687500061451999, -3.027376345333614438, 5.243569643749998122 ) ) ;
#59060 = CARTESIAN_POINT ( 'NONE',  ( 29.03437500061451715, -4.541064518000419881, 2.621784821874995952 ) ) ;
#59061 = CARTESIAN_POINT ( 'NONE',  ( 5.390625000614518214, 6.054752690667223547, 3.707466751127219781E-16 ) ) ;
#59062 = CARTESIAN_POINT ( 'NONE',  ( 18.81562500061452070, 3.027376345333613106, -5.243569643749998122 ) ) ;
#59063 = CARTESIAN_POINT ( 'NONE',  ( 2.121784821874999061, 16.05312500061451786, 26.32496088578401583 ) ) ;
#59064 = CARTESIAN_POINT ( 'NONE',  ( 17.28750000122903430, 6.123233995736764310E-16, -4.999999999999998224 ) ) ;
#59065 = CARTESIAN_POINT ( 'NONE',  ( 12.27187500061451608, 2.746126346562643317, 4.756430356249998326 ) ) ;
#59066 = CARTESIAN_POINT ( 'NONE',  ( 8.090625000614515727, 6.054752690667223547, 3.707466751127219781E-16 ) ) ;
#59067 = CARTESIAN_POINT ( 'NONE',  ( 4.021875000614516082, 3.027376345333613106, -5.243569643749998122 ) ) ;
#59068 = CARTESIAN_POINT ( 'NONE',  ( 28.56562500061451715, -6.054752690667223547, -1.112240025338166033E-15 ) ) ;
#59069 = ADVANCED_FACE ( 'NONE', ( #51222 ), #34215, .F. ) ;
#59070 = CARTESIAN_POINT ( 'NONE',  ( 24.15937500061451715, -4.541064518000417216, -2.621784821875001281 ) ) ;
#59071 = CARTESIAN_POINT ( 'NONE',  ( 13.75312500061451715, -4.541064518000417216, -2.621784821875001281 ) ) ;
#59072 = CARTESIAN_POINT ( 'NONE',  ( 25.61250000122903359, 0.000000000000000000, 4.999999999999998224 ) ) ;
#59073 = CARTESIAN_POINT ( 'NONE',  ( 23.57812500061451289, -4.541064518000419881, 2.621784821874995952 ) ) ;
#59074 = CARTESIAN_POINT ( 'NONE',  ( 20.48437500061451289, -4.541064518000419881, 2.621784821874995952 ) ) ;
#59075 = CARTESIAN_POINT ( 'NONE',  ( 13.97812500061451679, 4.541064518000418104, 2.621784821874999949 ) ) ;
#59076 = CARTESIAN_POINT ( 'NONE',  ( -2.121784821874999949, 14.83437500061451786, 26.32496088578401938 ) ) ;
#59077 = CARTESIAN_POINT ( 'NONE',  ( 20.46562500061451928, -6.054752690667223547, -1.112240025338166033E-15 ) ) ;
#59078 = CARTESIAN_POINT ( 'NONE',  ( 29.61562500061451431, 3.027376345333613106, -5.243569643749998122 ) ) ;
#59079 = EDGE_LOOP ( 'NONE', ( #59903, #47025, #63569, #50213 ) ) ;
#59080 = ORIENTED_EDGE ( 'NONE', *, *, #9880, .T. ) ;
#59081 = CARTESIAN_POINT ( 'NONE',  ( 22.01249999999999574, -5.773502691896255534, -1.060575238724906372E-15 ) ) ;
#59082 = CARTESIAN_POINT ( 'NONE',  ( 4.000000000000000000, 10.28750000000000142, -27.69059892324149530 ) ) ;
#59083 = CARTESIAN_POINT ( 'NONE',  ( 14.86875000122903323, -5.773502691896255534, -1.060575238724906372E-15 ) ) ;
#59084 = CARTESIAN_POINT ( 'NONE',  ( 27.29062500061451502, -3.027376345333610441, -5.243569643749999898 ) ) ;
#59085 = CARTESIAN_POINT ( 'NONE',  ( 7.415625000614516793, -6.054752690667223547, -1.112240025338166033E-15 ) ) ;
#59086 = CARTESIAN_POINT ( 'NONE',  ( 20.28750000122903074, -4.330127018922194537, 2.499999999999995559 ) ) ;
#59087 = CARTESIAN_POINT ( 'NONE',  ( 24.85312500061451502, 0.000000000000000000, 5.243569643749999010 ) ) ;
#59088 = CARTESIAN_POINT ( 'NONE',  ( 25.05000000000000071, 0.000000000000000000, 4.999999999999998224 ) ) ;
#59089 = CARTESIAN_POINT ( 'NONE',  ( 27.02812500061451573, 4.541064518000418104, 2.621784821874999949 ) ) ;
#59090 = CARTESIAN_POINT ( 'NONE',  ( 8.090625000614515727, 6.054752690667223547, 3.707466751127219781E-16 ) ) ;
#59091 = ORIENTED_EDGE ( 'NONE', *, *, #57675, .F. ) ;
#59092 = B_SPLINE_CURVE_WITH_KNOTS ( 'NONE', 3,
 ( #63753, #69318, #7976, #57844, #47500, #13877, #36416, #24594, #13142, #68956 ),
 .UNSPECIFIED., .F., .F.,
 ( 4, 3, 3, 4 ),
 ( 8.113426134873485606E-18, 7.861467438249196448E-05, 0.0001572289795642654289, 0.0002817739516380214507 ),
 .UNSPECIFIED. ) ;
#59093 = CARTESIAN_POINT ( 'NONE',  ( 26.72812500061451502, -4.541064518000419881, 2.621784821874995952 ) ) ;
#59094 = CARTESIAN_POINT ( 'NONE',  ( 5.578125000614518214, -4.541064518000419881, 2.621784821874995952 ) ) ;
#59095 = CARTESIAN_POINT ( 'NONE',  ( 13.69687500061451679, -2.746126346562646425, 4.756430356249996549 ) ) ;
#59096 = CARTESIAN_POINT ( 'NONE',  ( 3.403125000614518836, -4.541064518000417216, -2.621784821875001281 ) ) ;
#59097 = CARTESIAN_POINT ( 'NONE',  ( 4.243569643749999898, 19.63437500061451857, -30.00000000000000000 ) ) ;
#59098 = CARTESIAN_POINT ( 'NONE',  ( 12.97499999999999964, -4.330127018922194537, 2.499999999999995559 ) ) ;
#59099 = CARTESIAN_POINT ( 'NONE',  ( 14.22187500061451537, -6.054752690667223547, -1.112240025338166033E-15 ) ) ;
#59100 = CARTESIAN_POINT ( 'NONE',  ( 8.700000001229032165, -2.886751345948125991, -5.000000000000000000 ) ) ;
#59101 = CARTESIAN_POINT ( 'NONE',  ( 13.77187500061451786, -6.054752690667223547, -1.112240025338166033E-15 ) ) ;
#59102 = CARTESIAN_POINT ( 'NONE',  ( 16.08749999999999503, -2.886751345948129988, 4.999999999999997335 ) ) ;
#59103 = CARTESIAN_POINT ( 'NONE',  ( 7.621875000614519280, 3.027376345333613106, -5.243569643749998122 ) ) ;
#59104 = CARTESIAN_POINT ( 'NONE',  ( 2.121784821875001281, 12.75312500061451715, -26.32496088578401938 ) ) ;
#59105 = CARTESIAN_POINT ( 'NONE',  ( 15.37500000000000000, 6.123233995736764310E-16, -4.999999999999998224 ) ) ;
#59106 = CARTESIAN_POINT ( 'NONE',  ( 13.13437500061451857, 4.541064518000418104, 2.621784821874999949 ) ) ;
#59107 = ORIENTED_EDGE ( 'NONE', *, *, #9276, .T. ) ;
#59108 = EDGE_CURVE ( 'NONE', #51352, #70677, #35848, .T. ) ;
#59109 = CARTESIAN_POINT ( 'NONE',  ( 21.14062500061451289, 6.054752690667223547, 3.707466751127219781E-16 ) ) ;
#59110 = CARTESIAN_POINT ( 'NONE',  ( 4.243569643749999010, 10.67187500061451644, 27.54997392385601174 ) ) ;
#59111 = DIRECTION ( 'NONE',  ( -0.000000000000000000, -1.000000000000000000, -0.000000000000000000 ) ) ;
#59112 = CARTESIAN_POINT ( 'NONE',  ( 26.18437500061451573, 4.541064518000418104, 2.621784821874999949 ) ) ;
#59113 = CARTESIAN_POINT ( 'NONE',  ( 27.87187500061451573, 3.027376345333613106, -5.243569643749998122 ) ) ;
#59114 = CARTESIAN_POINT ( 'NONE',  ( 4.790625000614518569, -3.027376345333610441, -5.243569643749999898 ) ) ;
#59115 = CARTESIAN_POINT ( 'NONE',  ( 22.09687500061451360, 0.000000000000000000, 4.756430356249998326 ) ) ;
#59116 = CARTESIAN_POINT ( 'NONE',  ( 17.07187500061451502, 3.027376345333613106, -5.243569643749998122 ) ) ;
#59117 = CARTESIAN_POINT ( 'NONE',  ( 7.771875000614516082, -4.119189519843968306, 2.378215178124996054 ) ) ;
#59118 = CARTESIAN_POINT ( 'NONE',  ( 29.06250000122903288, 4.330127018922192761, -2.499999999999997780 ) ) ;
#59119 = CARTESIAN_POINT ( 'NONE',  ( 6.346875000614517148, 6.054752690667223547, 3.707466751127219781E-16 ) ) ;
#59120 = CARTESIAN_POINT ( 'NONE',  ( 15.64687500061451608, -3.027376345333610441, -5.243569643749999898 ) ) ;
#59121 = CARTESIAN_POINT ( 'NONE',  ( 9.074999999999999289, 6.123233995736764310E-16, -4.999999999999998224 ) ) ;
#59122 = CARTESIAN_POINT ( 'NONE',  ( 25.80000000000000071, 4.330127018922192761, -2.499999999999997780 ) ) ;
#59123 = CARTESIAN_POINT ( 'NONE',  ( 26.67187500061451644, 3.027376345333611329, 5.243569643749999010 ) ) ;
#59124 = CARTESIAN_POINT ( 'NONE',  ( -3.756430356249999214, 12.94062499938548250, 27.83122392262697531 ) ) ;
#59125 = CARTESIAN_POINT ( 'NONE',  ( 10.12500000000000178, 4.330127018922191873, 2.499999999999999556 ) ) ;
#59126 = EDGE_LOOP ( 'NONE', ( #24389, #62179 ) ) ;
#59127 = CARTESIAN_POINT ( 'NONE',  ( 7.087499999999999467, -2.886751345948129988, 4.999999999999997335 ) ) ;
#59128 = CARTESIAN_POINT ( 'NONE',  ( 8.221875000614515372, -4.119189519843968306, 2.378215178124996054 ) ) ;
#59129 = CARTESIAN_POINT ( 'NONE',  ( 21.85312500061451502, -4.541064518000417216, -2.621784821875001281 ) ) ;
#59130 = CARTESIAN_POINT ( 'NONE',  ( 10.76250000000000107, -5.773502691896255534, -1.060575238724906372E-15 ) ) ;
#59131 = CARTESIAN_POINT ( 'NONE',  ( 7.462500001229035007, 4.330127018922192761, -2.499999999999997780 ) ) ;
#59132 = CARTESIAN_POINT ( 'NONE',  ( 6.440625000614517148, -3.027376345333614438, 5.243569643749998122 ) ) ;
#59133 = CARTESIAN_POINT ( 'NONE',  ( 21.82499999999999574, 4.330127018922191873, 2.499999999999999556 ) ) ;
#59134 = CARTESIAN_POINT ( 'NONE',  ( 19.60312500061451502, -4.541064518000417216, -2.621784821875001281 ) ) ;
#59135 = CARTESIAN_POINT ( 'NONE',  ( 0.000000000000000000, -4.999999999999998224, 0.000000000000000000 ) ) ;
#59136 = CARTESIAN_POINT ( 'NONE',  ( 26.40000000122902790, 5.773502691896255534, 3.535250795749688894E-16 ) ) ;
#59137 = CARTESIAN_POINT ( 'NONE',  ( -3.756430356250000990, 20.55312499938548143, 32.16877607737301048 ) ) ;
#59138 = CARTESIAN_POINT ( 'NONE',  ( 4.800000000000002487, 0.000000000000000000, 4.999999999999998224 ) ) ;
#59139 = ORIENTED_EDGE ( 'NONE', *, *, #51006, .F. ) ;
#59140 = CARTESIAN_POINT ( 'NONE',  ( 19.22812500061451502, 6.421520780324663323E-16, -5.243569643749999010 ) ) ;
#59141 = CARTESIAN_POINT ( 'NONE',  ( 27.21562500061451928, -6.054752690667223547, -1.112240025338166033E-15 ) ) ;
#59142 = CARTESIAN_POINT ( 'NONE',  ( 24.79687500061451999, 6.054752690667223547, 3.707466751127219781E-16 ) ) ;
#59143 = CARTESIAN_POINT ( 'NONE',  ( 8.962500000000002132, -5.773502691896255534, -1.060575238724906372E-15 ) ) ;
#59144 = CARTESIAN_POINT ( 'NONE',  ( 12.62812500061451537, 4.541064518000418104, 2.621784821874999949 ) ) ;
#59145 = CARTESIAN_POINT ( 'NONE',  ( 28.00312500061451715, 0.000000000000000000, 5.243569643749999010 ) ) ;
#59146 = CARTESIAN_POINT ( 'NONE',  ( 8.428125000614517859, 6.421520780324663323E-16, -5.243569643749999010 ) ) ;
#59147 = FACE_OUTER_BOUND ( 'NONE', #42570, .T. ) ;
#59148 = CARTESIAN_POINT ( 'NONE',  ( -2.121784821874996840, 12.28437500061451892, 33.67503911421598417 ) ) ;
#59149 = CARTESIAN_POINT ( 'NONE',  ( 24.90000000122903145, -2.886751345948125991, -5.000000000000000000 ) ) ;
#59150 = CARTESIAN_POINT ( 'NONE',  ( 18.75937500061451857, -4.119189519843965641, -2.378215178125001383 ) ) ;
#59151 = CARTESIAN_POINT ( 'NONE',  ( 13.41562500061451502, 3.027376345333612662, -5.243569643749998122 ) ) ;
#59152 =( GEOMETRIC_REPRESENTATION_CONTEXT ( 3 ) GLOBAL_UNCERTAINTY_ASSIGNED_CONTEXT ( ( #7051 ) ) GLOBAL_UNIT_ASSIGNED_CONTEXT ( ( #33832, #51556, #27940 ) ) REPRESENTATION_CONTEXT ( 'NONE', 'WORKASPACE' ) );
#59153 = CARTESIAN_POINT ( 'NONE',  ( 11.33437500061451608, 4.541064518000418104, 2.621784821874999949 ) ) ;
#59154 = CARTESIAN_POINT ( 'NONE',  ( 9.646875000614516082, -3.027376345333614438, 5.243569643749998122 ) ) ;
#59155 = CARTESIAN_POINT ( 'NONE',  ( 16.95937500061451786, -4.541064518000417216, -2.621784821875001281 ) ) ;
#59156 = VERTEX_POINT ( 'NONE', #5432 ) ;
#59157 = CARTESIAN_POINT ( 'NONE',  ( 29.70937500061451431, 4.541064518000418104, -2.621784821874998173 ) ) ;
#59158 = CARTESIAN_POINT ( 'NONE',  ( 21.55312500061451431, 4.541064518000418104, -2.621784821874998173 ) ) ;
#59159 = CARTESIAN_POINT ( 'NONE',  ( 17.67187500061451644, 3.027376345333611329, 5.243569643749999010 ) ) ;
#59160 = CARTESIAN_POINT ( 'NONE',  ( 20.91562500061451502, -6.054752690667223547, -1.112240025338166033E-15 ) ) ;
#59161 = CARTESIAN_POINT ( 'NONE',  ( 3.999999999999998668, 14.86250000000000071, 27.69059892324149175 ) ) ;
#59162 = CARTESIAN_POINT ( 'NONE',  ( 27.32812500061451644, 6.421520780324663323E-16, -5.243569643749999010 ) ) ;
#59163 = CARTESIAN_POINT ( 'NONE',  ( 7.087500001229034119, 4.330127018922191873, 2.499999999999999556 ) ) ;
#59164 = ORIENTED_EDGE ( 'NONE', *, *, #49176, .T. ) ;
#59165 = CARTESIAN_POINT ( 'NONE',  ( 3.862500001229035362, 4.330127018922192761, -2.499999999999997780 ) ) ;
#59166 = CARTESIAN_POINT ( 'NONE',  ( -3.999999999999997335, 18.23750000000000071, -27.69059892324149175 ) ) ;
#59167 = CARTESIAN_POINT ( 'NONE',  ( 23.66250000122903430, 4.330127018922192761, -2.499999999999997780 ) ) ;
#59168 = CARTESIAN_POINT ( 'NONE',  ( -1.878215178125001827, 14.85312499938548214, 33.25316411605952283 ) ) ;
#59169 = CARTESIAN_POINT ( 'NONE',  ( 7.134375000614516793, 6.421520780324663323E-16, -5.243569643749999010 ) ) ;
#59170 = FACE_OUTER_BOUND ( 'NONE', #61867, .T. ) ;
#59171 = CARTESIAN_POINT ( 'NONE',  ( 16.15312500061451573, 4.541064518000418104, -2.621784821874998173 ) ) ;
#59172 = CARTESIAN_POINT ( 'NONE',  ( 8.634375000614518569, 4.541064518000418104, 2.621784821874999949 ) ) ;
#59173 = CARTESIAN_POINT ( 'NONE',  ( 26.21250000122903501, -4.330127018922190985, -2.500000000000001332 ) ) ;
#59174 = CARTESIAN_POINT ( 'NONE',  ( 18.34687500061451715, -3.027376345333610441, -5.243569643749999898 ) ) ;
#59175 = CARTESIAN_POINT ( 'NONE',  ( 3.984375000614517326, 6.421520780324663323E-16, -5.243569643749999010 ) ) ;
#59176 = CARTESIAN_POINT ( 'NONE',  ( 5.803125000614517859, 4.541064518000418104, -2.621784821874998173 ) ) ;
#59177 = CARTESIAN_POINT ( 'NONE',  ( 14.54062500061451679, -3.027376345333614438, 5.243569643749998122 ) ) ;
#59178 = ORIENTED_EDGE ( 'NONE', *, *, #63830, .T. ) ;
#59179 = CARTESIAN_POINT ( 'NONE',  ( 13.22812500061451502, -4.541064518000419881, 2.621784821874995952 ) ) ;
#59180 = CARTESIAN_POINT ( 'NONE',  ( 5.662500001229035185, 4.330127018922192761, -2.499999999999997780 ) ) ;
#59181 = CARTESIAN_POINT ( 'NONE',  ( 9.853125000614516793, 4.541064518000418104, -2.621784821874998173 ) ) ;
#59182 = CARTESIAN_POINT ( 'NONE',  ( 21.57187500061451502, 2.746126346562645981, -4.756430356249997438 ) ) ;
#59183 = CARTESIAN_POINT ( 'NONE',  ( 11.88749999999999751, 5.773502691896255534, 3.535250795749688894E-16 ) ) ;
#59184 = CARTESIAN_POINT ( 'NONE',  ( 7.050000001229036251, 5.773502691896255534, 3.535250795749688894E-16 ) ) ;
#59185 = CARTESIAN_POINT ( 'NONE',  ( 19.91250000000000142, 2.886751345948129099, -4.999999999999998224 ) ) ;
#59186 = CARTESIAN_POINT ( 'NONE',  ( 16.09687500061452070, -3.027376345333610441, -5.243569643749999898 ) ) ;
#59187 = CARTESIAN_POINT ( 'NONE',  ( 16.31250000122903288, -4.330127018922190985, -2.500000000000001332 ) ) ;
#59188 = CARTESIAN_POINT ( 'NONE',  ( 22.68750000000000000, 5.773502691896255534, 3.535250795749688894E-16 ) ) ;
#59189 = CARTESIAN_POINT ( 'NONE',  ( 4.243569643749999010, 19.61562500061451431, -32.45002607614398471 ) ) ;
#59190 = CARTESIAN_POINT ( 'NONE',  ( 3.223068828554207066, 3.822549816615882445, 3.589315889418955408 ) ) ;
#59191 = CARTESIAN_POINT ( 'NONE',  ( -1.626862140677534273E-15, 15.93124999877096748, 34.00000000000000000 ) ) ;
#59192 = DIRECTION ( 'NONE',  ( 0.000000000000000000, 0.000000000000000000, 1.000000000000000000 ) ) ;
#59193 = CARTESIAN_POINT ( 'NONE',  ( 9.487500001229033586, -4.330127018922194537, 2.499999999999995559 ) ) ;
#59194 = CARTESIAN_POINT ( 'NONE',  ( 19.70625000122903359, 0.000000000000000000, 4.999999999999998224 ) ) ;
#59195 = CARTESIAN_POINT ( 'NONE',  ( 16.35937500061451644, 0.000000000000000000, 5.243569643749999010 ) ) ;
#59196 = EDGE_CURVE ( 'NONE', #13067, #72457, #45150, .T. ) ;
#59197 =( BOUNDED_CURVE ( )  B_SPLINE_CURVE ( 2, ( #49056, #4361, #9884, #71948, #21324, #43877, #65294, #38322, #15779, #31691, #60847, #37225, #15054, #10254, #37592, #54226, #2882, #48686, #71209, #20586, #43141, #60113, #61574, #55682, #34221, #27612, #28688, #67861, #62668, #4716, #21690, #16149, #50148, #49784, #5079, #72676, #27979, #67503, #39060, #22418, #22059, #56754, #68227, #10977, #61221, #264, #28328, #61943, #10615, #39792, #44246, #33145, #22774, #50866, #67147, #33498, #11347, #66777, #56047, #44617, #50509, #45325, #45693, #51227, #16507, #27250, #23138, #17590, #5439, #44965, #38701, #40149, #73035, #17232, #12063, #55322, #72308, #33864, #16867, #56407, #39422, #5798, #62309, #11705, #6159, #631, #13490, #57835, #34586, #52309, #18304, #63023, #58195, #40875, #34954, #36038, #6886, #7966, #47132, #41953, #57114, #13133, #63392, #46773, #1711, #7244, #19029, #57482, #995, #58558, #7598, #30502, #12777, #64105, #18670, #35313, #24947, #30137, #52668, #53030, #2424, #29773, #41232, #23502, #51595, #6526, #70021, #12422, #2075, #47491, #24224, #35672, #41587, #29058, #64473, #69309, #24584, #29419, #69663, #46050, #51952, #68585, #19392, #63744, #17946, #40508, #1352, #23861, #46409, #68946, #8329, #43047, #20126, #37865, #31226, #14963, #58921, #53397, #30859, #37128, #43784, #31961, #43422, #65944, #54499, #4270, #9792, #3163, #36408, #54862, #26794, #36768, #54137, #70390, #49328, #2790, #9433, #71860, #21232, #25315, #20491, #3900, #70751, #60021, #47861, #3532, #13867, #26054, #42681, #15324, #59657, #19766, #31600, #65204, #42317, #37501, #14593, #14230, #60384, #59285, #32325, #26421, #64843, #8694, #65573, #9066, #48594, #71119, #48962, #71492, #53768, #25692, #48227, #20869, #38974 ),
 .UNSPECIFIED., .F., .F. ) 
 B_SPLINE_CURVE_WITH_KNOTS ( ( 3, 2, 2, 2, 2, 2, 2, 2, 2, 2, 2, 2, 2, 2, 2, 2, 2, 2, 2, 2, 2, 2, 2, 2, 2, 2, 2, 2, 2, 2, 2, 2, 2, 2, 2, 2, 2, 2, 2, 2, 2, 2, 2, 2, 2, 2, 2, 2, 2, 2, 2, 2, 2, 2, 2, 2, 2, 2, 2, 2, 2, 2, 2, 2, 2, 2, 2, 2, 2, 2, 2, 2, 2, 2, 2, 2, 2, 2, 2, 2, 2, 2, 2, 2, 2, 2, 2, 2, 2, 2, 2, 2, 2, 2, 2, 2, 2, 2, 2, 2, 2, 2, 2, 2, 2, 2, 2, 3 ),
 ( 0.000000000000000000, 0.009375299918951271114, 0.01875059983790254223, 0.02812589975685381508, 0.03750119967580508445, 0.04687649959475635730, 0.05625179951370763015, 0.06562709943265890300, 0.07500239935161016891, 0.08437769927056144870, 0.09375299918951271461, 0.1031282991084639805, 0.1125035990274152603, 0.1218788989463665262, 0.1312541988653178060, 0.1406294987842690858, 0.1500047987032203378, 0.1593800986221716176, 0.1687553985411228974, 0.1781306984600741772, 0.1875059983790254292, 0.1968812982979767090, 0.2062565982169279610, 0.2156318981358792686, 0.2250071980548305206, 0.2343824979737818004, 0.2437577978927330524, 0.2531330978116843600, 0.2625083977306356120, 0.2718836976495869195, 0.2812589975685381716, 0.2906342974874894236, 0.3000095974064406756, 0.3093848973253919832, 0.3187601972443432352, 0.3281354971632944872, 0.3375107970822457948, 0.3468860970011971023, 0.3562613969201483544, 0.3656366968390996064, 0.3750119967580508584, 0.3843872966770021660, 0.3937625965959534180, 0.4031378965149046700, 0.4125131964338559221, 0.4218884963528072296, 0.4312637962717585371, 0.4406390961907097892, 0.4500143961096610412, 0.4593896960286123488, 0.4687649959475636008, 0.4781402958665148528, 0.4875155957854661049, 0.4968908957044174124, 0.5062661956233687199, 0.5156414955423199720, 0.5250167954612712240, 0.5343920953802224760, 0.5437673952991738391, 0.5531426952181249801, 0.5625179951370763431, 0.5718932950560274842, 0.5812685949749788472, 0.5906438948939302103, 0.6000191948128813513, 0.6093944947318327143, 0.6187697946507839664, 0.6281450945697352184, 0.6375203944886864704, 0.6468956944076377225, 0.6562709943265889745, 0.6656462942455403375, 0.6750215941644915896, 0.6843968940834428416, 0.6937721940023942047, 0.7031474939213453457, 0.7125227938402967087, 0.7218980937592478497, 0.7312733936781992128, 0.7406486935971504648, 0.7500239935161017168, 0.7593992934350529689, 0.7687745933540043319, 0.7781498932729555840, 0.7875251931919068360, 0.7969004931108581991, 0.8062757930298093401, 0.8156510929487607031, 0.8250263928677118441, 0.8344016927866632072, 0.8437769927056144592, 0.8531522926245657112, 0.8625275925435170743, 0.8719028924624683263, 0.8812781923814195784, 0.8906534923003708304, 0.9000287922193220824, 0.9094040921382733345, 0.9187793920572246975, 0.9281546919761758385, 0.9375299918951272016, 0.9469052918140784536, 0.9562805917330297056, 0.9656558916519810687, 0.9750311915709322097, 0.9844064914898835728, 0.9937817914088348248, 1.000000000000000000 ),
 .UNSPECIFIED. ) 
 CURVE ( )  GEOMETRIC_REPRESENTATION_ITEM ( )  RATIONAL_B_SPLINE_CURVE ( ( 1.000000000000000000, 0.8660254037844387076, 1.000000000000000000, 0.8660254037844387076, 1.000000000000000000, 0.8660254037844387076, 1.000000000000000000, 0.8660254037844387076, 1.000000000000000000, 0.8660254037844387076, 1.000000000000000000, 0.8660254037844387076, 1.000000000000000000, 0.8660254037844387076, 1.000000000000000000, 0.8660254037844387076, 1.000000000000000000, 0.8660254037844387076, 1.000000000000000000, 0.8660254037844387076, 1.000000000000000000, 0.8660254037844387076, 1.000000000000000000, 0.8660254037844387076, 1.000000000000000000, 0.8660254037844387076, 1.000000000000000000, 0.8660254037844387076, 1.000000000000000000, 0.8660254037844387076, 1.000000000000000000, 0.8660254037844387076, 1.000000000000000000, 0.8660254037844387076, 1.000000000000000000, 0.8660254037844387076, 1.000000000000000000, 0.8660254037844387076, 1.000000000000000000, 0.8660254037844387076, 1.000000000000000000, 0.8660254037844387076, 1.000000000000000000, 0.8660254037844387076, 1.000000000000000000, 0.8660254037844387076, 1.000000000000000000, 0.8660254037844387076, 1.000000000000000000, 0.8660254037844387076, 1.000000000000000000, 0.8660254037844387076, 1.000000000000000000, 0.8660254037844387076, 1.000000000000000000, 0.8660254037844387076, 1.000000000000000000, 0.8660254037844387076, 1.000000000000000000, 0.8660254037844387076, 1.000000000000000000, 0.8660254037844387076, 1.000000000000000000, 0.8660254037844387076, 1.000000000000000000, 0.8660254037844387076, 1.000000000000000000, 0.8660254037844387076, 1.000000000000000000, 0.8660254037844387076, 1.000000000000000000, 0.8660254037844387076, 1.000000000000000000, 0.8660254037844387076, 1.000000000000000000, 0.8660254037844387076, 1.000000000000000000, 0.8660254037844387076, 1.000000000000000000, 0.8660254037844387076, 1.000000000000000000, 0.8660254037844387076, 1.000000000000000000, 0.8660254037844387076, 1.000000000000000000, 0.8660254037844387076, 1.000000000000000000, 0.8660254037844387076, 1.000000000000000000, 0.8660254037844387076, 1.000000000000000000, 0.8660254037844387076, 1.000000000000000000, 0.8660254037844387076, 1.000000000000000000, 0.8660254037844387076, 1.000000000000000000, 0.8660254037844387076, 1.000000000000000000, 0.8660254037844387076, 1.000000000000000000, 0.8660254037844387076, 1.000000000000000000, 0.8660254037844387076, 1.000000000000000000, 0.8660254037844387076, 1.000000000000000000, 0.8660254037844387076, 1.000000000000000000, 0.8660254037844387076, 1.000000000000000000, 0.8660254037844387076, 1.000000000000000000, 0.8660254037844387076, 1.000000000000000000, 0.8660254037844387076, 1.000000000000000000, 0.8660254037844387076, 1.000000000000000000, 0.8660254037844387076, 1.000000000000000000, 0.8660254037844387076, 1.000000000000000000, 0.8660254037844387076, 1.000000000000000000, 0.8660254037844387076, 1.000000000000000000, 0.8660254037844387076, 1.000000000000000000, 0.8660254037844387076, 1.000000000000000000, 0.8660254037844387076, 1.000000000000000000, 0.8660254037844387076, 1.000000000000000000, 0.8660254037844387076, 1.000000000000000000, 0.8660254037844387076, 1.000000000000000000, 0.8660254037844387076, 1.000000000000000000, 0.8660254037844387076, 1.000000000000000000, 0.8660254037844387076, 1.000000000000000000, 0.8660254037844387076, 1.000000000000000000, 0.8660254037844387076, 1.000000000000000000, 0.8660254037844387076, 1.000000000000000000, 0.8660254037844387076, 1.000000000000000000, 0.8660254037844387076, 1.000000000000000000, 0.8660254037844387076, 1.000000000000000000, 0.8660254037844387076, 1.000000000000000000, 0.8660254037844387076, 1.000000000000000000, 0.8660254037844387076, 1.000000000000000000, 0.8660254037844387076, 1.000000000000000000, 0.8660254037844387076, 1.000000000000000000, 0.8660254037844387076, 1.000000000000000000, 0.8660254037844387076, 1.000000000000000000, 0.8660254037844387076, 1.000000000000000000, 0.8660254037844387076, 1.000000000000000000, 0.8660254037844387076, 1.000000000000000000, 0.8660254037844387076, 1.000000000000000000, 0.8660254037844387076, 1.000000000000000000, 0.8660254037844387076, 1.000000000000000000, 0.8660254037844387076, 1.000000000000000000, 0.8660254037844387076, 1.000000000000000000, 0.8660254037844387076, 1.000000000000000000, 0.8660254037844387076, 1.000000000000000000, 0.8660254037844387076, 1.000000000000000000, 0.8660254037844387076, 1.000000000000000000, 0.8660254037844387076, 1.000000000000000000, 0.8660254037844387076, 1.000000000000000000, 0.8660254037844387076, 1.000000000000000000, 0.8660254037844387076, 1.000000000000000000, 0.8660254037844387076, 1.000000000000000000, 0.8660254037844387076, 1.000000000000000000, 0.8660254037844387076, 1.000000000000000000, 0.8660254037844387076, 1.000000000000000000, 0.8660254037844387076, 1.000000000000000000, 0.9111407643075507545, 0.9401540804404022733 ) ) 
 REPRESENTATION_ITEM ( '' )  );
#59198 = CARTESIAN_POINT ( 'NONE',  ( 12.85312500061451502, -4.541064518000417216, -2.621784821875001281 ) ) ;
#59199 = AXIS2_PLACEMENT_3D ( 'NONE', #54284, #14741, #20275 ) ;
#59200 = CARTESIAN_POINT ( 'NONE',  ( 7.818750001229033408, 2.886751345948129099, -4.999999999999998224 ) ) ;
#59201 = CARTESIAN_POINT ( 'NONE',  ( 24.04687500061451644, -3.027376345333614438, 5.243569643749998122 ) ) ;
#59202 = CARTESIAN_POINT ( 'NONE',  ( 16.92187500061451644, 5.824947211148865298E-16, -4.756430356249998326 ) ) ;
#59203 = CARTESIAN_POINT ( 'NONE',  ( 10.79062500061451679, 6.054752690667223547, 3.707466751127219781E-16 ) ) ;
#59204 = CARTESIAN_POINT ( 'NONE',  ( 16.32187500061451502, 3.027376345333611329, 5.243569643749999010 ) ) ;
#59205 = ORIENTED_EDGE ( 'NONE', *, *, #21176, .T. ) ;
#59206 = CARTESIAN_POINT ( 'NONE',  ( 24.12187500061451217, -6.054752690667223547, -1.112240025338166033E-15 ) ) ;
#59207 = CARTESIAN_POINT ( 'NONE',  ( 25.11562500061451431, 3.027376345333613106, -5.243569643749998122 ) ) ;
#59208 = CARTESIAN_POINT ( 'NONE',  ( 27.25312500061451360, -4.541064518000417216, -2.621784821875001281 ) ) ;
#59209 = CARTESIAN_POINT ( 'NONE',  ( 30.00000000000000000, 0.000000000000000000, 4.999999999999998224 ) ) ;
#59210 = CARTESIAN_POINT ( 'NONE',  ( 7.350000000000002309, 4.330127018922192761, -2.499999999999997780 ) ) ;
#59211 = CARTESIAN_POINT ( 'NONE',  ( 18.00000000122903288, -2.886751345948129988, 4.999999999999997335 ) ) ;
#59212 = CARTESIAN_POINT ( 'NONE',  ( 16.66875000122903216, -5.773502691896255534, -1.060575238724906372E-15 ) ) ;
#59213 = CARTESIAN_POINT ( 'NONE',  ( 7.246875000614514839, 0.000000000000000000, 4.756430356249998326 ) ) ;
#59214 = VERTEX_POINT ( 'NONE', #7237 ) ;
#59215 = CARTESIAN_POINT ( 'NONE',  ( 16.01249999999999929, 2.886751345948126879, 4.999999999999999112 ) ) ;
#59216 = CARTESIAN_POINT ( 'NONE',  ( 19.16250000000000142, 2.886751345948126879, 4.999999999999999112 ) ) ;
#59217 = CARTESIAN_POINT ( 'NONE',  ( 13.37812500061451715, 6.421520780324663323E-16, -5.243569643749999010 ) ) ;
#59218 = VERTEX_POINT ( 'NONE', #64097 ) ;
#59219 = CARTESIAN_POINT ( 'NONE',  ( 4.000000000000000000, 18.50000000122903288, -27.69059892324149885 ) ) ;
#59220 = CARTESIAN_POINT ( 'NONE',  ( -2.121784821874996840, 15.88437500061451857, -26.32496088578401583 ) ) ;
#59221 = CARTESIAN_POINT ( 'NONE',  ( 5.653125000614517504, -4.541064518000417216, -2.621784821875001281 ) ) ;
#59222 = CARTESIAN_POINT ( 'NONE',  ( 0.000000000000000000, 4.999999999999998224, 0.000000000000000000 ) ) ;
#59223 = CARTESIAN_POINT ( 'NONE',  ( 11.10000000000000142, 0.000000000000000000, 4.999999999999998224 ) ) ;
#59224 = CARTESIAN_POINT ( 'NONE',  ( 28.43437500061451573, -2.746126346562646425, 4.756430356249996549 ) ) ;
#59225 = ORIENTED_EDGE ( 'NONE', *, *, #25685, .T. ) ;
#59226 = CARTESIAN_POINT ( 'NONE',  ( 4.243569643749999898, 15.07812500061451644, 30.00000000000000000 ) ) ;
#59227 = CARTESIAN_POINT ( 'NONE',  ( 26.54062500061451146, 6.054752690667223547, 3.707466751127219781E-16 ) ) ;
#59228 = FACE_OUTER_BOUND ( 'NONE', #30447, .T. ) ;
#59229 = CARTESIAN_POINT ( 'NONE',  ( -7.967954043666661671E-16, 18.37812499938548427, 34.33755215474603517 ) ) ;
#59230 = CARTESIAN_POINT ( 'NONE',  ( 24.38437500061451502, 4.541064518000418104, 2.621784821874999949 ) ) ;
#59231 = CARTESIAN_POINT ( 'NONE',  ( 18.21562500061451573, -6.054752690667223547, -1.112240025338166033E-15 ) ) ;
#59232 = CARTESIAN_POINT ( 'NONE',  ( 4.243569643749999010, 14.66562500061459495, -32.45002607614398471 ) ) ;
#59233 = CARTESIAN_POINT ( 'NONE',  ( 23.88750000122903216, -4.330127018922194537, 2.499999999999995559 ) ) ;
#59234 = CARTESIAN_POINT ( 'NONE',  ( 6.628125000614517148, 6.421520780324663323E-16, -5.243569643749999010 ) ) ;
#59235 = CARTESIAN_POINT ( 'NONE',  ( 27.64687500061452141, -2.746126346562646425, 4.756430356249996549 ) ) ;
#59236 = CARTESIAN_POINT ( 'NONE',  ( 22.07812500061451644, 4.541064518000418104, 2.621784821874999949 ) ) ;
#59237 = CARTESIAN_POINT ( 'NONE',  ( 9.871875000614517504, 2.746126346562645981, -4.756430356249997438 ) ) ;
#59238 = CARTESIAN_POINT ( 'NONE',  ( -3.756430356250001434, 16.05312499938548143, 32.16877607737301048 ) ) ;
#59239 = CARTESIAN_POINT ( 'NONE',  ( 16.28437500061452070, 4.541064518000418104, 2.621784821874999949 ) ) ;
#59240 = CARTESIAN_POINT ( 'NONE',  ( 25.09687500061451715, -3.027376345333610441, -5.243569643749999898 ) ) ;
#59241 = CARTESIAN_POINT ( 'NONE',  ( -2.121784821874996840, 13.18437500061451750, 33.67503911421598417 ) ) ;
#59242 = CARTESIAN_POINT ( 'NONE',  ( 4.640625000614518214, -3.027376345333614438, 5.243569643749998122 ) ) ;
#59243 = CARTESIAN_POINT ( 'NONE',  ( 28.75312500061451715, 4.541064518000418104, -2.621784821874998173 ) ) ;
#59244 = EDGE_CURVE ( 'NONE', #45117, #10316, #12133, .T. ) ;
#59245 = CARTESIAN_POINT ( 'NONE',  ( 28.94062500061452070, -3.027376345333614438, 5.243569643749998122 ) ) ;
#59246 = CARTESIAN_POINT ( 'NONE',  ( -1.071796769724489229, 13.71740381056766722, 34.00000000000000000 ) ) ;
#59247 = CARTESIAN_POINT ( 'NONE',  ( 0.000000000000000000, 20.00000000000000000, -30.00000000000000000 ) ) ;
#59248 = CARTESIAN_POINT ( 'NONE',  ( 29.25000000122903288, -2.886751345948129988, 4.999999999999997335 ) ) ;
#59249 = CARTESIAN_POINT ( 'NONE',  ( 7.434375000614519280, -4.541064518000419881, 2.621784821874995952 ) ) ;
#59250 = CARTESIAN_POINT ( 'NONE',  ( 15.48750000122903359, 6.123233995736764310E-16, -4.999999999999998224 ) ) ;
#59251 = CARTESIAN_POINT ( 'NONE',  ( 29.61562500061451431, 3.027376345333613106, -5.243569643749998122 ) ) ;
#59252 = CARTESIAN_POINT ( 'NONE',  ( 10.76250000122903572, 0.000000000000000000, 4.999999999999998224 ) ) ;
#59253 = CARTESIAN_POINT ( 'NONE',  ( 4.228125000614517681, -4.541064518000419881, 2.621784821874995952 ) ) ;
#59254 = CARTESIAN_POINT ( 'NONE',  ( -4.000000000000000000, 14.01874999877096606, 30.00000000000000000 ) ) ;
#59255 = CARTESIAN_POINT ( 'NONE',  ( 20.23125000122902861, -4.330127018922194537, 2.499999999999995559 ) ) ;
#59256 = CARTESIAN_POINT ( 'NONE',  ( 15.04687500061451644, -3.027376345333614438, 5.243569643749998122 ) ) ;
#59257 = ORIENTED_EDGE ( 'NONE', *, *, #10249, .F. ) ;
#59258 = CARTESIAN_POINT ( 'NONE',  ( 22.82812500061451644, 6.421520780324663323E-16, -5.243569643749999010 ) ) ;
#59259 = CARTESIAN_POINT ( 'NONE',  ( 7.678125000614516082, 4.541064518000418104, 2.621784821874999949 ) ) ;
#59260 = CARTESIAN_POINT ( 'NONE',  ( 24.12187500061451573, -6.054752690667223547, -1.112240025338166033E-15 ) ) ;
#59261 = CARTESIAN_POINT ( 'NONE',  ( 8.240625000614516082, -3.027376345333614438, 5.243569643749998122 ) ) ;
#59262 = CARTESIAN_POINT ( 'NONE',  ( 30.00000000000000000, 0.000000000000000000, 0.000000000000000000 ) ) ;
#59263 = CARTESIAN_POINT ( 'NONE',  ( 8.437500001229034652, 4.330127018922191873, 2.499999999999999556 ) ) ;
#59264 = CARTESIAN_POINT ( 'NONE',  ( 24.59062500061451573, -3.027376345333610441, -5.243569643749999898 ) ) ;
#59265 = AXIS2_PLACEMENT_3D ( 'NONE', #22696, #56682, #72230 ) ;
#59266 = CARTESIAN_POINT ( 'NONE',  ( 1.999999999999998668, 19.51250000122903216, -33.46410161513775705 ) ) ;
#59267 = CARTESIAN_POINT ( 'NONE',  ( 11.13750000122903216, 4.330127018922191873, 2.499999999999999556 ) ) ;
#59268 = CARTESIAN_POINT ( 'NONE',  ( 20.39062500061451644, -3.027376345333614438, 5.243569643749998122 ) ) ;
#59269 = CARTESIAN_POINT ( 'NONE',  ( 18.32812500061451644, 6.421520780324663323E-16, -5.243569643749999010 ) ) ;
#59270 = CARTESIAN_POINT ( 'NONE',  ( 27.87187500061451573, 2.746126346562645981, -4.756430356249997438 ) ) ;
#59271 = CARTESIAN_POINT ( 'NONE',  ( 17.43750000000000355, -2.886751345948129988, 4.999999999999997335 ) ) ;
#59272 = CARTESIAN_POINT ( 'NONE',  ( 14.28750000122903430, 4.330127018922191873, 2.499999999999999556 ) ) ;
#59273 = CARTESIAN_POINT ( 'NONE',  ( 9.590625000614517504, -3.027376345333614438, 5.243569643749998122 ) ) ;
#59274 = CARTESIAN_POINT ( 'NONE',  ( 13.45312500061451466, 4.541064518000418104, -2.621784821874998173 ) ) ;
#59275 = CARTESIAN_POINT ( 'NONE',  ( 22.80000000122903359, 5.773502691896255534, 3.535250795749688894E-16 ) ) ;
#59276 = CARTESIAN_POINT ( 'NONE',  ( 22.99687500061451573, 6.054752690667223547, 3.707466751127219781E-16 ) ) ;
#59277 = CARTESIAN_POINT ( 'NONE',  ( 21.79687500061451644, -3.027376345333614438, 5.243569643749998122 ) ) ;
#59278 = CARTESIAN_POINT ( 'NONE',  ( 7.481250001229032165, 4.330127018922191873, 2.499999999999999556 ) ) ;
#59279 = CARTESIAN_POINT ( 'NONE',  ( 7.312500001229033764, -4.330127018922190985, -2.500000000000001332 ) ) ;
#59280 = CARTESIAN_POINT ( 'NONE',  ( 7.021875000614518747, -6.054752690667223547, -1.112240025338166033E-15 ) ) ;
#59281 = CARTESIAN_POINT ( 'NONE',  ( 23.18437500061451573, -4.541064518000419881, 2.621784821874995952 ) ) ;
#59282 = CARTESIAN_POINT ( 'NONE',  ( 10.57500000000000107, 4.330127018922191873, 2.499999999999999556 ) ) ;
#59283 = CARTESIAN_POINT ( 'NONE',  ( 18.74062500061451431, -3.027376345333610441, -5.243569643749999898 ) ) ;
#59284 = CARTESIAN_POINT ( 'NONE',  ( 24.08437500061451786, -4.541064518000419881, 2.621784821874995952 ) ) ;
#59285 = CARTESIAN_POINT ( 'NONE',  ( -3.756430356250000990, 20.21562499938548285, 32.16877607737301048 ) ) ;
#59286 = CARTESIAN_POINT ( 'NONE',  ( 23.09999999999999787, 4.330127018922192761, -2.499999999999997780 ) ) ;
#59287 = DIRECTION ( 'NONE',  ( -1.000000000000000000, -0.000000000000000000, -0.000000000000000000 ) ) ;
#59288 = CARTESIAN_POINT ( 'NONE',  ( 5.634375000614519458, -4.541064518000419881, 2.621784821874995952 ) ) ;
#59289 = CARTESIAN_POINT ( 'NONE',  ( 17.46562500061451217, 3.027376345333613106, -5.243569643749998122 ) ) ;
#59290 = EDGE_LOOP ( 'NONE', ( #42607, #34711, #27636, #45621 ) ) ;
#59291 = CARTESIAN_POINT ( 'NONE',  ( 24.55312500061451786, -4.541064518000417216, -2.621784821875001281 ) ) ;
#59292 = CARTESIAN_POINT ( 'NONE',  ( 3.430292791878407410, 3.637806684167773863, -3.517583096594174119 ) ) ;
#59293 = CYLINDRICAL_SURFACE ( 'NONE', #61983, 4.999999999999998224 ) ;
#59294 = CARTESIAN_POINT ( 'NONE',  ( 15.71250000000000213, -5.773502691896255534, -1.060575238724906372E-15 ) ) ;
#59295 = CARTESIAN_POINT ( 'NONE',  ( 27.60000000122903430, -2.886751345948125991, -5.000000000000000000 ) ) ;
#59296 = CARTESIAN_POINT ( 'NONE',  ( 21.62812500061451360, 4.541064518000418104, 2.621784821874999949 ) ) ;
#59297 = ORIENTED_EDGE ( 'NONE', *, *, #61121, .F. ) ;
#59298 = CARTESIAN_POINT ( 'NONE',  ( 22.27499999999999858, 4.330127018922191873, 2.499999999999999556 ) ) ;
#59299 = CARTESIAN_POINT ( 'NONE',  ( 22.77187500061451786, -6.054752690667223547, -1.112240025338166033E-15 ) ) ;
#59300 = VERTEX_POINT ( 'NONE', #35665 ) ;
#59301 = CARTESIAN_POINT ( 'NONE',  ( 13.42500000122903536, 2.886751345948126879, 4.999999999999998224 ) ) ;
#59302 = CARTESIAN_POINT ( 'NONE',  ( 13.22812500061451502, -4.541064518000419881, 2.621784821874995952 ) ) ;
#59303 = CARTESIAN_POINT ( 'NONE',  ( 3.478125000614517237, 6.421520780324663323E-16, -5.243569643749999010 ) ) ;
#59304 = CARTESIAN_POINT ( 'NONE',  ( 17.44687500061451502, 4.119189519843966529, -2.378215178124998275 ) ) ;
#59305 = CARTESIAN_POINT ( 'NONE',  ( 27.89062500061451289, 6.054752690667223547, 3.707466751127219781E-16 ) ) ;
#59306 = CARTESIAN_POINT ( 'NONE',  ( 13.27500000122903323, 2.886751345948129099, -4.999999999999998224 ) ) ;
#59307 = CARTESIAN_POINT ( 'NONE',  ( 20.24999999999999645, -4.330127018922190985, -2.500000000000001332 ) ) ;
#59308 = CARTESIAN_POINT ( 'NONE',  ( 26.02499999999999858, -4.330127018922194537, 2.499999999999995559 ) ) ;
#59309 = CARTESIAN_POINT ( 'NONE',  ( 34.99999999999999289, 2.500000000000000444, 3.499999999999999112 ) ) ;
#59310 = CARTESIAN_POINT ( 'NONE',  ( 8.034375000614518925, 6.421520780324663323E-16, -5.243569643749999010 ) ) ;
#59311 = CARTESIAN_POINT ( 'NONE',  ( 16.99687500061451573, -3.027376345333610441, -5.243569643749999898 ) ) ;
#59312 = CARTESIAN_POINT ( 'NONE',  ( -1.071796769724491005, 13.72009619066136921, 26.00000000000000355 ) ) ;
#59313 = ORIENTED_EDGE ( 'NONE', *, *, #64489, .T. ) ;
#59314 = CARTESIAN_POINT ( 'NONE',  ( 28.56562500061451715, -6.054752690667223547, -1.112240025338166033E-15 ) ) ;
#59315 = CARTESIAN_POINT ( 'NONE',  ( 3.525000000000000355, -4.330127018922194537, 2.499999999999995559 ) ) ;
#59316 = CARTESIAN_POINT ( 'NONE',  ( 4.898587196589412829E-16, 27.50000000000000000, 34.00000000000000000 ) ) ;
#59317 = CARTESIAN_POINT ( 'NONE',  ( 17.02499999999999858, -4.330127018922194537, 2.499999999999995559 ) ) ;
#59318 = CARTESIAN_POINT ( 'NONE',  ( 12.59062500061451573, 6.054752690667223547, 3.707466751127219781E-16 ) ) ;
#59319 = CARTESIAN_POINT ( 'NONE',  ( -5.810221930991193690E-16, 11.45000000122903216, 26.00000000000000355 ) ) ;
#59320 = CARTESIAN_POINT ( 'NONE',  ( 4.064219793244338241, -3.782806921759631624, -3.447986216289088635 ) ) ;
#59321 = CARTESIAN_POINT ( 'NONE',  ( 19.42500000122903714, -5.773502691896255534, -1.060575238724906372E-15 ) ) ;
#59322 = CARTESIAN_POINT ( 'NONE',  ( 3.752440054025286909, -3.304420318444254878, 4.071342403668507082 ) ) ;
#59323 = CARTESIAN_POINT ( 'NONE',  ( 17.03437500061451715, 5.824947211148865298E-16, -4.756430356249998326 ) ) ;
#59324 = CARTESIAN_POINT ( 'NONE',  ( 7.865625000614516971, -6.054752690667223547, -1.112240025338166033E-15 ) ) ;
#59325 = CARTESIAN_POINT ( 'NONE',  ( 23.78437500061451360, 6.421520780324663323E-16, -5.243569643749999010 ) ) ;
#59326 = CARTESIAN_POINT ( 'NONE',  ( -2.121784821874996840, 16.78437500061452070, 33.67503911421598417 ) ) ;
#59327 = CARTESIAN_POINT ( 'NONE',  ( 24.42187500061451999, 3.027376345333611329, 5.243569643749999010 ) ) ;
#59328 = CARTESIAN_POINT ( 'NONE',  ( 5.850000000000001421, -4.330127018922190985, -2.500000000000001332 ) ) ;
#59329 = CARTESIAN_POINT ( 'NONE',  ( 8.484601909799253346E-16, 10.32500000122903572, 34.61880215351700230 ) ) ;
#59330 = CARTESIAN_POINT ( 'NONE',  ( 13.00312500061451537, 4.541064518000418104, -2.621784821874998173 ) ) ;
#59331 = CARTESIAN_POINT ( 'NONE',  ( 3.862500001229035362, 4.330127018922192761, -2.499999999999997780 ) ) ;
#59332 = ADVANCED_FACE ( 'NONE', ( #2068 ), #47123, .T. ) ;
#59333 = CARTESIAN_POINT ( 'NONE',  ( 8.821875000614518569, -6.054752690667223547, -1.112240025338166033E-15 ) ) ;
#59334 = DIRECTION ( 'NONE',  ( 1.000000000000000000, -0.000000000000000000, -0.000000000000000000 ) ) ;
#59335 = ORIENTED_EDGE ( 'NONE', *, *, #27670, .F. ) ;
#59336 = CARTESIAN_POINT ( 'NONE',  ( 10.82812500061451644, 4.541064518000418104, 2.621784821874999949 ) ) ;
#59337 = CARTESIAN_POINT ( 'NONE',  ( 13.84687500061451537, -3.027376345333610441, -5.243569643749999898 ) ) ;
#59338 = CARTESIAN_POINT ( 'NONE',  ( 3.999999999999998668, 19.60624999877096641, 32.30940107675850470 ) ) ;
#59339 = CARTESIAN_POINT ( 'NONE',  ( 23.92500000122903359, -5.773502691896255534, -1.060575238724906372E-15 ) ) ;
#59340 = CARTESIAN_POINT ( 'NONE',  ( 10.92187500061451644, 3.027376345333611329, 5.243569643749999010 ) ) ;
#59341 = CARTESIAN_POINT ( 'NONE',  ( 13.07812500061451821, 4.541064518000418104, 2.621784821874999949 ) ) ;
#59342 = CARTESIAN_POINT ( 'NONE',  ( 27.65625000122902932, 4.330127018922192761, -2.499999999999997780 ) ) ;
#59343 = CARTESIAN_POINT ( 'NONE',  ( 22.20937500061451431, 0.000000000000000000, 5.243569643749999010 ) ) ;
#59344 = CARTESIAN_POINT ( 'NONE',  ( 45.00000000000000000, 0.000000000000000000, 4.999999999999998224 ) ) ;
#59345 = CARTESIAN_POINT ( 'NONE',  ( 4.387500001229033053, 4.330127018922191873, 2.499999999999999556 ) ) ;
#59346 = CARTESIAN_POINT ( 'NONE',  ( 13.68750000122903288, 6.123233995736764310E-16, -4.999999999999998224 ) ) ;
#59347 = CARTESIAN_POINT ( 'NONE',  ( -4.243569643749999898, 15.32187500061451502, -32.45002607614398471 ) ) ;
#59348 = CARTESIAN_POINT ( 'NONE',  ( 15.42187500061451821, 3.027376345333611329, 5.243569643749999010 ) ) ;
#59349 = CARTESIAN_POINT ( 'NONE',  ( 18.82500000122903216, 2.886751345948126879, 4.999999999999999112 ) ) ;
#59350 = CARTESIAN_POINT ( 'NONE',  ( 11.10937500061451644, -4.541064518000417216, -2.621784821875001281 ) ) ;
#59351 = CARTESIAN_POINT ( 'NONE',  ( -2.121784821874999949, 18.37812500061451715, -33.67503911421598417 ) ) ;
#59352 = CARTESIAN_POINT ( 'NONE',  ( 18.07500000122903216, -5.773502691896255534, -1.060575238724906372E-15 ) ) ;
#59353 = CARTESIAN_POINT ( 'NONE',  ( 13.79062500061451502, -3.027376345333610441, -5.243569643749999898 ) ) ;
#59354 = VERTEX_POINT ( 'NONE', #69655 ) ;
#59355 = CARTESIAN_POINT ( 'NONE',  ( 15.63749999999999751, -2.886751345948129988, 4.999999999999997335 ) ) ;
#59356 = CARTESIAN_POINT ( 'NONE',  ( 4.642109779777202405, 1.860292132678681210, -4.642109779777202405 ) ) ;
#59357 = CARTESIAN_POINT ( 'NONE',  ( 9.384375000614518569, 6.421520780324663323E-16, -5.243569643749999010 ) ) ;
#59358 = CARTESIAN_POINT ( 'NONE',  ( 3.089506346739232967, 3.931278485869285522, -3.469880700456108968 ) ) ;
#59359 = CARTESIAN_POINT ( 'NONE',  ( 13.57500000122903572, -5.773502691896255534, -1.060575238724906372E-15 ) ) ;
#59360 = CARTESIAN_POINT ( 'NONE',  ( 21.56250000122903288, 0.000000000000000000, 4.999999999999998224 ) ) ;
#59361 = CARTESIAN_POINT ( 'NONE',  ( 17.24062500061451786, -3.027376345333614438, 5.243569643749998122 ) ) ;
#59362 =( BOUNDED_CURVE ( )  B_SPLINE_CURVE ( 2, ( #31252, #3925, #37526, #13892, #9090, #53425, #43074, #70417, #42344 ),
 .UNSPECIFIED., .F., .F. ) 
 B_SPLINE_CURVE_WITH_KNOTS ( ( 3, 2, 2, 2, 3 ),
 ( 0.1527777777777777901, 0.1574074074074074125, 0.1666666666666666574, 0.1759259259259259300, 0.1805555555555555525 ),
 .UNSPECIFIED. ) 
 CURVE ( )  GEOMETRIC_REPRESENTATION_ITEM ( )  RATIONAL_B_SPLINE_CURVE ( ( 0.9330127018922194093, 0.9330127018922195203, 1.000000000000000000, 0.8660254037844387076, 1.000000000000000000, 0.8660254037844387076, 1.000000000000000000, 0.9330127018922194093, 0.9330127018922194093 ) ) 
 REPRESENTATION_ITEM ( '' )  );
#59363 = CARTESIAN_POINT ( 'NONE',  ( 21.36562500061451431, -6.054752690667223547, -1.112240025338166033E-15 ) ) ;
#59364 = CARTESIAN_POINT ( 'NONE',  ( 26.88750000122903216, 4.330127018922191873, 2.499999999999999556 ) ) ;
#59365 = CARTESIAN_POINT ( 'NONE',  ( 24.97499999999999787, 4.330127018922191873, 2.499999999999999556 ) ) ;
#59366 = CARTESIAN_POINT ( 'NONE',  ( 28.31249999999999645, -5.773502691896255534, -1.060575238724906372E-15 ) ) ;
#59367 = CARTESIAN_POINT ( 'NONE',  ( 28.42499999999999716, 6.123233995736764310E-16, -4.999999999999998224 ) ) ;
#59368 = CARTESIAN_POINT ( 'NONE',  ( 27.79687500061451999, -3.027376345333610441, -5.243569643749999898 ) ) ;
#59369 = CARTESIAN_POINT ( 'NONE',  ( 11.55000000000000071, 0.000000000000000000, 4.999999999999998224 ) ) ;
#59370 = CARTESIAN_POINT ( 'NONE',  ( -4.243569643749999898, 13.55937500061451750, -30.00000000000000000 ) ) ;
#59371 = CARTESIAN_POINT ( 'NONE',  ( 3.862500001229035362, 4.330127018922192761, -2.499999999999997780 ) ) ;
#59372 = CARTESIAN_POINT ( 'NONE',  ( 4.387500000000002842, -2.886751345948129988, 4.999999999999997335 ) ) ;
#59373 = EDGE_CURVE ( 'NONE', #15563, #46535, #19019, .T. ) ;
#59374 = CARTESIAN_POINT ( 'NONE',  ( 16.50000000000000000, 0.000000000000000000, 4.999999999999998224 ) ) ;
#59375 = CARTESIAN_POINT ( 'NONE',  ( 8.484375000614518214, 6.421520780324663323E-16, -5.243569643749999010 ) ) ;
#59376 = CARTESIAN_POINT ( 'NONE',  ( 26.24062500061451431, -3.027376345333614438, 5.243569643749998122 ) ) ;
#59378 = ADVANCED_FACE ( 'NONE', ( #46766 ), #58547, .F. ) ;
#59377 = FACE_OUTER_BOUND ( 'NONE', #12388, .T. ) ;
#59379 = CARTESIAN_POINT ( 'NONE',  ( 22.38749999999999574, -2.886751345948102898, 5.000000000000044409 ) ) ;
#59380 = CARTESIAN_POINT ( 'NONE',  ( 8.212500000000000355, 2.886751345948129099, -4.999999999999997335 ) ) ;
#59381 = CARTESIAN_POINT ( 'NONE',  ( 4.696875000614518569, -3.027376345333614438, 5.243569643749998122 ) ) ;
#59382 = CARTESIAN_POINT ( 'NONE',  ( 8.859375000614518214, -4.541064518000417216, -2.621784821875001281 ) ) ;
#59383 = CARTESIAN_POINT ( 'NONE',  ( 5.137500000000000178, 5.773502691896255534, 3.535250795749688894E-16 ) ) ;
#59384 = CARTESIAN_POINT ( 'NONE',  ( 4.243569643749999010, 12.86562500061459247, 27.54997392385601174 ) ) ;
#59386 = EDGE_CURVE ( 'NONE', #71135, #5961, #18663, .T. ) ;
#59385 = CARTESIAN_POINT ( 'NONE',  ( 28.57499999999999929, 4.330127018922191873, 2.499999999999999556 ) ) ;
#59387 = CARTESIAN_POINT ( 'NONE',  ( 3.262500000000001510, 2.886751345948129099, -4.999999999999998224 ) ) ;
#59388 = CARTESIAN_POINT ( 'NONE',  ( 15.79687500061451644, 0.000000000000000000, 4.756430356249998326 ) ) ;
#59389 = CARTESIAN_POINT ( 'NONE',  ( 21.10312500061451502, 4.541064518000418104, -2.621784821874998173 ) ) ;
#59390 = CARTESIAN_POINT ( 'NONE',  ( 10.64062500061451644, -3.027376345333610441, -5.243569643749999898 ) ) ;
#59391 = CARTESIAN_POINT ( 'NONE',  ( 23.29687500061451644, 4.119189519843966529, -2.378215178124998275 ) ) ;
#59392 = CARTESIAN_POINT ( 'NONE',  ( 9.309375000614517504, -4.541064518000417216, -2.621784821875001281 ) ) ;
#59393 = CARTESIAN_POINT ( 'NONE',  ( 26.62500000000000000, 6.123233995736764310E-16, -4.999999999999998224 ) ) ;
#59394 = CARTESIAN_POINT ( 'NONE',  ( 20.17500000122903359, 2.886751345948126879, 4.999999999999999112 ) ) ;
#59395 = CARTESIAN_POINT ( 'NONE',  ( 27.44062500061451715, 6.054752690667223547, 3.707466751127219781E-16 ) ) ;
#59396 = FACE_OUTER_BOUND ( 'NONE', #24154, .T. ) ;
#59397 = CARTESIAN_POINT ( 'NONE',  ( 8.446875000614518569, -3.027376345333610441, -5.243569643749999898 ) ) ;
#59398 = CARTESIAN_POINT ( 'NONE',  ( 14.67187500061451821, -6.054752690667223547, -1.112240025338166033E-15 ) ) ;
#59399 = CARTESIAN_POINT ( 'NONE',  ( 26.18437500061451573, 4.541064518000418104, 2.621784821874999949 ) ) ;
#59400 = ADVANCED_FACE ( 'NONE', ( #987 ), #68938, .T. ) ;
#59401 = CARTESIAN_POINT ( 'NONE',  ( 23.56875000122903074, 2.886751345948101122, -5.000000000000046185 ) ) ;
#59402 = CARTESIAN_POINT ( 'NONE',  ( 13.42499999999999893, -4.330127018922194537, 2.499999999999995559 ) ) ;
#59403 = CARTESIAN_POINT ( 'NONE',  ( 21.04687500061451644, -3.027376345333610441, -5.243569643749999898 ) ) ;
#59404 =( BOUNDED_CURVE ( )  B_SPLINE_CURVE ( 3, ( #27700, #67235, #61308, #22148 ),
 .UNSPECIFIED., .F., .F. ) 
 B_SPLINE_CURVE_WITH_KNOTS ( ( 4, 4 ),
 ( 4.712388980384689674, 6.283185307179586232 ),
 .UNSPECIFIED. ) 
 CURVE ( )  GEOMETRIC_REPRESENTATION_ITEM ( )  RATIONAL_B_SPLINE_CURVE ( ( 1.000000000000000000, 0.8047378541243649375, 0.8047378541243649375, 1.000000000000000000 ) ) 
 REPRESENTATION_ITEM ( '' )  );
#59405 = CARTESIAN_POINT ( 'NONE',  ( 12.12187500061451573, 3.027376345333613106, -5.243569643749998122 ) ) ;
#59406 = CARTESIAN_POINT ( 'NONE',  ( 3.756430356250000546, 13.12812499938548250, 27.83122392262697886 ) ) ;
#59407 = CARTESIAN_POINT ( 'NONE',  ( 23.85000000000000142, -4.330127018922190985, -2.500000000000001332 ) ) ;
#59408 = CARTESIAN_POINT ( 'NONE',  ( -3.999999999999999556, 15.38750000000000107, 27.69059892324149175 ) ) ;
#59409 = CARTESIAN_POINT ( 'NONE',  ( 2.121784821874999061, 11.60937500061451821, -33.67503911421598417 ) ) ;
#59410 = CARTESIAN_POINT ( 'NONE',  ( 25.24687500061451573, 5.492252693125287522, 3.363034840372157021E-16 ) ) ;
#59411 = CARTESIAN_POINT ( 'NONE',  ( 14.95312500061451644, 0.000000000000000000, 5.243569643749999010 ) ) ;
#59412 = CARTESIAN_POINT ( 'NONE',  ( 3.525000000000000355, -4.330127018922194537, 2.499999999999995559 ) ) ;
#59413 = DIRECTION ( 'NONE',  ( 0.000000000000000000, -1.000000000000000000, 8.673617379884035472E-17 ) ) ;
#59414 = FACE_OUTER_BOUND ( 'NONE', #40339, .T. ) ;
#59415 =( BOUNDED_CURVE ( )  B_SPLINE_CURVE ( 2, ( #23111, #27952, #62286, #44588, #33842, #39035, #5050, #15750, #34197, #28664, #16119, #33472, #49754, #51203, #55295, #56385, #66374, #38289, #10589, #28307, #32758, #50842, #72281, #242, #61194, #50119, #50484, #67120, #45301, #61549, #22751, #66749, #27587, #67835, #16843, #72650, #38672, #17208, #4689, #11682, #21660, #33117, #10951, #67480, #73009, #27219, #12751, #18274, #12035, #47106, #51567, #41208, #68203, #34560, #6496, #40481, #40126, #46023, #68560, #40848, #63716, #36010, #58528, #24194, #35286, #17918, #68917, #62996, #52642, #19000, #12391, #63366, #62640, #2049, #17564, #967, #34927, #35646, #24560, #51926, #7217, #57088, #29031, #1323, #46748, #57808, #69638, #58168, #29746, #23477, #57454, #6859, #29392, #23833, #46383, #52284, #1685, #69282, #7573, #18644, #2400, #41561, #13108, #30108, #64079, #13461, #7938, #30476, #53005, #45668, #2765, #26395, #36740, #71466, #31200, #64814, #65179, #14204, #8669, #47833, #19365, #42655, #54474, #31937, #20842, #30835, #25287, #48937, #59629, #3509, #9767, #3872, #70363, #41923, #19741, #54836, #9042, #43396, #53742, #71093, #70723, #42290, #64449, #37477, #65549, #69996, #65918, #54111, #15299, #37838, #14938, #59997, #60358, #59260, #32301, #3135, #9407, #53368, #24921, #25664, #48201, #47463, #31572, #26028, #48567, #20467, #43021, #13840, #36379, #58895, #8305, #20098, #14570, #37103, #157, #10138, #50399, #22663, #71836, #49668, #61106, #55211, #28224, #38948, #55930, #62198, #56299, #4604, #21206, #72196, #34111, #61466, #50754, #33031, #72924, #50032, #66656, #26770, #45213, #17119, #27135, #33754, #33394, #5689, #11231, #67394, #16756, #67747, #21575, #39678, #16033, #61826, #32670, #39314, #44129, #10503, #67033, #55570, #11594, #27498, #22306, #10861, #4243, #43759, #49302, #27867, #60727, #38581, #4965, #21945, #38201, #72557, #44500, #5326, #16393, #44858, #66284, #15662, #41121, #17828, #35559, #69555, #23024, #57724, #68112, #63633, #1965, #17478, #34838, #13021, #40389, #41475, #6045, #63995, #34473, #45580, #513, #28579, #18916, #40038, #62552, #13376, #28940, #62908, #1238, #12302, #6408, #51478, #23386, #879, #11948, #58079, #57364, #56650, #51116, #57001, #45935, #68466, #7487, #6772, #23743, #29304, #51834, #46291, #68832, #18188, #40758, #63273, #52559, #12665, #35202, #30016, #7129, #24108, #24474, #46656, #47020, #29659, #52196, #1597, #69196, #18556, #35919, #69910, #25194, #20751, #14850, #59174, #3043, #42933, #30390, #65093, #42204, #59913, #53279, #37017, #7854, #2317, #13752, #37389, #47739, #3422, #65458, #25942, #9319, #19648, #54027, #31852, #41831, #8952, #54388, #52919, #8219, #64728, #20382, #24832, #64362, #48482, #71006, #25574, #8582, #47380, #30747, #65829, #70637, #3784, #14114, #31485, #31111, #70277, #58443, #26308, #48846, #58808, #48114, #19278, #71376, #36294, #43309, #2678, #36653, #53650, #20012, #42565, #14483, #59541, #27775, #10050, #72102, #4874, #44039, #67308, #38490, #61378, #15574, #4520, #16666, #38862, #21487, #38116, #39224, #15942, #32944, #49217, #66196, #71751, #66940, #66562, #27410, #55482, #61015, #72837, #49580, #61736, #5603, #28139, #16308, #49941, #60637, #10412, #32583, #72465, #22219, #21850, #71, #37751, #22577, #55122, #4152, #32216, #60269, #50667, #21120, #43673, #26684, #9683, #44413, #10774, #33307, #11137, #5233, #33666, #54750, #27049, #55845, #50314, #44773, #56210, #45126, #15211, #45488, #51025, #47204, #52381, #7673, #35746, #41305, #53102, #29846, #47564, #58995, #34023, #69735, #5955, #2498, #13942, #28487, #46846, #25022, #1788, #53472, #17026, #2864, #68019, #56560, #11501, #39584, #30931, #421, #22929, #17392, #39949, #24298, #13207, #69386, #62462, #11860, #34380, #56912, #6317, #70094, #18741, #25394, #67660, #63815, #58267, #62108, #19470, #30210, #52742, #42028, #2147, #24658, #19104, #41659, #64181, #13569, #64549, #36113, #58634, #36477, #8041, #30576, #8402, #37938, #4343, #31674, #66016, #43859, #53843, #20940, #26868, #54937, #21305, #3237, #25765, #71930, #9504, #26494, #32768, #49399, #48301, #64915, #20201, #4699, #32033, #66384, #3604, #43491, #20564, #37207, #42393, #60457, #15396, #19841, #15760, #3971, #38300, #60828, #9866, #32397, #10234, #42755, #55305, #59729, #47937, #70827, #70466, #65276, #54207, #37571, #54569, #49037, #71566, #14305, #36842, #59357, #8769, #71190, #31303, #60095, #14664, #9137, #26126, #48665, #43122, #65646, #15034, #56741, #56394, #28674, #22759, #62649, #12046, #44599, #62295, #17573, #67489, #16487, #11332, #10599, #61926, #45676, #51214, #33850, #5784, #28315, #50851, #251, #23122, #66760, #33481, #27597, #6143, #16131, #614, #33127, #45311, #49766, #38683, #61204, #22040, #21670, #50129, #72660, #73019, #67846, #68212, #40135, #55664, #17218, #67130, #50493, #39044, #34207, #34569, #61558, #22403, #44227, #57098, #72292, #5060, #10960, #39779, #27229, #56031, #11691, #5423, #27961, #44951, #16852, #39408, #30486, #69647, #63726, #57464, #29042, #976, #51936, #1333, #12403, #35297, #23845, #69293, #19009, #51577, #36391, #58178, #7228, #63377, #13849, #53015, #46393, #7583, #23486, #46033, #6870, #7949, #18285, #2409, #12761, #68928, #46758, #40860, #57818, #29402, #68569, #47473, #24206, #36020, #13471, #29757, #64089, #17928, #34938, #24570, #41571 ),
 .UNSPECIFIED., .F., .F. ) 
 B_SPLINE_CURVE_WITH_KNOTS ( ( 3, 2, 2, 2, 2, 2, 2, 2, 2, 2, 2, 2, 2, 2, 2, 2, 2, 2, 2, 2, 2, 2, 2, 2, 2, 2, 2, 2, 2, 2, 2, 2, 2, 2, 2, 2, 2, 2, 2, 2, 2, 2, 2, 2, 2, 2, 2, 2, 2, 2, 2, 2, 2, 2, 2, 2, 2, 2, 2, 2, 2, 2, 2, 2, 2, 2, 2, 2, 2, 2, 2, 2, 2, 2, 2, 2, 2, 2, 2, 2, 2, 2, 2, 2, 2, 2, 2, 2, 2, 2, 2, 2, 2, 2, 2, 2, 2, 2, 2, 2, 2, 2, 2, 2, 2, 2, 2, 2, 2, 2, 2, 2, 2, 2, 2, 2, 2, 2, 2, 2, 2, 2, 2, 2, 2, 2, 2, 2, 2, 2, 2, 2, 2, 2, 2, 2, 2, 2, 2, 2, 2, 2, 2, 2, 2, 2, 2, 2, 2, 2, 2, 2, 2, 2, 2, 2, 2, 2, 2, 2, 2, 2, 2, 2, 2, 2, 2, 2, 2, 2, 2, 2, 2, 2, 2, 2, 2, 2, 2, 2, 2, 2, 2, 2, 2, 2, 2, 2, 2, 2, 2, 2, 2, 2, 2, 2, 2, 2, 2, 2, 2, 2, 2, 2, 2, 2, 2, 2, 2, 2, 2, 2, 2, 2, 2, 2, 2, 2, 2, 2, 2, 2, 2, 2, 2, 2, 2, 2, 2, 2, 2, 2, 2, 2, 2, 2, 2, 2, 2, 2, 2, 2, 2, 2, 2, 2, 2, 2, 2, 2, 2, 2, 2, 2, 2, 2, 2, 2, 2, 2, 2, 2, 2, 2, 2, 2, 2, 2, 2, 2, 2, 2, 2, 2, 2, 2, 2, 2, 2, 2, 2, 2, 2, 2, 2, 2, 2, 2, 2, 2, 2, 2, 2, 2, 2, 2, 2, 2, 2, 2, 2, 2, 2, 2, 2, 2, 2, 2, 2, 2, 2, 2, 2, 2, 2, 2, 2, 2, 2, 2, 2, 2, 2, 2, 2, 2, 2, 2, 2, 2, 2, 2, 2, 3 ),
 ( 0.000000000000000000, 0.002777777777777777884, 0.005555555555555555768, 0.008333333333333333218, 0.01111111111111111154, 0.01388888888888888812, 0.01666666666666666644, 0.01944444444444444475, 0.02222222222222222307, 0.02500000000000000139, 0.02777777777777777624, 0.03055555555555555455, 0.03333333333333333287, 0.03611111111111110772, 0.03888888888888888951, 0.04166666666666666435, 0.04444444444444444614, 0.04722222222222222099, 0.05000000000000000278, 0.05277777777777777762, 0.05555555555555555247, 0.05833333333333333426, 0.06111111111111110911, 0.06388888888888888395, 0.06666666666666666574, 0.06944444444444444753, 0.07222222222222221544, 0.07499999999999999722, 0.07777777777777777901, 0.08055555555555556080, 0.08333333333333332871, 0.08611111111111111049, 0.08888888888888889228, 0.09166666666666666019, 0.09444444444444444198, 0.09722222222222222376, 0.1000000000000000056, 0.1027777777777777873, 0.1055555555555555552, 0.1083333333333333370, 0.1111111111111111049, 0.1138888888888888867, 0.1166666666666666685, 0.1194444444444444503, 0.1222222222222222182, 0.1250000000000000000, 0.1277777777777777679, 0.1305555555555555636, 0.1333333333333333315, 0.1361111111111110994, 0.1388888888888888951, 0.1416666666666666630, 0.1444444444444444309, 0.1472222222222222265, 0.1499999999999999944, 0.1527777777777777901, 0.1555555555555555580, 0.1583333333333333259, 0.1611111111111111216, 0.1638888888888888895, 0.1666666666666666574, 0.1694444444444444253, 0.1722222222222222210, 0.1749999999999999889, 0.1777777777777777846, 0.1805555555555555525, 0.1833333333333333204, 0.1861111111111111160, 0.1888888888888888840, 0.1916666666666666796, 0.1944444444444444475, 0.1972222222222222154, 0.2000000000000000111, 0.2027777777777777790, 0.2055555555555555747, 0.2083333333333333426, 0.2111111111111111105, 0.2138888888888888784, 0.2166666666666666741, 0.2194444444444444420, 0.2222222222222222099, 0.2250000000000000056, 0.2277777777777777735, 0.2305555555555555691, 0.2333333333333333370, 0.2361111111111111049, 0.2388888888888889006, 0.2416666666666666685, 0.2444444444444444364, 0.2472222222222222321, 0.2500000000000000000, 0.2527777777777777679, 0.2555555555555555358, 0.2583333333333333592, 0.2611111111111111271, 0.2638888888888888951, 0.2666666666666666630, 0.2694444444444444309, 0.2722222222222221988, 0.2750000000000000222, 0.2777777777777777901, 0.2805555555555555580, 0.2833333333333333259, 0.2861111111111111494, 0.2888888888888888618, 0.2916666666666666852, 0.2944444444444444531, 0.2972222222222222210, 0.2999999999999999889, 0.3027777777777777568, 0.3055555555555555802, 0.3083333333333333481, 0.3111111111111111160, 0.3138888888888888840, 0.3166666666666666519, 0.3194444444444444198, 0.3222222222222222432, 0.3250000000000000111, 0.3277777777777777790, 0.3305555555555555469, 0.3333333333333333148, 0.3361111111111111382, 0.3388888888888888506, 0.3416666666666666741, 0.3444444444444444420, 0.3472222222222222099, 0.3499999999999999778, 0.3527777777777778012, 0.3555555555555555691, 0.3583333333333333370, 0.3611111111111111049, 0.3638888888888888729, 0.3666666666666666408, 0.3694444444444444642, 0.3722222222222222321, 0.3750000000000000000, 0.3777777777777777679, 0.3805555555555555358, 0.3833333333333333592, 0.3861111111111111271, 0.3888888888888888951, 0.3916666666666666630, 0.3944444444444444309, 0.3972222222222221988, 0.4000000000000000222, 0.4027777777777777901, 0.4055555555555555580, 0.4083333333333333259, 0.4111111111111111494, 0.4138888888888888618, 0.4166666666666666852, 0.4194444444444444531, 0.4222222222222222210, 0.4249999999999999889, 0.4277777777777777568, 0.4305555555555555802, 0.4333333333333333481, 0.4361111111111111160, 0.4388888888888888840, 0.4416666666666666519, 0.4444444444444444198, 0.4472222222222222432, 0.4500000000000000111, 0.4527777777777777790, 0.4555555555555555469, 0.4583333333333333148, 0.4611111111111111382, 0.4638888888888888506, 0.4666666666666666741, 0.4694444444444444420, 0.4722222222222222099, 0.4749999999999999778, 0.4777777777777778012, 0.4805555555555555691, 0.4833333333333333370, 0.4861111111111111049, 0.4888888888888888729, 0.4916666666666666408, 0.4944444444444444642, 0.4972222222222222321, 0.5000000000000000000, 0.5027777777777777679, 0.5055555555555555358, 0.5083333333333333037, 0.5111111111111110716, 0.5138888888888888395, 0.5166666666666667185, 0.5194444444444444864, 0.5222222222222222543, 0.5250000000000000222, 0.5277777777777777901, 0.5305555555555555580, 0.5333333333333333259, 0.5361111111111110938, 0.5388888888888888618, 0.5416666666666666297, 0.5444444444444443976, 0.5472222222222222765, 0.5500000000000000444, 0.5527777777777778123, 0.5555555555555555802, 0.5583333333333333481, 0.5611111111111111160, 0.5638888888888888840, 0.5666666666666666519, 0.5694444444444444198, 0.5722222222222222987, 0.5749999999999999556, 0.5777777777777777235, 0.5805555555555556024, 0.5833333333333333703, 0.5861111111111112493, 0.5888888888888889062, 0.5916666666666666741, 0.5944444444444444420, 0.5972222222222222099, 0.5999999999999999778, 0.6027777777777777457, 0.6055555555555555136, 0.6083333333333332815, 0.6111111111111111605, 0.6138888888888889284, 0.6166666666666666963, 0.6194444444444444642, 0.6222222222222222321, 0.6249999999999998890, 0.6277777777777777679, 0.6305555555555555358, 0.6333333333333333037, 0.6361111111111110716, 0.6388888888888888395, 0.6416666666666667185, 0.6444444444444444864, 0.6472222222222222543, 0.6500000000000000222, 0.6527777777777777901, 0.6555555555555555580, 0.6583333333333333259, 0.6611111111111110938, 0.6638888888888887507, 0.6666666666666666297, 0.6694444444444443976, 0.6722222222222222765, 0.6750000000000000444, 0.6777777777777777013, 0.6805555555555555802, 0.6833333333333333481, 0.6861111111111111160, 0.6888888888888888840, 0.6916666666666666519, 0.6944444444444444198, 0.6972222222222221877, 0.6999999999999999556, 0.7027777777777777235, 0.7055555555555556024, 0.7083333333333333703, 0.7111111111111111382, 0.7138888888888889062, 0.7166666666666666741, 0.7194444444444444420, 0.7222222222222222099, 0.7249999999999999778, 0.7277777777777777457, 0.7305555555555555136, 0.7333333333333332815, 0.7361111111111111605, 0.7388888888888889284, 0.7416666666666666963, 0.7444444444444444642, 0.7472222222222222321, 0.7500000000000000000, 0.7527777777777777679, 0.7555555555555555358, 0.7583333333333333037, 0.7611111111111110716, 0.7638888888888888395, 0.7666666666666667185, 0.7694444444444444864, 0.7722222222222222543, 0.7750000000000000222, 0.7777777777777777901, 0.7805555555555555580, 0.7833333333333333259, 0.7861111111111110938, 0.7888888888888888618, 0.7916666666666666297, 0.7944444444444443976, 0.7972222222222222765, 0.8000000000000000444, 0.8027777777777778123, 0.8055555555555555802, 0.8083333333333333481, 0.8111111111111111160, 0.8138888888888888840, 0.8166666666666666519, 0.8194444444444444198, 0.8222222222222222987, 0.8249999999999999556, 0.8277777777777777235, 0.8305555555555556024, 0.8333333333333333703, 0.8361111111111112493, 0.8388888888888889062, 0.8416666666666666741, 0.8444444444444444420, 0.8472222222222222099, 0.8499999999999999778, 0.8527777777777777457, 0.8555555555555555136, 0.8583333333333332815, 0.8611111111111111605, 0.8638888888888889284, 0.8666666666666666963, 0.8694444444444444642, 0.8722222222222222321, 0.8750000000000001110, 0.8777777777777777679, 0.8805555555555555358, 0.8833333333333333037, 0.8861111111111110716, 0.8888888888888888395, 0.8916666666666667185, 0.8944444444444444864, 0.8972222222222222543, 0.9000000000000000222, 0.9027777777777777901, 0.9055555555555555580, 0.9083333333333333259, 0.9111111111111110938, 0.9138888888888887507, 0.9166666666666666297, 0.9194444444444443976, 0.9222222222222222765, 0.9244751644120873246 ),
 .UNSPECIFIED. ) 
 CURVE ( )  GEOMETRIC_REPRESENTATION_ITEM ( )  RATIONAL_B_SPLINE_CURVE ( ( 1.000000000000000000, 0.8660254037844387076, 1.000000000000000000, 0.8660254037844387076, 1.000000000000000000, 0.8660254037844387076, 1.000000000000000000, 0.8660254037844387076, 1.000000000000000000, 0.8660254037844387076, 1.000000000000000000, 0.8660254037844387076, 1.000000000000000000, 0.8660254037844387076, 1.000000000000000000, 0.8660254037844387076, 1.000000000000000000, 0.8660254037844387076, 1.000000000000000000, 0.8660254037844387076, 1.000000000000000000, 0.8660254037844387076, 1.000000000000000000, 0.8660254037844387076, 1.000000000000000000, 0.8660254037844387076, 1.000000000000000000, 0.8660254037844387076, 1.000000000000000000, 0.8660254037844387076, 1.000000000000000000, 0.8660254037844387076, 1.000000000000000000, 0.8660254037844387076, 1.000000000000000000, 0.8660254037844387076, 1.000000000000000000, 0.8660254037844387076, 1.000000000000000000, 0.8660254037844387076, 1.000000000000000000, 0.8660254037844387076, 1.000000000000000000, 0.8660254037844387076, 1.000000000000000000, 0.8660254037844387076, 1.000000000000000000, 0.8660254037844387076, 1.000000000000000000, 0.8660254037844387076, 1.000000000000000000, 0.8660254037844387076, 1.000000000000000000, 0.8660254037844387076, 1.000000000000000000, 0.8660254037844387076, 1.000000000000000000, 0.8660254037844387076, 1.000000000000000000, 0.8660254037844387076, 1.000000000000000000, 0.8660254037844387076, 1.000000000000000000, 0.8660254037844387076, 1.000000000000000000, 0.8660254037844387076, 1.000000000000000000, 0.8660254037844387076, 1.000000000000000000, 0.8660254037844387076, 1.000000000000000000, 0.8660254037844387076, 1.000000000000000000, 0.8660254037844387076, 1.000000000000000000, 0.8660254037844387076, 1.000000000000000000, 0.8660254037844387076, 1.000000000000000000, 0.8660254037844387076, 1.000000000000000000, 0.8660254037844387076, 1.000000000000000000, 0.8660254037844387076, 1.000000000000000000, 0.8660254037844387076, 1.000000000000000000, 0.8660254037844387076, 1.000000000000000000, 0.8660254037844387076, 1.000000000000000000, 0.8660254037844387076, 1.000000000000000000, 0.8660254037844387076, 1.000000000000000000, 0.8660254037844387076, 1.000000000000000000, 0.8660254037844387076, 1.000000000000000000, 0.8660254037844387076, 1.000000000000000000, 0.8660254037844387076, 1.000000000000000000, 0.8660254037844387076, 1.000000000000000000, 0.8660254037844387076, 1.000000000000000000, 0.8660254037844387076, 1.000000000000000000, 0.8660254037844387076, 1.000000000000000000, 0.8660254037844387076, 1.000000000000000000, 0.8660254037844387076, 1.000000000000000000, 0.8660254037844387076, 1.000000000000000000, 0.8660254037844387076, 1.000000000000000000, 0.8660254037844387076, 1.000000000000000000, 0.8660254037844387076, 1.000000000000000000, 0.8660254037844387076, 1.000000000000000000, 0.8660254037844387076, 1.000000000000000000, 0.8660254037844387076, 1.000000000000000000, 0.8660254037844387076, 1.000000000000000000, 0.8660254037844387076, 1.000000000000000000, 0.8660254037844387076, 1.000000000000000000, 0.8660254037844387076, 1.000000000000000000, 0.8660254037844387076, 1.000000000000000000, 0.8660254037844387076, 1.000000000000000000, 0.8660254037844387076, 1.000000000000000000, 0.8660254037844387076, 1.000000000000000000, 0.8660254037844387076, 1.000000000000000000, 0.8660254037844387076, 1.000000000000000000, 0.8660254037844387076, 1.000000000000000000, 0.8660254037844387076, 1.000000000000000000, 0.8660254037844387076, 1.000000000000000000, 0.8660254037844387076, 1.000000000000000000, 0.8660254037844387076, 1.000000000000000000, 0.8660254037844387076, 1.000000000000000000, 0.8660254037844387076, 1.000000000000000000, 0.8660254037844387076, 1.000000000000000000, 0.8660254037844387076, 1.000000000000000000, 0.8660254037844387076, 1.000000000000000000, 0.8660254037844387076, 1.000000000000000000, 0.8660254037844387076, 1.000000000000000000, 0.8660254037844387076, 1.000000000000000000, 0.8660254037844387076, 1.000000000000000000, 0.8660254037844387076, 1.000000000000000000, 0.8660254037844387076, 1.000000000000000000, 0.8660254037844387076, 1.000000000000000000, 0.8660254037844387076, 1.000000000000000000, 0.8660254037844387076, 1.000000000000000000, 0.8660254037844387076, 1.000000000000000000, 0.8660254037844387076, 1.000000000000000000, 0.8660254037844387076, 1.000000000000000000, 0.8660254037844387076, 1.000000000000000000, 0.8660254037844387076, 1.000000000000000000, 0.8660254037844387076, 1.000000000000000000, 0.8660254037844387076, 1.000000000000000000, 0.8660254037844387076, 1.000000000000000000, 0.8660254037844387076, 1.000000000000000000, 0.8660254037844387076, 1.000000000000000000, 0.8660254037844387076, 1.000000000000000000, 0.8660254037844387076, 1.000000000000000000, 0.8660254037844387076, 1.000000000000000000, 0.8660254037844387076, 1.000000000000000000, 0.8660254037844387076, 1.000000000000000000, 0.8660254037844387076, 1.000000000000000000, 0.8660254037844387076, 1.000000000000000000, 0.8660254037844387076, 1.000000000000000000, 0.8660254037844387076, 1.000000000000000000, 0.8660254037844387076, 1.000000000000000000, 0.8660254037844387076, 1.000000000000000000, 0.8660254037844387076, 1.000000000000000000, 0.8660254037844387076, 1.000000000000000000, 0.8660254037844387076, 1.000000000000000000, 0.8660254037844387076, 1.000000000000000000, 0.8660254037844387076, 1.000000000000000000, 0.8660254037844387076, 1.000000000000000000, 0.8660254037844387076, 1.000000000000000000, 0.8660254037844387076, 1.000000000000000000, 0.8660254037844387076, 1.000000000000000000, 0.8660254037844387076, 1.000000000000000000, 0.8660254037844387076, 1.000000000000000000, 0.8660254037844387076, 1.000000000000000000, 0.8660254037844387076, 1.000000000000000000, 0.8660254037844387076, 1.000000000000000000, 0.8660254037844387076, 1.000000000000000000, 0.8660254037844387076, 1.000000000000000000, 0.8660254037844387076, 1.000000000000000000, 0.8660254037844387076, 1.000000000000000000, 0.8660254037844387076, 1.000000000000000000, 0.8660254037844387076, 1.000000000000000000, 0.8660254037844387076, 1.000000000000000000, 0.8660254037844387076, 1.000000000000000000, 0.8660254037844387076, 1.000000000000000000, 0.8660254037844387076, 1.000000000000000000, 0.8660254037844387076, 1.000000000000000000, 0.8660254037844387076, 1.000000000000000000, 0.8660254037844387076, 1.000000000000000000, 0.8660254037844387076, 1.000000000000000000, 0.8660254037844387076, 1.000000000000000000, 0.8660254037844387076, 1.000000000000000000, 0.8660254037844387076, 1.000000000000000000, 0.8660254037844387076, 1.000000000000000000, 0.8660254037844387076, 1.000000000000000000, 0.8660254037844387076, 1.000000000000000000, 0.8660254037844387076, 1.000000000000000000, 0.8660254037844387076, 1.000000000000000000, 0.8660254037844387076, 1.000000000000000000, 0.8660254037844387076, 1.000000000000000000, 0.8660254037844387076, 1.000000000000000000, 0.8660254037844387076, 1.000000000000000000, 0.8660254037844387076, 1.000000000000000000, 0.8660254037844387076, 1.000000000000000000, 0.8660254037844387076, 1.000000000000000000, 0.8660254037844387076, 1.000000000000000000, 0.8660254037844387076, 1.000000000000000000, 0.8660254037844387076, 1.000000000000000000, 0.8660254037844387076, 1.000000000000000000, 0.8660254037844387076, 1.000000000000000000, 0.8660254037844387076, 1.000000000000000000, 0.8660254037844387076, 1.000000000000000000, 0.8660254037844387076, 1.000000000000000000, 0.8660254037844387076, 1.000000000000000000, 0.8660254037844387076, 1.000000000000000000, 0.8660254037844387076, 1.000000000000000000, 0.8660254037844387076, 1.000000000000000000, 0.8660254037844387076, 1.000000000000000000, 0.8660254037844387076, 1.000000000000000000, 0.8660254037844387076, 1.000000000000000000, 0.8660254037844387076, 1.000000000000000000, 0.8660254037844387076, 1.000000000000000000, 0.8660254037844387076, 1.000000000000000000, 0.8660254037844387076, 1.000000000000000000, 0.8660254037844387076, 1.000000000000000000, 0.8660254037844387076, 1.000000000000000000, 0.8660254037844387076, 1.000000000000000000, 0.8660254037844387076, 1.000000000000000000, 0.8660254037844387076, 1.000000000000000000, 0.8660254037844387076, 1.000000000000000000, 0.8660254037844387076, 1.000000000000000000, 0.8660254037844387076, 1.000000000000000000, 0.8660254037844387076, 1.000000000000000000, 0.8660254037844387076, 1.000000000000000000, 0.8660254037844387076, 1.000000000000000000, 0.8660254037844387076, 1.000000000000000000, 0.8660254037844387076, 1.000000000000000000, 0.8660254037844387076, 1.000000000000000000, 0.8660254037844387076, 1.000000000000000000, 0.8660254037844387076, 1.000000000000000000, 0.8660254037844387076, 1.000000000000000000, 0.8660254037844387076, 1.000000000000000000, 0.8660254037844387076, 1.000000000000000000, 0.8660254037844387076, 1.000000000000000000, 0.8660254037844387076, 1.000000000000000000, 0.8660254037844387076, 1.000000000000000000, 0.8660254037844387076, 1.000000000000000000, 0.8660254037844387076, 1.000000000000000000, 0.8660254037844387076, 1.000000000000000000, 0.8660254037844387076, 1.000000000000000000, 0.8660254037844387076, 1.000000000000000000, 0.8660254037844387076, 1.000000000000000000, 0.8660254037844387076, 1.000000000000000000, 0.8660254037844387076, 1.000000000000000000, 0.8660254037844387076, 1.000000000000000000, 0.8660254037844387076, 1.000000000000000000, 0.8660254037844387076, 1.000000000000000000, 0.8660254037844387076, 1.000000000000000000, 0.8660254037844387076, 1.000000000000000000, 0.8660254037844387076, 1.000000000000000000, 0.8660254037844387076, 1.000000000000000000, 0.8660254037844387076, 1.000000000000000000, 0.8660254037844387076, 1.000000000000000000, 0.8660254037844387076, 1.000000000000000000, 0.8660254037844387076, 1.000000000000000000, 0.8660254037844387076, 1.000000000000000000, 0.8660254037844387076, 1.000000000000000000, 0.8660254037844387076, 1.000000000000000000, 0.8660254037844387076, 1.000000000000000000, 0.8660254037844387076, 1.000000000000000000, 0.8660254037844387076, 1.000000000000000000, 0.8660254037844387076, 1.000000000000000000, 0.8660254037844387076, 1.000000000000000000, 0.8660254037844387076, 1.000000000000000000, 0.8660254037844387076, 1.000000000000000000, 0.8660254037844387076, 1.000000000000000000, 0.8660254037844387076, 1.000000000000000000, 0.8660254037844387076, 1.000000000000000000, 0.8660254037844387076, 1.000000000000000000, 0.8660254037844387076, 1.000000000000000000, 0.8660254037844387076, 1.000000000000000000, 0.8660254037844387076, 1.000000000000000000, 0.8660254037844387076, 1.000000000000000000, 0.8660254037844387076, 1.000000000000000000, 0.8660254037844387076, 1.000000000000000000, 0.8660254037844387076, 1.000000000000000000, 0.8660254037844387076, 1.000000000000000000, 0.8660254037844387076, 1.000000000000000000, 0.8660254037844387076, 1.000000000000000000, 0.8660254037844387076, 1.000000000000000000, 0.8660254037844387076, 1.000000000000000000, 0.8660254037844387076, 1.000000000000000000, 0.8660254037844387076, 1.000000000000000000, 0.8660254037844387076, 1.000000000000000000, 0.8660254037844387076, 1.000000000000000000, 0.8660254037844387076, 1.000000000000000000, 0.8660254037844387076, 1.000000000000000000, 0.8660254037844387076, 1.000000000000000000, 0.8660254037844387076, 1.000000000000000000, 0.8660254037844387076, 1.000000000000000000, 0.8660254037844387076, 1.000000000000000000, 0.8660254037844387076, 1.000000000000000000, 0.8660254037844387076, 1.000000000000000000, 0.8660254037844387076, 1.000000000000000000, 0.8660254037844387076, 1.000000000000000000, 0.8660254037844387076, 1.000000000000000000, 0.8660254037844387076, 1.000000000000000000, 0.8660254037844387076, 1.000000000000000000, 0.8660254037844387076, 1.000000000000000000, 0.8660254037844387076, 1.000000000000000000, 0.8660254037844387076, 1.000000000000000000, 0.8660254037844387076, 1.000000000000000000, 0.8660254037844387076, 1.000000000000000000, 0.8660254037844387076, 1.000000000000000000, 0.8660254037844387076, 1.000000000000000000, 0.8660254037844387076, 1.000000000000000000, 0.8660254037844387076, 1.000000000000000000, 0.8660254037844387076, 1.000000000000000000, 0.8660254037844387076, 1.000000000000000000, 0.8660254037844387076, 1.000000000000000000, 0.8660254037844387076, 1.000000000000000000, 0.8660254037844387076, 1.000000000000000000, 0.8660254037844387076, 1.000000000000000000, 0.8660254037844387076, 1.000000000000000000, 0.8660254037844387076, 1.000000000000000000, 0.8660254037844387076, 1.000000000000000000, 0.8660254037844387076, 1.000000000000000000, 0.8660254037844387076, 1.000000000000000000, 0.8660254037844387076, 1.000000000000000000, 0.8660254037844387076, 1.000000000000000000, 0.8660254037844387076, 1.000000000000000000, 0.8660254037844387076, 1.000000000000000000, 0.8660254037844387076, 1.000000000000000000, 0.8660254037844387076, 1.000000000000000000, 0.8660254037844387076, 1.000000000000000000, 0.8660254037844387076, 1.000000000000000000, 0.8660254037844387076, 1.000000000000000000, 0.8660254037844387076, 1.000000000000000000, 0.8660254037844387076, 1.000000000000000000, 0.8660254037844387076, 1.000000000000000000, 0.8660254037844387076, 1.000000000000000000, 0.8660254037844387076, 1.000000000000000000, 0.8660254037844387076, 1.000000000000000000, 0.8660254037844387076, 1.000000000000000000, 0.8660254037844387076, 1.000000000000000000, 0.8660254037844387076, 1.000000000000000000, 0.8660254037844387076, 1.000000000000000000, 0.8660254037844387076, 1.000000000000000000, 0.8660254037844387076, 1.000000000000000000, 0.8660254037844387076, 1.000000000000000000, 0.8660254037844387076, 1.000000000000000000, 0.8660254037844387076, 1.000000000000000000, 0.8660254037844387076, 1.000000000000000000, 0.8660254037844387076, 1.000000000000000000, 0.8660254037844387076, 1.000000000000000000, 0.8660254037844387076, 1.000000000000000000, 0.8660254037844387076, 1.000000000000000000, 0.8660254037844387076, 1.000000000000000000, 0.8660254037844387076, 1.000000000000000000, 0.8660254037844387076, 1.000000000000000000, 0.8660254037844387076, 1.000000000000000000, 0.8660254037844387076, 1.000000000000000000, 0.8660254037844387076, 1.000000000000000000, 0.8660254037844387076, 1.000000000000000000, 0.8660254037844387076, 1.000000000000000000, 0.8660254037844387076, 1.000000000000000000, 0.8660254037844387076, 1.000000000000000000, 0.8660254037844387076, 1.000000000000000000, 0.8660254037844387076, 1.000000000000000000, 0.8660254037844387076, 1.000000000000000000, 0.8660254037844387076, 1.000000000000000000, 0.8660254037844387076, 1.000000000000000000, 0.8660254037844387076, 1.000000000000000000, 0.8660254037844387076, 1.000000000000000000, 0.8660254037844387076, 1.000000000000000000, 0.8660254037844387076, 1.000000000000000000, 0.8660254037844387076, 1.000000000000000000, 0.8660254037844387076, 1.000000000000000000, 0.8660254037844387076, 1.000000000000000000, 0.8660254037844387076, 1.000000000000000000, 0.8913386727337029303, 0.9589388812629791037 ) ) 
 REPRESENTATION_ITEM ( '' )  );
#59416 = CARTESIAN_POINT ( 'NONE',  ( 12.22499999999999964, 6.123233995736764310E-16, -4.999999999999998224 ) ) ;
#59417 = CARTESIAN_POINT ( 'NONE',  ( 3.999999999999998668, 16.77500000122903145, 27.69059892324149175 ) ) ;
#59418 = CARTESIAN_POINT ( 'NONE',  ( 11.47500000122903252, 2.886751345948129099, -4.999999999999998224 ) ) ;
#59419 = CARTESIAN_POINT ( 'NONE',  ( 22.47187500061451715, 3.027376345333613106, -5.243569643749998122 ) ) ;
#59420 = CARTESIAN_POINT ( 'NONE',  ( 16.84687500061451715, -3.027376345333614438, 5.243569643749998122 ) ) ;
#59421 = CARTESIAN_POINT ( 'NONE',  ( 45.00000000000000000, 0.000000000000000000, 4.999999999999998224 ) ) ;
#59422 = ORIENTED_EDGE ( 'NONE', *, *, #10971, .F. ) ;
#59423 = CARTESIAN_POINT ( 'NONE',  ( 18.02812500061451573, 4.541064518000418104, 2.621784821874999949 ) ) ;
#59424 = CARTESIAN_POINT ( 'NONE',  ( 4.003125000614518925, 4.541064518000418104, -2.621784821874998173 ) ) ;
#59425 = CARTESIAN_POINT ( 'NONE',  ( 18.42187500061451644, 3.027376345333613106, -5.243569643749998122 ) ) ;
#59426 = CARTESIAN_POINT ( 'NONE',  ( 29.14687500061451075, -3.027376345333610441, -5.243569643749999898 ) ) ;
#59427 = CARTESIAN_POINT ( 'NONE',  ( 4.865625000614517859, 3.027376345333613106, -5.243569643749998122 ) ) ;
#59428 = CARTESIAN_POINT ( 'NONE',  ( 19.34062500061451573, 6.054752690667223547, 3.707466751127219781E-16 ) ) ;
#59429 = CARTESIAN_POINT ( 'NONE',  ( -2.121784821874996840, 14.47812500061451679, 33.67503911421598417 ) ) ;
#59430 = CARTESIAN_POINT ( 'NONE',  ( 15.48750000122903359, 6.123233995736764310E-16, -4.999999999999998224 ) ) ;
#59431 = CARTESIAN_POINT ( 'NONE',  ( 11.67187500061451821, 2.746126346562645981, -4.756430356249997438 ) ) ;
#59432 = CARTESIAN_POINT ( 'NONE',  ( 6.103125000614515905, -4.541064518000417216, -2.621784821875001281 ) ) ;
#59433 = CARTESIAN_POINT ( 'NONE',  ( 29.80312500061451431, 0.000000000000000000, 5.243569643749999010 ) ) ;
#59434 = CARTESIAN_POINT ( 'NONE',  ( 3.999999999999998668, 19.02500000122903501, -32.30940107675850470 ) ) ;
#59435 = CARTESIAN_POINT ( 'NONE',  ( 23.40937500061451715, 4.541064518000418104, -2.621784821874998173 ) ) ;
#59436 = CARTESIAN_POINT ( 'NONE',  ( 13.94062500061451892, 6.054752690667223547, 3.707466751127219781E-16 ) ) ;
#59437 = CARTESIAN_POINT ( 'NONE',  ( 25.27500000122903145, -5.773502691896255534, -1.060575238724906372E-15 ) ) ;
#59438 =( BOUNDED_CURVE ( )  B_SPLINE_CURVE ( 2, ( #68318, #16596, #6252, #2, #16960, #72765, #69665, #39885, #5167 ),
 .UNSPECIFIED., .F., .T. ) 
 B_SPLINE_CURVE_WITH_KNOTS ( ( 3, 2, 2, 2, 3 ),
 ( 0.5326086956521739468, 0.5362318840579710644, 0.5434782608695651884, 0.5507246376811594235, 0.5543478260869565410 ),
 .UNSPECIFIED. ) 
 CURVE ( )  GEOMETRIC_REPRESENTATION_ITEM ( )  RATIONAL_B_SPLINE_CURVE ( ( 0.9330127018922194093, 0.9330127018922194093, 1.000000000000000000, 0.8660254037844387076, 1.000000000000000000, 0.8660254037844387076, 1.000000000000000000, 0.9330127018922194093, 0.9330127018922194093 ) ) 
 REPRESENTATION_ITEM ( '' )  );
#59439 = CARTESIAN_POINT ( 'NONE',  ( 23.72812500061451502, 6.421520780324663323E-16, -5.243569643749999010 ) ) ;
#59440 = CARTESIAN_POINT ( 'NONE',  ( 19.99687500061451573, -3.027376345333614438, 5.243569643749998122 ) ) ;
#59441 = CARTESIAN_POINT ( 'NONE',  ( 15.10312500061451502, -4.541064518000417216, -2.621784821875001281 ) ) ;
#59442 = CARTESIAN_POINT ( 'NONE',  ( -4.243569643749999898, 14.90937500061451715, 30.00000000000000000 ) ) ;
#59443 = CARTESIAN_POINT ( 'NONE',  ( 19.00312500061451715, 0.000000000000000000, 5.243569643749999010 ) ) ;
#59444 = CARTESIAN_POINT ( 'NONE',  ( 29.65312500061451573, 4.541064518000418104, -2.621784821874998173 ) ) ;
#59445 = ORIENTED_EDGE ( 'NONE', *, *, #1067, .T. ) ;
#59446 = ORIENTED_EDGE ( 'NONE', *, *, #32425, .T. ) ;
#59447 = CARTESIAN_POINT ( 'NONE',  ( 23.28750000000000142, -2.886751345948129988, 4.999999999999997335 ) ) ;
#59448 = CARTESIAN_POINT ( 'NONE',  ( -3.999999999999997335, 10.58750000000000213, -27.69059892324149175 ) ) ;
#59449 = CARTESIAN_POINT ( 'NONE',  ( 4.000000000000000000, 18.05000000122903359, 32.30940107675849760 ) ) ;
#59450 = CARTESIAN_POINT ( 'NONE',  ( 25.97812500061451502, 6.421520780324663323E-16, -5.243569643749999010 ) ) ;
#59451 = CARTESIAN_POINT ( 'NONE',  ( 7.640625000614517326, 6.054752690667223547, 3.707466751127219781E-16 ) ) ;
#59452 = CARTESIAN_POINT ( 'NONE',  ( 19.53750000122903430, 6.123233995736764310E-16, -4.999999999999998224 ) ) ;
#59453 = CARTESIAN_POINT ( 'NONE',  ( 24.62812500061451715, 6.421520780324663323E-16, -5.243569643749999010 ) ) ;
#59454 = CARTESIAN_POINT ( 'NONE',  ( 22.01249999999999574, -5.773502691896255534, -1.060575238724906372E-15 ) ) ;
#59455 = CARTESIAN_POINT ( 'NONE',  ( 29.01562500061451644, -6.054752690667223547, -1.112240025338166033E-15 ) ) ;
#59456 = CARTESIAN_POINT ( 'NONE',  ( 7.415625000614516793, -6.054752690667223547, -1.112240025338166033E-15 ) ) ;
#59457 = VERTEX_POINT ( 'NONE', #51945 ) ;
#59458 = CARTESIAN_POINT ( 'NONE',  ( 23.57812500061451289, -4.541064518000419881, 2.621784821874995952 ) ) ;
#59459 = CARTESIAN_POINT ( 'NONE',  ( 5.765625000614519102, 3.027376345333613106, -5.243569643749998122 ) ) ;
#59460 = CARTESIAN_POINT ( 'NONE',  ( 13.47187500061451537, 2.746126346562645981, -4.756430356249997438 ) ) ;
#59461 = CARTESIAN_POINT ( 'NONE',  ( 3.178125000614515638, 4.541064518000418104, 2.621784821874999949 ) ) ;
#59462 = CARTESIAN_POINT ( 'NONE',  ( -2.000000000000000000, 12.83750000122903501, -33.46410161513775705 ) ) ;
#59463 = CARTESIAN_POINT ( 'NONE',  ( -3.999999999999999112, 10.21250000122903501, 30.00000000000000000 ) ) ;
#59464 = CARTESIAN_POINT ( 'NONE',  ( 11.92500000000000071, 4.330127018922191873, 2.499999999999999556 ) ) ;
#59465 = CARTESIAN_POINT ( 'NONE',  ( 10.39687500061451786, 6.054752690667223547, 3.707466751127219781E-16 ) ) ;
#59466 = CARTESIAN_POINT ( 'NONE',  ( 9.000000001229034652, -2.886751345948129988, 4.999999999999997335 ) ) ;
#59467 = CARTESIAN_POINT ( 'NONE',  ( 15.04687500061451644, -3.027376345333614438, 5.243569643749998122 ) ) ;
#59468 = CARTESIAN_POINT ( 'NONE',  ( 15.15000000000000036, 0.000000000000000000, 4.999999999999998224 ) ) ;
#59469 = CARTESIAN_POINT ( 'NONE',  ( 6.234375000614519102, 6.421520780324663323E-16, -5.243569643749999010 ) ) ;
#59470 = CARTESIAN_POINT ( 'NONE',  ( -2.121784821874996840, 10.42812500061451786, -26.32496088578401583 ) ) ;
#59471 = DIRECTION ( 'NONE',  ( -1.000000000000000000, -0.000000000000000000, -0.000000000000000000 ) ) ;
#59472 = CARTESIAN_POINT ( 'NONE',  ( 12.90937500061451537, -4.541064518000417216, -2.621784821875001281 ) ) ;
#59473 = ORIENTED_EDGE ( 'NONE', *, *, #44600, .F. ) ;
#59474 = CARTESIAN_POINT ( 'NONE',  ( 22.41562500061451502, 3.027376345333613106, -5.243569643749998122 ) ) ;
#59475 = LINE ( 'NONE', #71307, #16829 ) ;
#59476 = CARTESIAN_POINT ( 'NONE',  ( -3.999999999999999112, 17.41250000122903430, 30.00000000000000000 ) ) ;
#59477 = CARTESIAN_POINT ( 'NONE',  ( 27.19687500061451857, -3.027376345333614438, 5.243569643749998122 ) ) ;
#59478 = EDGE_CURVE ( 'NONE', #55622, #49981, #6879, .T. ) ;
#59479 = CARTESIAN_POINT ( 'NONE',  ( 1.071796769724488785, 16.45759618943233704, 34.00000000000000000 ) ) ;
#59480 = CARTESIAN_POINT ( 'NONE',  ( 5.315625000614516260, 3.027376345333613106, -5.243569643749998122 ) ) ;
#59481 = CARTESIAN_POINT ( 'NONE',  ( 22.92187500061451644, 4.119189519843966529, 2.378215178124999607 ) ) ;
#59482 = CARTESIAN_POINT ( 'NONE',  ( 16.32187500061451502, 3.027376345333611329, 5.243569643749999010 ) ) ;
#59483 = CARTESIAN_POINT ( 'NONE',  ( 8.334375000614516082, -2.746126346562641984, -4.756430356249999214 ) ) ;
#59484 = CARTESIAN_POINT ( 'NONE',  ( 27.41250000122903430, 0.000000000000000000, 4.999999999999998224 ) ) ;
#59485 = CARTESIAN_POINT ( 'NONE',  ( 6.046875000614519102, -3.027376345333614438, 5.243569643749998122 ) ) ;
#59486 = CARTESIAN_POINT ( 'NONE',  ( 16.54687500061451644, -3.027376345333610441, -5.243569643749999898 ) ) ;
#59487 = CARTESIAN_POINT ( 'NONE',  ( -3.794299971169996066, 25.05385333968535733, 28.70714863339405554 ) ) ;
#59488 = CARTESIAN_POINT ( 'NONE',  ( 24.71250000000000213, -5.773502691896255534, -1.060575238724906372E-15 ) ) ;
#59489 = CARTESIAN_POINT ( 'NONE',  ( 4.800000001229032698, 5.773502691896255534, 3.535250795749688894E-16 ) ) ;
#59490 = CARTESIAN_POINT ( 'NONE',  ( 26.59687500061451360, 6.054752690667223547, 3.707466751127219781E-16 ) ) ;
#59491 = CARTESIAN_POINT ( 'NONE',  ( 3.756430356250000102, 12.75312499938548427, 30.00000000000000000 ) ) ;
#59492 = CARTESIAN_POINT ( 'NONE',  ( 8.831250001229033586, 4.330127018922191873, 2.499999999999999556 ) ) ;
#59493 = CARTESIAN_POINT ( 'NONE',  ( 8.737500000000002487, 5.773502691896255534, 3.535250795749688894E-16 ) ) ;
#59494 = CARTESIAN_POINT ( 'NONE',  ( 9.609375000614514661, -5.492252693125287522, -1.008910452111647106E-15 ) ) ;
#59495 = CARTESIAN_POINT ( 'NONE',  ( 23.09062500061451573, -3.027376345333614438, 5.243569643749998122 ) ) ;
#59496 = CARTESIAN_POINT ( 'NONE',  ( 10.98750000000000071, 5.773502691896255534, 3.535250795749688894E-16 ) ) ;
#59497 = CARTESIAN_POINT ( 'NONE',  ( 5.578125000614518214, -4.541064518000419881, 2.621784821874995952 ) ) ;
#59498 = CARTESIAN_POINT ( 'NONE',  ( 20.10000000000000142, 0.000000000000000000, 4.999999999999998224 ) ) ;
#59499 = CARTESIAN_POINT ( 'NONE',  ( 19.56562500061451715, -6.054752690667223547, -1.112240025338166033E-15 ) ) ;
#59500 = CARTESIAN_POINT ( 'NONE',  ( 4.177602232894093603, -2.747429830345227142, 4.435137505375752909 ) ) ;
#59501 = CARTESIAN_POINT ( 'NONE',  ( 23.58750000122903145, 6.123233995736764310E-16, -4.999999999999998224 ) ) ;
#59502 = CARTESIAN_POINT ( 'NONE',  ( -7.967954043666661671E-16, 20.17812499938548143, 34.33755215474603517 ) ) ;
#59503 = CARTESIAN_POINT ( 'NONE',  ( 3.487500000000000711, -2.886751345948129988, 4.999999999999997335 ) ) ;
#59504 = ORIENTED_EDGE ( 'NONE', *, *, #6481, .T. ) ;
#59505 = CARTESIAN_POINT ( 'NONE',  ( 20.09062500061451573, -3.027376345333610441, -5.243569643749999898 ) ) ;
#59506 = CARTESIAN_POINT ( 'NONE',  ( 25.79062500061451502, -3.027376345333614438, 5.243569643749998122 ) ) ;
#59507 = CARTESIAN_POINT ( 'NONE',  ( 23.82187500061451502, 3.027376345333613106, -5.243569643749998122 ) ) ;
#59508 = CARTESIAN_POINT ( 'NONE',  ( 7.837499999999999467, 5.773502691896255534, 3.535250795749688894E-16 ) ) ;
#59509 = CARTESIAN_POINT ( 'NONE',  ( 11.61562500061451608, 3.027376345333613106, -5.243569643749998122 ) ) ;
#59510 = CARTESIAN_POINT ( 'NONE',  ( 25.94062500061451715, -3.027376345333610441, -5.243569643749999898 ) ) ;
#59511 = CARTESIAN_POINT ( 'NONE',  ( 16.62187500061451573, 3.027376345333613106, -5.243569643749998122 ) ) ;
#59512 = CARTESIAN_POINT ( 'NONE',  ( 9.103125000614515017, 0.000000000000000000, 5.243569643749999010 ) ) ;
#59513 = CARTESIAN_POINT ( 'NONE',  ( 65.00000000000000000, 7.332543590861083871, -5.218601775200134796 ) ) ;
#59514 = CARTESIAN_POINT ( 'NONE',  ( -4.243569643749999898, 11.30937500061451928, 30.00000000000000000 ) ) ;
#59515 = EDGE_CURVE ( 'NONE', #46954, #3601, #42332, .T. ) ;
#59516 = CARTESIAN_POINT ( 'NONE',  ( 24.75000000122902932, -2.886751345948129988, 4.999999999999997335 ) ) ;
#59517 = CARTESIAN_POINT ( 'NONE',  ( 20.25937500061451857, 4.119189519843966529, -2.378215178124998275 ) ) ;
#59518 = CARTESIAN_POINT ( 'NONE',  ( 14.84062500061451750, 6.054752690667223547, 3.707466751127219781E-16 ) ) ;
#59519 = CARTESIAN_POINT ( 'NONE',  ( 10.02187500061451964, 3.027376345333611329, 5.243569643749999010 ) ) ;
#59520 = CARTESIAN_POINT ( 'NONE',  ( 10.35937500061451644, 4.541064518000418104, -2.621784821874998173 ) ) ;
#59521 = ORIENTED_EDGE ( 'NONE', *, *, #16132, .T. ) ;
#59522 = CARTESIAN_POINT ( 'NONE',  ( 15.22500000000000142, -4.330127018922194537, 2.499999999999995559 ) ) ;
#59523 = CARTESIAN_POINT ( 'NONE',  ( 21.40312500061451573, -4.541064518000417216, -2.621784821875001281 ) ) ;
#59524 = CARTESIAN_POINT ( 'NONE',  ( 15.98437500061451821, -4.541064518000419881, 2.621784821874995952 ) ) ;
#59525 = CARTESIAN_POINT ( 'NONE',  ( 21.77812500061451928, -4.541064518000419881, 2.621784821874995952 ) ) ;
#59526 = CARTESIAN_POINT ( 'NONE',  ( 1.999999999999998668, 11.75000000000000178, 26.53589838486224650 ) ) ;
#59527 = AXIS2_PLACEMENT_3D ( 'NONE', #44517, #6063, #38598 ) ;
#59528 = CARTESIAN_POINT ( 'NONE',  ( 26.24062500061451431, -3.027376345333614438, 5.243569643749998122 ) ) ;
#59529 = CARTESIAN_POINT ( 'NONE',  ( 7.387500001229032165, 6.123233995736764310E-16, -4.999999999999998224 ) ) ;
#59530 = VERTEX_POINT ( 'NONE', #40868 ) ;
#59531 = CARTESIAN_POINT ( 'NONE',  ( 3.300000001229034918, -2.886751345948125991, -5.000000000000000000 ) ) ;
#59532 = CARTESIAN_POINT ( 'NONE',  ( -2.000000000000000000, 17.22500000000000142, -33.46410161513775705 ) ) ;
#59533 = CARTESIAN_POINT ( 'NONE',  ( 25.27500000122903145, -5.773502691896255534, -1.060575238724906372E-15 ) ) ;
#59534 = CARTESIAN_POINT ( 'NONE',  ( -3.756430356250001434, 15.26562499938548356, 32.16877607737301048 ) ) ;
#59535 = CARTESIAN_POINT ( 'NONE',  ( 6.609375000614519102, -4.541064518000417216, -2.621784821875001281 ) ) ;
#59536 = DIRECTION ( 'NONE',  ( 0.000000000000000000, 0.000000000000000000, 1.000000000000000000 ) ) ;
#59537 = EDGE_CURVE ( 'NONE', #32794, #61283, #35216, .T. ) ;
#59538 = CARTESIAN_POINT ( 'NONE',  ( 16.04062500061451857, -3.027376345333610441, -5.243569643749999898 ) ) ;
#59539 = CARTESIAN_POINT ( 'NONE',  ( 8.671875000614518214, 3.027376345333611329, 5.243569643749999010 ) ) ;
#59540 = CARTESIAN_POINT ( 'NONE',  ( 26.62500000122903288, -5.773502691896255534, -1.060575238724906372E-15 ) ) ;
#59541 = CARTESIAN_POINT ( 'NONE',  ( 16.17187500061451644, 3.027376345333612662, -5.243569643749998122 ) ) ;
#59542 = CARTESIAN_POINT ( 'NONE',  ( 5.821875000614519458, 3.027376345333613106, -5.243569643749998122 ) ) ;
#59543 = CARTESIAN_POINT ( 'NONE',  ( 4.861368277861656928, -1.180116475822727162, 4.861368277861656928 ) ) ;
#59544 = CARTESIAN_POINT ( 'NONE',  ( 6.478125000614516793, -4.541064518000419881, 2.621784821874995952 ) ) ;
#59545 = CARTESIAN_POINT ( 'NONE',  ( 15.21562500061451750, 3.027376345333613106, -5.243569643749998122 ) ) ;
#59546 = ORIENTED_EDGE ( 'NONE', *, *, #28336, .T. ) ;
#59547 = CARTESIAN_POINT ( 'NONE',  ( 13.49062500061451608, 6.054752690667223547, 3.707466751127219781E-16 ) ) ;
#59548 = CARTESIAN_POINT ( 'NONE',  ( 6.562500001229032875, 4.330127018922192761, -2.499999999999997780 ) ) ;
#59549 = VECTOR ( 'NONE', #8237, 1000.000000000000000 ) ;
#59550 = CARTESIAN_POINT ( 'NONE',  ( 11.35312500061451679, 0.000000000000000000, 5.243569643749999010 ) ) ;
#59551 = CARTESIAN_POINT ( 'NONE',  ( 21.79687500061451644, -2.746126346562646425, 4.756430356249996549 ) ) ;
#59552 = CARTESIAN_POINT ( 'NONE',  ( 9.825000000000001066, -4.330127018922194537, 2.499999999999995559 ) ) ;
#59553 = CARTESIAN_POINT ( 'NONE',  ( 4.162500001229033408, -4.330127018922190985, -2.500000000000001332 ) ) ;
#59554 = CARTESIAN_POINT ( 'NONE',  ( 21.44999999999999929, 0.000000000000000000, 4.999999999999998224 ) ) ;
#59555 = CARTESIAN_POINT ( 'NONE',  ( 15.45937500061451608, 0.000000000000000000, 5.243569643749999010 ) ) ;
#59556 = CARTESIAN_POINT ( 'NONE',  ( 16.20000000122903216, -2.886751345948129988, 4.999999999999997335 ) ) ;
#59557 = CARTESIAN_POINT ( 'NONE',  ( 22.80000000000000071, 0.000000000000000000, 4.999999999999998224 ) ) ;
#59558 = CARTESIAN_POINT ( 'NONE',  ( -4.243569643749997233, 17.14062500061451644, -27.54997392385601174 ) ) ;
#59559 = CARTESIAN_POINT ( 'NONE',  ( 12.07500000122903039, 2.886751345948193936, 4.999999999999883649 ) ) ;
#59560 = CARTESIAN_POINT ( 'NONE',  ( 1.999999999999997335, 15.96874999877096535, 33.46410161513775705 ) ) ;
#59561 = DIRECTION ( 'NONE',  ( -0.000000000000000000, -1.000000000000000000, -0.000000000000000000 ) ) ;
#59562 = CARTESIAN_POINT ( 'NONE',  ( 3.455719506257207918, -3.613630455596491320, 3.583513068947109748 ) ) ;
#59563 = FACE_OUTER_BOUND ( 'NONE', #31992, .T. ) ;
#59564 = CARTESIAN_POINT ( 'NONE',  ( 15.87187500061451573, 3.027376345333611329, 5.243569643749999010 ) ) ;
#59565 = CARTESIAN_POINT ( 'NONE',  ( 28.76249999999999929, -5.773502691896255534, -1.060575238724906372E-15 ) ) ;
#59566 = CARTESIAN_POINT ( 'NONE',  ( 11.31562500061451892, 3.027376345333611329, 5.243569643749999010 ) ) ;
#59567 = CARTESIAN_POINT ( 'NONE',  ( 7.781250001229034652, 6.123233995736764310E-16, -4.999999999999998224 ) ) ;
#59568 = CARTESIAN_POINT ( 'NONE',  ( 23.22187500061451715, -6.054752690667223547, -1.112240025338166033E-15 ) ) ;
#59569 = CARTESIAN_POINT ( 'NONE',  ( 17.18437500061451573, -2.746126346562646425, 4.756430356249996549 ) ) ;
#59570 = AXIS2_PLACEMENT_3D ( 'NONE', #67904, #34264, #24274 ) ;
#59571 = CARTESIAN_POINT ( 'NONE',  ( 6.853125000614516793, 0.000000000000000000, 5.243569643749999010 ) ) ;
#59572 = CARTESIAN_POINT ( 'NONE',  ( 13.84687500061451537, -3.027376345333610441, -5.243569643749999898 ) ) ;
#59573 = ORIENTED_EDGE ( 'NONE', *, *, #68005, .T. ) ;
#59574 = CARTESIAN_POINT ( 'NONE',  ( 24.04687500061451644, -3.027376345333614438, 5.243569643749998122 ) ) ;
#59575 = CARTESIAN_POINT ( 'NONE',  ( 28.60312500061451502, -4.541064518000417216, -2.621784821875001281 ) ) ;
#59576 = CARTESIAN_POINT ( 'NONE',  ( 8.625000000000000000, 6.123233995736764310E-16, -4.999999999999998224 ) ) ;
#59577 = CARTESIAN_POINT ( 'NONE',  ( 7.462500000000001243, 2.886751345948126879, 4.999999999999999112 ) ) ;
#59578 = CARTESIAN_POINT ( 'NONE',  ( 17.36250000122903359, 4.330127018922192761, -2.499999999999997780 ) ) ;
#59579 = DIRECTION ( 'NONE',  ( -0.000000000000000000, -1.000000000000000000, -0.000000000000000000 ) ) ;
#59580 = DIRECTION ( 'NONE',  ( -0.000000000000000000, -1.000000000000000000, -0.000000000000000000 ) ) ;
#59581 = ORIENTED_EDGE ( 'NONE', *, *, #57650, .T. ) ;
#59582 = CARTESIAN_POINT ( 'NONE',  ( 16.27499999999999858, 6.123233995736764310E-16, -4.999999999999998224 ) ) ;
#59583 = CARTESIAN_POINT ( 'NONE',  ( 19.83750000000000213, -2.886751345948125991, -5.000000000000000000 ) ) ;
#59584 = CARTESIAN_POINT ( 'NONE',  ( 14.76562500061451821, 3.027376345333613106, -5.243569643749998122 ) ) ;
#59586 = ORIENTED_EDGE ( 'NONE', *, *, #19616, .F. ) ;
#59585 = VECTOR ( 'NONE', #54873, 1000.000000000000000 ) ;
#59587 = CARTESIAN_POINT ( 'NONE',  ( -3.999999999999999112, 16.68124999877096570, 27.69059892324149530 ) ) ;
#59588 = CARTESIAN_POINT ( 'NONE',  ( 4.243569643749999898, 17.34687500061451715, -27.54997392385601529 ) ) ;
#59589 = CARTESIAN_POINT ( 'NONE',  ( 4.115625000614516082, 3.027376345333611329, 5.243569643749999010 ) ) ;
#59590 = CARTESIAN_POINT ( 'NONE',  ( 12.52500000000000213, -4.330127018922194537, 2.499999999999995559 ) ) ;
#59591 = CARTESIAN_POINT ( 'NONE',  ( 27.83437500061451075, 5.492252693125287522, 3.363034840372157021E-16 ) ) ;
#59592 = ORIENTED_EDGE ( 'NONE', *, *, #8903, .F. ) ;
#59593 = CARTESIAN_POINT ( 'NONE',  ( -4.243569643749997233, 15.79062500061451857, 32.45002607614398471 ) ) ;
#59594 = CARTESIAN_POINT ( 'NONE',  ( 26.76562500061451644, -6.054752690667223547, -1.112240025338166033E-15 ) ) ;
#59595 = CARTESIAN_POINT ( 'NONE',  ( 8.287499999999999645, 5.773502691896255534, 3.535250795749688894E-16 ) ) ;
#59596 = AXIS2_PLACEMENT_3D ( 'NONE', #7201, #29730, #52268 ) ;
#59597 = CARTESIAN_POINT ( 'NONE',  ( 1.878215178125000495, 19.46562499938548640, 26.74683588394047007 ) ) ;
#59598 = CARTESIAN_POINT ( 'NONE',  ( 22.62187500061451573, 3.027376345333611329, 5.243569643749999010 ) ) ;
#59599 = CARTESIAN_POINT ( 'NONE',  ( 18.36562500061451431, 3.027376345333613106, -5.243569643749998122 ) ) ;
#59600 = CARTESIAN_POINT ( 'NONE',  ( 2.121784821875001281, 13.20312500061459460, -26.32496088578401938 ) ) ;
#59601 = CARTESIAN_POINT ( 'NONE',  ( 24.33750000122903145, -4.330127018922194537, 2.499999999999995559 ) ) ;
#59602 = CARTESIAN_POINT ( 'NONE',  ( 5.240625000614516971, -3.027376345333610441, -5.243569643749999898 ) ) ;
#59603 = CARTESIAN_POINT ( 'NONE',  ( 26.22187500061451715, 2.746126346562643317, 4.756430356249998326 ) ) ;
#59604 = CARTESIAN_POINT ( 'NONE',  ( 21.36562500061451075, -6.054752690667223547, -1.112240025338166033E-15 ) ) ;
#59605 = CARTESIAN_POINT ( 'NONE',  ( 9.534375000614517148, 4.119189519843966529, 2.378215178124999607 ) ) ;
#59606 = CARTESIAN_POINT ( 'NONE',  ( 1.878215178125000495, 16.76562499938548356, 26.74683588394047007 ) ) ;
#59607 = CARTESIAN_POINT ( 'NONE',  ( 18.49687500061452283, 6.054752690667223547, 3.707466751127219781E-16 ) ) ;
#59608 = CARTESIAN_POINT ( 'NONE',  ( 16.02187500061451786, -6.054752690667223547, -1.112240025338166033E-15 ) ) ;
#59609 = CARTESIAN_POINT ( 'NONE',  ( 25.62187500061451573, 3.027376345333613106, -5.243569643749998122 ) ) ;
#59610 = CARTESIAN_POINT ( 'NONE',  ( 4.243569643749999898, 15.09687500061451715, 32.45002607614398471 ) ) ;
#59611 = CARTESIAN_POINT ( 'NONE',  ( 5.390625000614518214, 6.054752690667223547, 3.707466751127219781E-16 ) ) ;
#59612 = CARTESIAN_POINT ( 'NONE',  ( 28.37812500061451715, 4.541064518000418104, 2.621784821874999949 ) ) ;
#59613 = CARTESIAN_POINT ( 'NONE',  ( 3.234375000614516438, 4.541064518000418104, 2.621784821874999949 ) ) ;
#59614 = CARTESIAN_POINT ( 'NONE',  ( -3.999999999999999112, 13.58750000000000213, 27.69059892324149530 ) ) ;
#59615 = CARTESIAN_POINT ( 'NONE',  ( 3.999999999999998668, 19.36250000000000426, 27.69059892324149175 ) ) ;
#59616 = CARTESIAN_POINT ( 'NONE',  ( 6.646875000614518747, -3.027376345333610441, -5.243569643749999898 ) ) ;
#59617 = CARTESIAN_POINT ( 'NONE',  ( 0.000000000000000000, 0.000000000000000000, 0.000000000000000000 ) ) ;
#59618 = CARTESIAN_POINT ( 'NONE',  ( 14.25000000122903465, 5.773502691896255534, 3.535250795749688894E-16 ) ) ;
#59619 = CARTESIAN_POINT ( 'NONE',  ( 8.887500001229033941, 4.330127018922191873, 2.499999999999999556 ) ) ;
#59620 = CARTESIAN_POINT ( 'NONE',  ( 3.928125000614516527, 6.421520780324663323E-16, -5.243569643749999010 ) ) ;
#59621 = CARTESIAN_POINT ( 'NONE',  ( 1.999999999999997335, 16.41874999877096641, 33.46410161513775705 ) ) ;
#59622 = CARTESIAN_POINT ( 'NONE',  ( 20.68125000122903145, -4.330127018922194537, 2.499999999999995559 ) ) ;
#59623 = CARTESIAN_POINT ( 'NONE',  ( 14.97187500061451892, 3.027376345333611329, 5.243569643749999010 ) ) ;
#59624 = CARTESIAN_POINT ( 'NONE',  ( 21.11250000000000071, -5.773502691896255534, -1.060575238724906372E-15 ) ) ;
#59625 = ORIENTED_EDGE ( 'NONE', *, *, #21830, .T. ) ;
#59626 = ADVANCED_FACE ( 'NONE', ( #57107 ), #19384, .T. ) ;
#59627 = CARTESIAN_POINT ( 'NONE',  ( 22.79062500061451502, -3.027376345333610441, -5.243569643749999898 ) ) ;
#59628 = CARTESIAN_POINT ( 'NONE',  ( 6.740625000614516082, 6.054752690667223547, 3.707466751127219781E-16 ) ) ;
#59629 = CARTESIAN_POINT ( 'NONE',  ( 25.05937500061451573, -4.541064518000417216, -2.621784821875001281 ) ) ;
#59630 = CARTESIAN_POINT ( 'NONE',  ( 8.015625000614518214, 3.027376345333613106, -5.243569643749998122 ) ) ;
#59631 = CARTESIAN_POINT ( 'NONE',  ( 23.26875000122903003, 2.886751345948126879, 4.999999999999998224 ) ) ;
#59632 = CARTESIAN_POINT ( 'NONE',  ( 8.175000001229031810, -5.773502691896255534, -1.060575238724906372E-15 ) ) ;
#59633 = CARTESIAN_POINT ( 'NONE',  ( 23.57812500061451289, -4.541064518000419881, 2.621784821874995952 ) ) ;
#59634 = CARTESIAN_POINT ( 'NONE',  ( -2.121784821874996840, 10.87812500061451715, -26.32496088578401583 ) ) ;
#59635 = CARTESIAN_POINT ( 'NONE',  ( 9.750000001229032875, 5.773502691896255534, 3.535250795749688894E-16 ) ) ;
#59636 = CARTESIAN_POINT ( 'NONE',  ( 19.45312500061451644, 0.000000000000000000, 5.243569643749999010 ) ) ;
#59637 = MECHANICAL_DESIGN_GEOMETRIC_PRESENTATION_REPRESENTATION (  '', ( #13649 ), #65557 ) ;
#59638 = CARTESIAN_POINT ( 'NONE',  ( 17.54062500061451502, 6.054752690667223547, 3.707466751127219781E-16 ) ) ;
#59639 = CARTESIAN_POINT ( 'NONE',  ( 28.58437500061451786, -4.119189519843968306, 2.378215178124996054 ) ) ;
#59640 = CARTESIAN_POINT ( 'NONE',  ( 17.17500000000000071, 6.123233995736764310E-16, -4.999999999999998224 ) ) ;
#59641 = CARTESIAN_POINT ( 'NONE',  ( 11.88750000122903216, 6.123233995736764310E-16, -4.999999999999998224 ) ) ;
#59642 = CARTESIAN_POINT ( 'NONE',  ( 8.015625000614518214, 3.027376345333613106, -5.243569643749998122 ) ) ;
#59643 = CARTESIAN_POINT ( 'NONE',  ( 12.40312500061451573, -4.541064518000417216, -2.621784821875001281 ) ) ;
#59644 =( BOUNDED_CURVE ( )  B_SPLINE_CURVE ( 2, ( #24498, #28963, #28601, #41146, #45957, #39701, #52219 ),
 .UNSPECIFIED., .F., .F. ) 
 B_SPLINE_CURVE_WITH_KNOTS ( ( 3, 2, 2, 3 ),
 ( 0.6999999999999999556, 0.7027777777777777235, 0.7055555555555557135, 0.7083333333333334814 ),
 .UNSPECIFIED. ) 
 CURVE ( )  GEOMETRIC_REPRESENTATION_ITEM ( )  RATIONAL_B_SPLINE_CURVE ( ( 1.000000000000000000, 0.8660254037844387076, 1.000000000000000000, 0.8660254037844387076, 1.000000000000000000, 0.8660254037844333785, 1.000000000000005329 ) ) 
 REPRESENTATION_ITEM ( '' )  );
#59645 = VECTOR ( 'NONE', #35957, 1000.000000000000000 ) ;
#59646 = CARTESIAN_POINT ( 'NONE',  ( 22.76250000122903216, 4.330127018922192761, -2.499999999999997780 ) ) ;
#59647 = AXIS2_PLACEMENT_3D ( 'NONE', #66998, #62166, #16360 ) ;
#59648 = CARTESIAN_POINT ( 'NONE',  ( 21.49687500061451573, -3.027376345333610441, -5.243569643749999898 ) ) ;
#59649 = DIRECTION ( 'NONE',  ( -1.000000000000000000, 0.000000000000000000, 0.000000000000000000 ) ) ;
#59650 = CARTESIAN_POINT ( 'NONE',  ( 5.362500001229033586, 0.000000000000000000, 4.999999999999998224 ) ) ;
#59651 = CARTESIAN_POINT ( 'NONE',  ( 6.234375000614519102, 6.421520780324663323E-16, -5.243569643749999010 ) ) ;
#59652 = CARTESIAN_POINT ( 'NONE',  ( 22.35937500061451644, -4.541064518000417216, -2.621784821875001281 ) ) ;
#59653 = ADVANCED_FACE ( 'NONE', ( #35305 ), #24939, .F. ) ;
#59654 = CARTESIAN_POINT ( 'NONE',  ( -3.486133158594716510E-16, 12.61250000000000426, 26.00000000000000355 ) ) ;
#59655 = CARTESIAN_POINT ( 'NONE',  ( 19.90312500061451573, 0.000000000000000000, 5.243569643749999010 ) ) ;
#59656 = CARTESIAN_POINT ( 'NONE',  ( 23.52187500061451786, 3.027376345333611329, 5.243569643749999010 ) ) ;
#59657 = CARTESIAN_POINT ( 'NONE',  ( 1.878215178124997609, 19.87812499938548072, 33.25316411605952993 ) ) ;
#59658 = DIRECTION ( 'NONE',  ( -1.000000000000000000, -0.000000000000000000, -0.000000000000000000 ) ) ;
#59659 = CARTESIAN_POINT ( 'NONE',  ( 27.78750000122903074, 4.330127018922191873, 2.499999999999999556 ) ) ;
#59660 = CARTESIAN_POINT ( 'NONE',  ( 6.309375000614517504, 4.541064518000418104, -2.621784821874998173 ) ) ;
#59661 = CARTESIAN_POINT ( 'NONE',  ( 16.11562500061451786, 3.027376345333613106, -5.243569643749998122 ) ) ;
#59662 = CARTESIAN_POINT ( 'NONE',  ( 13.73437500061451821, -4.541064518000419881, 2.621784821874995952 ) ) ;
#59663 = ORIENTED_EDGE ( 'NONE', *, *, #1636, .F. ) ;
#59664 = CARTESIAN_POINT ( 'NONE',  ( 10.48125000122903216, 6.123233995736764310E-16, -4.999999999999998224 ) ) ;
#59665 = CARTESIAN_POINT ( 'NONE',  ( 25.15312500061451217, 4.541064518000418104, -2.621784821874998173 ) ) ;
#59666 = CARTESIAN_POINT ( 'NONE',  ( 3.242103837493086330E-14, 13.13749999999999929, -34.00000000000000000 ) ) ;
#59667 = CYLINDRICAL_SURFACE ( 'NONE', #27782, 3.999999999999996447 ) ;
#59668 = CARTESIAN_POINT ( 'NONE',  ( 13.57500000000000107, 6.123233995736764310E-16, -4.999999999999998224 ) ) ;
#59669 = CARTESIAN_POINT ( 'NONE',  ( 24.71250000122903145, 0.000000000000000000, 4.999999999999998224 ) ) ;
#59670 = CARTESIAN_POINT ( 'NONE',  ( 17.65312500061451573, 0.000000000000000000, 5.243569643749999010 ) ) ;
#59671 = ORIENTED_EDGE ( 'NONE', *, *, #13387, .F. ) ;
#59672 = CARTESIAN_POINT ( 'NONE',  ( 21.75000000000000000, 4.330127018922192761, -2.499999999999997780 ) ) ;
#59673 = CARTESIAN_POINT ( 'NONE',  ( 23.14687500061451786, -3.027376345333614438, 5.243569643749998122 ) ) ;
#59674 = ORIENTED_EDGE ( 'NONE', *, *, #16952, .T. ) ;
#59675 = CARTESIAN_POINT ( 'NONE',  ( 1.626862140677534273E-15, 17.52500000122903145, -26.00000000000000355 ) ) ;
#59676 = CARTESIAN_POINT ( 'NONE',  ( 13.11562500061451786, 3.027376345333611329, 5.243569643749999010 ) ) ;
#59677 = CARTESIAN_POINT ( 'NONE',  ( 4.640625000614518214, -3.027376345333614438, 5.243569643749998122 ) ) ;
#59678 = CARTESIAN_POINT ( 'NONE',  ( 15.79687500061451644, 0.000000000000000000, 4.756430356249998326 ) ) ;
#59679 = CARTESIAN_POINT ( 'NONE',  ( 26.01562500061451289, 3.027376345333613106, -5.243569643749998122 ) ) ;
#59680 = VECTOR ( 'NONE', #48110, 1000.000000000000000 ) ;
#59681 = CARTESIAN_POINT ( 'NONE',  ( 18.86249999999999716, -5.773502691896255534, -1.060575238724906372E-15 ) ) ;
#59682 = CARTESIAN_POINT ( 'NONE',  ( 27.44999999999999929, -4.330127018922190985, -2.500000000000001332 ) ) ;
#59683 = LINE ( 'NONE', #71143, #29751 ) ;
#59684 = CARTESIAN_POINT ( 'NONE',  ( 7.321875000614516793, 3.027376345333611329, 5.243569643749999010 ) ) ;
#59685 = CARTESIAN_POINT ( 'NONE',  ( 17.82187500061451502, -6.054752690667223547, -1.112240025338166033E-15 ) ) ;
#59686 = FACE_OUTER_BOUND ( 'NONE', #34877, .T. ) ;
#59687 = VERTEX_POINT ( 'NONE', #13858 ) ;
#59688 = CARTESIAN_POINT ( 'NONE',  ( 27.25312500061451360, -4.541064518000417216, -2.621784821875001281 ) ) ;
#59689 = CARTESIAN_POINT ( 'NONE',  ( 28.17187500061451644, -6.054752690667223547, -1.112240025338166033E-15 ) ) ;
#59690 = DIRECTION ( 'NONE',  ( 0.000000000000000000, -0.000000000000000000, -1.000000000000000000 ) ) ;
#59691 = CARTESIAN_POINT ( 'NONE',  ( 15.93750000000000000, 5.773502691896255534, 3.535250795749688894E-16 ) ) ;
#59692 = CARTESIAN_POINT ( 'NONE',  ( 10.79062500061451679, 6.054752690667223547, 3.707466751127219781E-16 ) ) ;
#59693 = CARTESIAN_POINT ( 'NONE',  ( 25.93125000122903145, 4.330127018922191873, 2.499999999999999556 ) ) ;
#59694 = CARTESIAN_POINT ( 'NONE',  ( -4.000000000000000000, 18.06874999877096855, 30.00000000000000000 ) ) ;
#59695 = CARTESIAN_POINT ( 'NONE',  ( 28.82812500061451644, 4.541064518000418104, 2.621784821874999949 ) ) ;
#59696 = CARTESIAN_POINT ( 'NONE',  ( 17.40000000122903145, 5.773502691896255534, 3.535250795749688894E-16 ) ) ;
#59697 = DIRECTION ( 'NONE',  ( -0.000000000000000000, -0.000000000000000000, -1.000000000000000000 ) ) ;
#59698 = CARTESIAN_POINT ( 'NONE',  ( 18.08437500061451431, 4.119189519843966529, 2.378215178124999607 ) ) ;
#59699 = CARTESIAN_POINT ( 'NONE',  ( 5.615625000614517859, -6.054752690667223547, -1.112240025338166033E-15 ) ) ;
#59700 = CARTESIAN_POINT ( 'NONE',  ( 22.35937500061451644, -4.541064518000417216, -2.621784821875001281 ) ) ;
#59701 = CARTESIAN_POINT ( 'NONE',  ( 4.243569643749999010, 16.07187500061451857, 27.54997392385601174 ) ) ;
#59702 = CARTESIAN_POINT ( 'NONE',  ( 23.97187500061451360, 3.027376345333611329, 5.243569643749999010 ) ) ;
#59703 = CARTESIAN_POINT ( 'NONE',  ( 3.937500000000000444, -2.886751345948129988, 4.999999999999997335 ) ) ;
#59704 = CARTESIAN_POINT ( 'NONE',  ( 4.000000000000000000, 9.950000001229035718, 32.30940107675849049 ) ) ;
#59705 = CARTESIAN_POINT ( 'NONE',  ( 11.12812500061451715, 6.421520780324663323E-16, -5.243569643749999010 ) ) ;
#59706 = CARTESIAN_POINT ( 'NONE',  ( 3.225000001229033408, -5.773502691896255534, -1.060575238724906372E-15 ) ) ;
#59707 = CARTESIAN_POINT ( 'NONE',  ( 10.58437500061451964, -4.541064518000419881, 2.621784821874995952 ) ) ;
#59708 = CARTESIAN_POINT ( 'NONE',  ( -2.556497649636125342E-15, 18.87500000122903288, 34.00000000000000000 ) ) ;
#59709 = CARTESIAN_POINT ( 'NONE',  ( 9.740625000614516082, -3.027376345333610441, -5.243569643749999898 ) ) ;
#59710 = CARTESIAN_POINT ( 'NONE',  ( 13.35937500061451821, -4.541064518000417216, -2.621784821875001281 ) ) ;
#59711 = CARTESIAN_POINT ( 'NONE',  ( 25.50000000000000000, 0.000000000000000000, 4.999999999999998224 ) ) ;
#59712 = CARTESIAN_POINT ( 'NONE',  ( 22.16250000122903074, -4.330127018922190985, -2.500000000000001332 ) ) ;
#59713 = CARTESIAN_POINT ( 'NONE',  ( 9.234375000614518214, -4.541064518000419881, 2.621784821874995952 ) ) ;
#59714 = CARTESIAN_POINT ( 'NONE',  ( 12.06562500061451537, 3.027376345333613106, -5.243569643749998122 ) ) ;
#59715 = CARTESIAN_POINT ( 'NONE',  ( 28.93125000122903145, 6.123233995736764310E-16, -4.999999999999998224 ) ) ;
#59716 = CARTESIAN_POINT ( 'NONE',  ( 22.39687500061451075, -3.027376345333610441, -5.243569643749999898 ) ) ;
#59717 = DIRECTION ( 'NONE',  ( -1.000000000000000000, -0.000000000000000000, -0.000000000000000000 ) ) ;
#59718 = CARTESIAN_POINT ( 'NONE',  ( -3.999999999999999112, 11.97500000122903430, -32.30940107675850470 ) ) ;
#59719 = CARTESIAN_POINT ( 'NONE',  ( 8.400000000000000355, 0.000000000000000000, 4.999999999999998224 ) ) ;
#59720 = CARTESIAN_POINT ( 'NONE',  ( 2.121784821874999061, 13.40937500061451892, -33.67503911421598417 ) ) ;
#59721 = CARTESIAN_POINT ( 'NONE',  ( 14.66250000122903252, 4.330127018922192761, -2.499999999999997780 ) ) ;
#59722 = CARTESIAN_POINT ( 'NONE',  ( 9.571875000614518569, 3.027376345333611329, 5.243569643749999010 ) ) ;
#59723 = CARTESIAN_POINT ( 'NONE',  ( 9.001249775931846008E-16, 17.66562500061451502, -25.09994784771203058 ) ) ;
#59724 = CARTESIAN_POINT ( 'NONE',  ( 18.48750000122903359, -4.330127018922194537, 2.499999999999995559 ) ) ;
#59725 = CARTESIAN_POINT ( 'NONE',  ( 12.40312500061451573, -4.541064518000417216, -2.621784821875001281 ) ) ;
#59726 = VERTEX_POINT ( 'NONE', #54129 ) ;
#59727 = CARTESIAN_POINT ( 'NONE',  ( 16.64999999999999858, -4.330127018922190985, -2.500000000000001332 ) ) ;
#59728 = CARTESIAN_POINT ( 'NONE',  ( 7.320879633048903241E-15, 17.30000000122903003, -34.00000000000000000 ) ) ;
#59729 = CARTESIAN_POINT ( 'NONE',  ( 9.834375000614517859, 6.421520780324663323E-16, -5.243569643749999010 ) ) ;
#59730 = CARTESIAN_POINT ( 'NONE',  ( -3.999999999999997335, 14.30000000122903359, 32.30940107675850470 ) ) ;
#59731 = CARTESIAN_POINT ( 'NONE',  ( 12.33750000122903145, 6.123233995736764310E-16, -4.999999999999998224 ) ) ;
#59732 = CARTESIAN_POINT ( 'NONE',  ( 19.87500000122903288, -5.773502691896255534, -1.060575238724906372E-15 ) ) ;
#59733 = CARTESIAN_POINT ( 'NONE',  ( 17.01562500061451644, 3.027376345333613106, -5.243569643749998122 ) ) ;
#59734 = CARTESIAN_POINT ( 'NONE',  ( 21.40312500061451573, -4.541064518000417216, -2.621784821875001281 ) ) ;
#59735 = CARTESIAN_POINT ( 'NONE',  ( 28.31250000122903288, 0.000000000000000000, 4.999999999999998224 ) ) ;
#59736 = CARTESIAN_POINT ( 'NONE',  ( 3.178125000614515638, 4.541064518000418104, 2.621784821874999949 ) ) ;
#59737 = CARTESIAN_POINT ( 'NONE',  ( 26.09999999999999787, -4.330127018922190985, -2.500000000000001332 ) ) ;
#59738 = CARTESIAN_POINT ( 'NONE',  ( 30.00000000000000000, 0.000000000000000000, 0.000000000000000000 ) ) ;
#59739 = VECTOR ( 'NONE', #29205, 1000.000000000000000 ) ;
#59740 = CARTESIAN_POINT ( 'NONE',  ( 29.02499999999999858, 4.330127018922191873, 2.499999999999999556 ) ) ;
#59741 = CARTESIAN_POINT ( 'NONE',  ( 28.17187500061451644, -6.054752690667223547, -1.112240025338166033E-15 ) ) ;
#59742 = CARTESIAN_POINT ( 'NONE',  ( -5.810221930991193690E-16, 15.50000000122903465, -34.00000000000000000 ) ) ;
#59743 = CARTESIAN_POINT ( 'NONE',  ( 3.637500001229036162, -4.330127018922194537, 2.499999999999995559 ) ) ;
#59744 = CARTESIAN_POINT ( 'NONE',  ( 29.74687500061451217, 6.054752690667223547, 3.707466751127219781E-16 ) ) ;
#59745 = EDGE_CURVE ( 'NONE', #4778, #67289, #5029, .T. ) ;
#59746 = DIRECTION ( 'NONE',  ( -0.000000000000000000, -1.000000000000000000, -0.000000000000000000 ) ) ;
#59747 = CARTESIAN_POINT ( 'NONE',  ( 8.596875000614518925, 6.054752690667223547, 3.707466751127219781E-16 ) ) ;
#59748 = CARTESIAN_POINT ( 'NONE',  ( 26.91562500061451146, 3.027376345333613106, -5.243569643749998122 ) ) ;
#59749 = CARTESIAN_POINT ( 'NONE',  ( 4.683223236373093457, -1.751405183929441556, 4.942428804804532838 ) ) ;
#59750 = CARTESIAN_POINT ( 'NONE',  ( 11.62500000122903465, 2.886751345948126879, 4.999999999999998224 ) ) ;
#59751 = CARTESIAN_POINT ( 'NONE',  ( -1.071796769724480347, 16.86740381056766580, 34.00000000000000711 ) ) ;
#59752 = CARTESIAN_POINT ( 'NONE',  ( 4.546875000614517326, 6.054752690667223547, 3.707466751127219781E-16 ) ) ;
#59753 = CARTESIAN_POINT ( 'NONE',  ( 9.684375000614517504, -4.541064518000419881, 2.621784821874995952 ) ) ;
#59754 = CARTESIAN_POINT ( 'NONE',  ( 5.287500000000000533, -2.886751345948129988, 4.999999999999997335 ) ) ;
#59755 = CARTESIAN_POINT ( 'NONE',  ( -2.121784821874996840, 11.32812500061459282, 33.67503911421598417 ) ) ;
#59756 = CARTESIAN_POINT ( 'NONE',  ( 22.38749999999999929, -2.886751345948129988, 4.999999999999997335 ) ) ;
#59757 = CARTESIAN_POINT ( 'NONE',  ( 20.85000000122903430, -2.886751345948126435, -5.000000000000000000 ) ) ;
#59758 = CARTESIAN_POINT ( 'NONE',  ( 4.724999999999999645, 4.330127018922191873, 2.499999999999999556 ) ) ;
#59759 = CARTESIAN_POINT ( 'NONE',  ( 15.42187500061451466, -4.119189519843968306, 2.378215178124996054 ) ) ;
#59760 = ORIENTED_EDGE ( 'NONE', *, *, #6118, .F. ) ;
#59761 = CARTESIAN_POINT ( 'NONE',  ( 19.15312500061451573, -4.541064518000417216, -2.621784821875001281 ) ) ;
#59762 = CARTESIAN_POINT ( 'NONE',  ( 9.778125000614517504, 6.421520780324663323E-16, -5.243569643749999010 ) ) ;
#59763 = CARTESIAN_POINT ( 'NONE',  ( 24.94687500061451502, -4.119189519843965641, -2.378215178125001383 ) ) ;
#59764 = CARTESIAN_POINT ( 'NONE',  ( 6.271875000614517859, 3.027376345333613106, -5.243569643749998122 ) ) ;
#59765 = CARTESIAN_POINT ( 'NONE',  ( 23.43750000000000000, -2.886751345948125991, -5.000000000000000000 ) ) ;
#59766 = CARTESIAN_POINT ( 'NONE',  ( 19.91250000122903074, -4.330127018922190985, -2.500000000000001332 ) ) ;
#59767 = CARTESIAN_POINT ( 'NONE',  ( 27.66562500061451146, -6.054752690667223547, -1.112240025338166033E-15 ) ) ;
#59768 = CARTESIAN_POINT ( 'NONE',  ( 30.00000000000000000, 0.000000000000000000, 0.000000000000000000 ) ) ;
#59769 = CARTESIAN_POINT ( 'NONE',  ( 8.934375000614517504, 6.421520780324663323E-16, -5.243569643749999010 ) ) ;
#59770 = CARTESIAN_POINT ( 'NONE',  ( 14.93437500061451750, 4.541064518000418104, 2.621784821874999949 ) ) ;
#59771 = CARTESIAN_POINT ( 'NONE',  ( 25.09687500061451715, -3.027376345333610441, -5.243569643749999898 ) ) ;
#59772 = AXIS2_PLACEMENT_3D ( 'NONE', #62011, #16934, #55387 ) ;
#59773 = FACE_OUTER_BOUND ( 'NONE', #67065, .T. ) ;
#59774 = CARTESIAN_POINT ( 'NONE',  ( 12.63749999999999929, -2.886751345948125991, -5.000000000000000000 ) ) ;
#59775 = CARTESIAN_POINT ( 'NONE',  ( 19.50937500061451857, 0.000000000000000000, 5.243569643749999010 ) ) ;
#59776 = CARTESIAN_POINT ( 'NONE',  ( 9.646875000614516082, -3.027376345333614438, 5.243569643749998122 ) ) ;
#59777 = CARTESIAN_POINT ( 'NONE',  ( -3.756430356250001434, 20.21562499938548285, 32.16877607737301048 ) ) ;
#59778 = CARTESIAN_POINT ( 'NONE',  ( 24.26249999999999929, -5.773502691896255534, -1.060575238724906372E-15 ) ) ;
#59779 = CARTESIAN_POINT ( 'NONE',  ( -8.484601909799255319E-16, 15.53749999999999964, 34.61880215351700940 ) ) ;
#59780 = CARTESIAN_POINT ( 'NONE',  ( -2.121784821874999949, 10.78437500061451715, -33.67503911421598417 ) ) ;
#59781 = CARTESIAN_POINT ( 'NONE',  ( 24.38437500061451502, 4.119189519843966529, 2.378215178124999607 ) ) ;
#59782 = CARTESIAN_POINT ( 'NONE',  ( 12.10312500061451857, 4.541064518000418104, -2.621784821874998173 ) ) ;
#59783 = CARTESIAN_POINT ( 'NONE',  ( 5.512499999999999289, 2.886751345948129099, -4.999999999999998224 ) ) ;
#59784 = PRESENTATION_STYLE_ASSIGNMENT (( #42807 ) ) ;
#59785 = FACE_OUTER_BOUND ( 'NONE', #69668, .T. ) ;
#59786 = CARTESIAN_POINT ( 'NONE',  ( 11.81250000000000000, 2.886751345948129099, -4.999999999999998224 ) ) ;
#59787 = CARTESIAN_POINT ( 'NONE',  ( -1.999999999999997113, 17.03750000122903430, 33.46410161513775705 ) ) ;
#59788 = CARTESIAN_POINT ( 'NONE',  ( 11.81250000122903465, -4.330127018922190985, -2.500000000000001332 ) ) ;
#59789 = CARTESIAN_POINT ( 'NONE',  ( 23.14687500061451786, -3.027376345333614438, 5.243569643749998122 ) ) ;
#59790 = CARTESIAN_POINT ( 'NONE',  ( 16.77187500061451786, 3.027376345333611329, 5.243569643749999010 ) ) ;
#59791 = CARTESIAN_POINT ( 'NONE',  ( 7.293750001229029500, -2.886751345948237457, -4.999999999999807265 ) ) ;
#59792 = ORIENTED_EDGE ( 'NONE', *, *, #55458, .T. ) ;
#59793 = CARTESIAN_POINT ( 'NONE',  ( 17.31562500061451715, -6.054752690667223547, -1.112240025338166033E-15 ) ) ;
#59794 = CARTESIAN_POINT ( 'NONE',  ( 29.36250000122903003, -4.330127018922190985, -2.500000000000001332 ) ) ;
#59795 = CARTESIAN_POINT ( 'NONE',  ( 18.68437500061451928, -4.541064518000419881, 2.621784821874995952 ) ) ;
#59796 = CARTESIAN_POINT ( 'NONE',  ( 28.92187500061451644, 3.027376345333611329, 5.243569643749999010 ) ) ;
#59797 = CARTESIAN_POINT ( 'NONE',  ( 3.815625000614518036, -6.054752690667223547, -1.112240025338166033E-15 ) ) ;
#59798 = CARTESIAN_POINT ( 'NONE',  ( 19.00312500061451715, 0.000000000000000000, 5.243569643749999010 ) ) ;
#59799 = CARTESIAN_POINT ( 'NONE',  ( 28.24687500061451573, -3.027376345333610441, -5.243569643749999898 ) ) ;
#59800 = CARTESIAN_POINT ( 'NONE',  ( 4.243569643749999010, 13.76562500061451644, 27.54997392385601174 ) ) ;
#59801 = CARTESIAN_POINT ( 'NONE',  ( 16.35000000122903430, -2.886751345948125991, -5.000000000000000000 ) ) ;
#59802 = CARTESIAN_POINT ( 'NONE',  ( 9.234375000614518214, -4.119189519843968306, 2.378215178124996054 ) ) ;
#59803 = CARTESIAN_POINT ( 'NONE',  ( 6.440625000614517148, -3.027376345333614438, 5.243569643749998122 ) ) ;
#59804 = CARTESIAN_POINT ( 'NONE',  ( 25.86562500061451431, -6.054752690667223547, -1.112240025338166033E-15 ) ) ;
#59805 = CARTESIAN_POINT ( 'NONE',  ( 8.887499999999997513, -2.886751345948063374, 5.000000000000112799 ) ) ;
#59806 =( BOUNDED_CURVE ( )  B_SPLINE_CURVE ( 2, ( #38653, #22731, #71905, #32370, #9841, #49739, #4674, #22375, #27933, #66357, #33825, #27204, #10207, #39018, #50823, #26841, #10931, #33100, #16460, #56002, #66732, #56368, #39751, #67463, #49375, #44927, #5759, #16826, #39380, #61899, #11304, #22016, #50102, #28292, #32742, #61533, #44572, #226, #45284, #43832, #21278, #10572, #67818, #15734, #17191, #54908, #4316, #38273, #55279, #72266, #21644, #44201, #16103, #61177, #55639, #57437, #28646, #6840, #47088, #69621, #951, #69264, #18626, #41191, #7199, #34541, #63700, #18983, #29728, #12374, #29013, #62268, #45650, #2032, #51184, #51550, #588, #68184, #23093, #40830, #6478, #24177, #17902, #52627, #62623, #23815, #11663, #34179, #6115, #29375, #62978, #56714, #23459, #17547, #40462, #24543, #40108, #12018, #57071, #46005, #68541, #34909, #13091, #51907, #1306, #58150, #46366, #35629, #68900, #18257, #52266, #63346, #1668, #7555, #12732, #46729, #35268, #57790, #30089, #26010, #25266, #14185, #13822, #37086, #48549, #71076, #58510, #59610, #20080, #7921, #71447, #36362, #41905, #70705, #26377, #47446, #53722, #69978, #30816, #59979, #35992, #20451, #41544, #48916, #30458, #8650, #42271, #64062, #58876, #52987, #70343, #54456, #2383, #13443, #24901, #8286, #53349, #31555, #9024, #19348, #65532, #37460, #64430, #43001, #2747, #47813, #54095, #19719, #3492, #14918, #64794, #9389, #65160, #48181, #31920, #3855, #36720, #25644, #59241, #31179, #42636, #3114, #14550, #38562, #44110, #15281, #10842, #71817, #4223, #66636, #38929, #32283, #49649, #54817, #21189, #44482, #65901, #10483, #10120, #72176, #16014, #49284, #72538, #20822, #27481, #37821, #55551, #21926, #4947, #33012, #61085, #50014, #21556, #4586, #67013, #26751, #16374, #27116, #61448, #43377, #43740, #32650, #60340, #9749, #55191, #66265, #15642, #38183, #60707, #70207, #36227, #31420, #48052, #31788, #70945, #26245, #8887, #53213, #53960, #71680, #21054, #20316, #42870, #25879, #54327, #59110, #15145, #43605, #3718, #36954, #53583, #13683, #19582, #26614, #2609, #2979, #25131, #42138, #47672, #65392, #31045, #48782, #42505, #4084, #14049, #48418, #37325, #64664, #8516 ),
 .UNSPECIFIED., .F., .F. ) 
 B_SPLINE_CURVE_WITH_KNOTS ( ( 3, 2, 2, 2, 2, 2, 2, 2, 2, 2, 2, 2, 2, 2, 2, 2, 2, 2, 2, 2, 2, 2, 2, 2, 2, 2, 2, 2, 2, 2, 2, 2, 2, 2, 2, 2, 2, 2, 2, 2, 2, 2, 2, 2, 2, 2, 2, 2, 2, 2, 2, 2, 2, 2, 2, 2, 2, 2, 2, 2, 2, 2, 2, 2, 2, 2, 2, 2, 2, 2, 2, 2, 2, 2, 2, 2, 2, 2, 2, 2, 2, 2, 2, 2, 2, 2, 2, 2, 2, 2, 2, 2, 2, 2, 2, 2, 2, 2, 2, 2, 2, 2, 2, 2, 2, 2, 2, 2, 2, 2, 2, 2, 2, 2, 2, 2, 2, 2, 2, 2, 2, 2, 2, 2, 2, 2, 2, 2, 2, 2, 2, 2, 2, 2, 3 ),
 ( 0.000000000000000000, 0.007499808062934601276, 0.01499961612586920255, 0.02249942418880380296, 0.02999923225173840510, 0.03749904031467300725, 0.04499884837760760592, 0.05249865644054221153, 0.05999846450347681021, 0.06749827256641140194, 0.07499808062934601449, 0.08249788869228059929, 0.08999769675521521184, 0.09749750481814981051, 0.1049973128810844231, 0.1124971209440190079, 0.1199969290069536204, 0.1274967370698882330, 0.1349965451328228039, 0.1424963531957574303, 0.1499961612586920290, 0.1574959693216266277, 0.1649957773845611986, 0.1724955854474958250, 0.1799953935104304237, 0.1874952015733650224, 0.1949950096362996210, 0.2024948176992342197, 0.2099946257621688461, 0.2174944338251034170, 0.2249942418880380157, 0.2324940499509726144, 0.2399938580139072408, 0.2474936660768418395, 0.2549934741397764659, 0.2624932822027110646, 0.2699930902656456078, 0.2774928983285802619, 0.2849927063915148606, 0.2924925144544494038, 0.2999923225173840580, 0.3074921305803186011, 0.3149919386432532553, 0.3224917467061878540, 0.3299915547691223972, 0.3374913628320570513, 0.3449911708949916500, 0.3524909789579262487, 0.3599907870208608474, 0.3674905950837954460, 0.3749904031467300447, 0.3824902112096646434, 0.3899900192725992421, 0.3974898273355338407, 0.4049896353984684394, 0.4124894434614030381, 0.4199892515243376923, 0.4274890595872722354, 0.4349888676502068341, 0.4424886757131414883, 0.4499884837760760314, 0.4574882918390106856, 0.4649880999019452288, 0.4724879079648798275, 0.4799877160278144816, 0.4874875240907490248, 0.4949873321536836790, 0.5024871402166182222, 0.5099869482795529319, 0.5174867563424874195, 0.5249865644054221292, 0.5324863724683566168, 0.5399861805312912155, 0.5474859885942259252, 0.5549857966571605239, 0.5624856047200950115, 0.5699854127830297212, 0.5774852208459643199, 0.5849850289088988076, 0.5924848369718334062, 0.5999846450347681159, 0.6074844530977027146, 0.6149842611606372023, 0.6224840692235719120, 0.6299838772865065106, 0.6374836853494409983, 0.6449834934123757080, 0.6524833014753103066, 0.6599831095382447943, 0.6674829176011795040, 0.6749827256641141027, 0.6824825337270487013, 0.6899823417899833000, 0.6974821498529178987, 0.7049819579158524974, 0.7124817659787869850, 0.7199815740417216947, 0.7274813821046562934, 0.7349811901675908921, 0.7424809982305254907, 0.7499808062934600894, 0.7574806143563946881, 0.7649804224193292868, 0.7724802304822638854, 0.7799800385451984841, 0.7874798466081331938, 0.7949796546710676814, 0.8024794627340022801, 0.8099792707969368788, 0.8174790788598714775, 0.8249788869228060761, 0.8324786949857406748, 0.8399785030486753845, 0.8474783111116098722, 0.8549781191745444708, 0.8624779272374791805, 0.8699777353004136682, 0.8774775433633482669, 0.8849773514262829766, 0.8924771594892175752, 0.8999769675521520629, 0.9074767756150867726, 0.9149765836780213712, 0.9224763917409558589, 0.9299761998038904576, 0.9374760078668251673, 0.9449758159297596549, 0.9524756239926942536, 0.9599754320556289633, 0.9674752401185635620, 0.9749750481814980496, 0.9824748562444327593, 0.9899746643073673580, 0.9974744723703018456, 1.000000000000000000 ),
 .UNSPECIFIED. ) 
 CURVE ( )  GEOMETRIC_REPRESENTATION_ITEM ( )  RATIONAL_B_SPLINE_CURVE ( ( 1.000000000000000000, 0.8660254037844387076, 1.000000000000000000, 0.8660254037844387076, 1.000000000000000000, 0.8660254037844387076, 1.000000000000000000, 0.8660254037844387076, 1.000000000000000000, 0.8660254037844387076, 1.000000000000000000, 0.8660254037844387076, 1.000000000000000000, 0.8660254037844387076, 1.000000000000000000, 0.8660254037844387076, 1.000000000000000000, 0.8660254037844387076, 1.000000000000000000, 0.8660254037844387076, 1.000000000000000000, 0.8660254037844387076, 1.000000000000000000, 0.8660254037844387076, 1.000000000000000000, 0.8660254037844387076, 1.000000000000000000, 0.8660254037844387076, 1.000000000000000000, 0.8660254037844387076, 1.000000000000000000, 0.8660254037844387076, 1.000000000000000000, 0.8660254037844387076, 1.000000000000000000, 0.8660254037844387076, 1.000000000000000000, 0.8660254037844387076, 1.000000000000000000, 0.8660254037844387076, 1.000000000000000000, 0.8660254037844387076, 1.000000000000000000, 0.8660254037844387076, 1.000000000000000000, 0.8660254037844387076, 1.000000000000000000, 0.8660254037844387076, 1.000000000000000000, 0.8660254037844387076, 1.000000000000000000, 0.8660254037844387076, 1.000000000000000000, 0.8660254037844387076, 1.000000000000000000, 0.8660254037844387076, 1.000000000000000000, 0.8660254037844387076, 1.000000000000000000, 0.8660254037844387076, 1.000000000000000000, 0.8660254037844387076, 1.000000000000000000, 0.8660254037844387076, 1.000000000000000000, 0.8660254037844387076, 1.000000000000000000, 0.8660254037844387076, 1.000000000000000000, 0.8660254037844387076, 1.000000000000000000, 0.8660254037844387076, 1.000000000000000000, 0.8660254037844387076, 1.000000000000000000, 0.8660254037844387076, 1.000000000000000000, 0.8660254037844387076, 1.000000000000000000, 0.8660254037844387076, 1.000000000000000000, 0.8660254037844387076, 1.000000000000000000, 0.8660254037844387076, 1.000000000000000000, 0.8660254037844387076, 1.000000000000000000, 0.8660254037844387076, 1.000000000000000000, 0.8660254037844387076, 1.000000000000000000, 0.8660254037844387076, 1.000000000000000000, 0.8660254037844387076, 1.000000000000000000, 0.8660254037844387076, 1.000000000000000000, 0.8660254037844387076, 1.000000000000000000, 0.8660254037844387076, 1.000000000000000000, 0.8660254037844387076, 1.000000000000000000, 0.8660254037844387076, 1.000000000000000000, 0.8660254037844387076, 1.000000000000000000, 0.8660254037844387076, 1.000000000000000000, 0.8660254037844387076, 1.000000000000000000, 0.8660254037844387076, 1.000000000000000000, 0.8660254037844387076, 1.000000000000000000, 0.8660254037844387076, 1.000000000000000000, 0.8660254037844387076, 1.000000000000000000, 0.8660254037844387076, 1.000000000000000000, 0.8660254037844387076, 1.000000000000000000, 0.8660254037844387076, 1.000000000000000000, 0.8660254037844387076, 1.000000000000000000, 0.8660254037844387076, 1.000000000000000000, 0.8660254037844387076, 1.000000000000000000, 0.8660254037844387076, 1.000000000000000000, 0.8660254037844387076, 1.000000000000000000, 0.8660254037844387076, 1.000000000000000000, 0.8660254037844387076, 1.000000000000000000, 0.8660254037844387076, 1.000000000000000000, 0.8660254037844387076, 1.000000000000000000, 0.8660254037844387076, 1.000000000000000000, 0.8660254037844387076, 1.000000000000000000, 0.8660254037844387076, 1.000000000000000000, 0.8660254037844387076, 1.000000000000000000, 0.8660254037844387076, 1.000000000000000000, 0.8660254037844387076, 1.000000000000000000, 0.8660254037844387076, 1.000000000000000000, 0.8660254037844387076, 1.000000000000000000, 0.8660254037844387076, 1.000000000000000000, 0.8660254037844387076, 1.000000000000000000, 0.8660254037844387076, 1.000000000000000000, 0.8660254037844387076, 1.000000000000000000, 0.8660254037844387076, 1.000000000000000000, 0.8660254037844387076, 1.000000000000000000, 0.8660254037844387076, 1.000000000000000000, 0.8660254037844387076, 1.000000000000000000, 0.8660254037844387076, 1.000000000000000000, 0.8660254037844387076, 1.000000000000000000, 0.8660254037844387076, 1.000000000000000000, 0.8660254037844387076, 1.000000000000000000, 0.8660254037844387076, 1.000000000000000000, 0.8660254037844387076, 1.000000000000000000, 0.8660254037844387076, 1.000000000000000000, 0.8660254037844387076, 1.000000000000000000, 0.8660254037844387076, 1.000000000000000000, 0.8660254037844387076, 1.000000000000000000, 0.8660254037844387076, 1.000000000000000000, 0.8660254037844387076, 1.000000000000000000, 0.8660254037844387076, 1.000000000000000000, 0.8660254037844387076, 1.000000000000000000, 0.8660254037844387076, 1.000000000000000000, 0.8660254037844387076, 1.000000000000000000, 0.8660254037844387076, 1.000000000000000000, 0.8660254037844387076, 1.000000000000000000, 0.8660254037844387076, 1.000000000000000000, 0.8660254037844387076, 1.000000000000000000, 0.8660254037844387076, 1.000000000000000000, 0.8660254037844387076, 1.000000000000000000, 0.8660254037844387076, 1.000000000000000000, 0.8660254037844387076, 1.000000000000000000, 0.8660254037844387076, 1.000000000000000000, 0.8660254037844387076, 1.000000000000000000, 0.8660254037844387076, 1.000000000000000000, 0.8660254037844387076, 1.000000000000000000, 0.8660254037844387076, 1.000000000000000000, 0.8660254037844387076, 1.000000000000000000, 0.8660254037844387076, 1.000000000000000000, 0.8660254037844387076, 1.000000000000000000, 0.8660254037844387076, 1.000000000000000000, 0.8660254037844387076, 1.000000000000000000, 0.8660254037844387076, 1.000000000000000000, 0.8660254037844387076, 1.000000000000000000, 0.8660254037844387076, 1.000000000000000000, 0.8660254037844387076, 1.000000000000000000, 0.8660254037844387076, 1.000000000000000000, 0.8660254037844387076, 1.000000000000000000, 0.8660254037844387076, 1.000000000000000000, 0.8660254037844387076, 1.000000000000000000, 0.8660254037844387076, 1.000000000000000000, 0.8660254037844387076, 1.000000000000000000, 0.8660254037844387076, 1.000000000000000000, 0.8660254037844387076, 1.000000000000000000, 0.9548846395026737710, 0.9401540804572410259 ) ) 
 REPRESENTATION_ITEM ( '' )  );
#59807 = CARTESIAN_POINT ( 'NONE',  ( 22.88437500061451857, 6.421520780324663323E-16, -5.243569643749999010 ) ) ;
#59808 = CARTESIAN_POINT ( 'NONE',  ( 14.01562500061451644, 3.027376345333611329, 5.243569643749999010 ) ) ;
#59809 = CARTESIAN_POINT ( 'NONE',  ( 23.13750000122903216, 6.123233995736764310E-16, -4.999999999999998224 ) ) ;
#59810 = CARTESIAN_POINT ( 'NONE',  ( 22.52812500061451573, 4.541064518000418104, 2.621784821874999949 ) ) ;
#59811 = CARTESIAN_POINT ( 'NONE',  ( 18.53437500061451715, 4.541064518000418104, 2.621784821874999949 ) ) ;
#59812 = CARTESIAN_POINT ( 'NONE',  ( 12.74062500061451786, -3.027376345333614438, 5.243569643749998122 ) ) ;
#59813 = CARTESIAN_POINT ( 'NONE',  ( 2.121784821874999061, 14.75937500061451679, 26.32496088578401583 ) ) ;
#59814 = CARTESIAN_POINT ( 'NONE',  ( 19.64062500061451644, -3.027376345333610441, -5.243569643749999898 ) ) ;
#59815 = CARTESIAN_POINT ( 'NONE',  ( 23.41875000122903216, -5.773502691896255534, -1.060575238724906372E-15 ) ) ;
#59816 = EDGE_LOOP ( 'NONE', ( #6299, #26071, #67905, #34749 ) ) ;
#59817 = VERTEX_POINT ( 'NONE', #31954 ) ;
#59818 = CARTESIAN_POINT ( 'NONE',  ( 23.32499999999999929, -4.330127018922194537, 2.499999999999995559 ) ) ;
#59819 = CARTESIAN_POINT ( 'NONE',  ( -3.999999999999999112, 10.10000000000000142, -30.00000000000000000 ) ) ;
#59820 = CARTESIAN_POINT ( 'NONE',  ( 14.94375000122903252, -2.886751345948126435, -5.000000000000000000 ) ) ;
#59821 = CARTESIAN_POINT ( 'NONE',  ( 26.91562500061451146, 3.027376345333613106, -5.243569643749998122 ) ) ;
#59822 = CARTESIAN_POINT ( 'NONE',  ( 5.653125000614517504, -4.541064518000417216, -2.621784821875001281 ) ) ;
#59823 = CARTESIAN_POINT ( 'NONE',  ( 20.21250000122903145, 0.000000000000000000, 4.999999999999998224 ) ) ;
#59824 = CARTESIAN_POINT ( 'NONE',  ( 24.81562500061451715, 3.027376345333611329, 5.243569643749999010 ) ) ;
#59825 = CARTESIAN_POINT ( 'NONE',  ( 23.32499999999999929, -4.330127018922194537, 2.499999999999995559 ) ) ;
#59826 = CARTESIAN_POINT ( 'NONE',  ( 27.62812500061451360, -4.541064518000419881, 2.621784821874995952 ) ) ;
#59827 = CARTESIAN_POINT ( 'NONE',  ( 9.215625000614515727, -6.054752690667223547, -1.112240025338166033E-15 ) ) ;
#59828 = ORIENTED_EDGE ( 'NONE', *, *, #23424, .T. ) ;
#59829 = CARTESIAN_POINT ( 'NONE',  ( 22.11562500061451786, 3.027376345333611329, 5.243569643749999010 ) ) ;
#59830 = CARTESIAN_POINT ( 'NONE',  ( 5.653125000614517504, -4.541064518000417216, -2.621784821875001281 ) ) ;
#59831 = CARTESIAN_POINT ( 'NONE',  ( 15.15937500061451715, -4.119189519843965641, -2.378215178125001383 ) ) ;
#59832 = CARTESIAN_POINT ( 'NONE',  ( 3.215625000614518836, 3.027376345333611329, 5.243569643749999010 ) ) ;
#59833 = CARTESIAN_POINT ( 'NONE',  ( -3.999999999999999556, 13.77500000122903678, -32.30940107675850470 ) ) ;
#59834 = EDGE_CURVE ( 'NONE', #11370, #49299, #32857, .T. ) ;
#59835 = CARTESIAN_POINT ( 'NONE',  ( 1.626862140677534273E-15, 10.32500000122903572, 34.00000000000000000 ) ) ;
#59836 = AXIS2_PLACEMENT_3D ( 'NONE', #49767, #25766, #14665 ) ;
#59837 = CARTESIAN_POINT ( 'NONE',  ( 10.98750000000000071, 5.773502691896255534, 3.535250795749688894E-16 ) ) ;
#59838 = CARTESIAN_POINT ( 'NONE',  ( 10.13437500061451679, -4.541064518000419881, 2.621784821874995952 ) ) ;
#59839 = CARTESIAN_POINT ( 'NONE',  ( 6.675000001229034474, 2.886751345948126879, 4.999999999999999112 ) ) ;
#59840 = CARTESIAN_POINT ( 'NONE',  ( 14.14687500061451786, -3.027376345333614438, 5.243569643749998122 ) ) ;
#59841 = CARTESIAN_POINT ( 'NONE',  ( 15.33750000000000036, -2.886751345948125991, -5.000000000000000000 ) ) ;
#59842 = CARTESIAN_POINT ( 'NONE',  ( 5.934375000614517504, 4.541064518000418104, 2.621784821874999949 ) ) ;
#59843 = CARTESIAN_POINT ( 'NONE',  ( 2.000000000000001332, 18.35000000000000142, 33.46410161513774995 ) ) ;
#59844 = DIRECTION ( 'NONE',  ( 0.000000000000000000, 1.000000000000000000, 0.000000000000000000 ) ) ;
#59845 = CARTESIAN_POINT ( 'NONE',  ( 13.43437500061451750, 6.421520780324663323E-16, -5.243569643749999010 ) ) ;
#59846 = CARTESIAN_POINT ( 'NONE',  ( 11.32500000000000107, 6.123233995736764310E-16, -4.999999999999998224 ) ) ;
#59847 = CARTESIAN_POINT ( 'NONE',  ( 22.45312500061451644, 4.541064518000418104, -2.621784821874998173 ) ) ;
#59848 = CARTESIAN_POINT ( 'NONE',  ( -3.137519842735245283E-14, 11.56250000000000178, 34.00000000000000000 ) ) ;
#59849 = CARTESIAN_POINT ( 'NONE',  ( -4.243569643749998122, 18.94062500061459531, 32.45002607614398471 ) ) ;
#59850 = CARTESIAN_POINT ( 'NONE',  ( 26.97187500061451360, 3.027376345333613106, -5.243569643749998122 ) ) ;
#59851 = CARTESIAN_POINT ( 'NONE',  ( -3.305248395036964552E-15, 5.000000000000034639, 25.99999999999995737 ) ) ;
#59852 =( BOUNDED_CURVE ( )  B_SPLINE_CURVE ( 2, ( #9735, #38168, #4571, #60692, #10105, #27101, #21539 ),
 .UNSPECIFIED., .F., .F. ) 
 B_SPLINE_CURVE_WITH_KNOTS ( ( 3, 2, 2, 3 ),
 ( 0.01999999999999995878, 0.02333333333333328583, 0.02666666666666661634, 0.02999999999999993991 ),
 .UNSPECIFIED. ) 
 CURVE ( )  GEOMETRIC_REPRESENTATION_ITEM ( )  RATIONAL_B_SPLINE_CURVE ( ( 1.000000000000001554, 0.8660254037844370423, 1.000000000000000000, 0.8660254037844387076, 1.000000000000000000, 0.8660254037844410391, 0.9999999999999976685 ) ) 
 REPRESENTATION_ITEM ( '' )  );
#59853 = CARTESIAN_POINT ( 'NONE',  ( 4.415625000614518569, 3.027376345333613106, -5.243569643749998122 ) ) ;
#59854 = CARTESIAN_POINT ( 'NONE',  ( 21.75937500061451502, -5.492252693125287522, -1.008910452111647106E-15 ) ) ;
#59855 = CARTESIAN_POINT ( 'NONE',  ( 13.09687500061451892, 6.054752690667223547, 3.707466751127219781E-16 ) ) ;
#59856 = CARTESIAN_POINT ( 'NONE',  ( 29.96250000000000213, 2.886751345948126879, 4.999999999999999112 ) ) ;
#59857 = CARTESIAN_POINT ( 'NONE',  ( 27.82500000122903572, 2.886751345948126879, 4.999999999999999112 ) ) ;
#59858 = CARTESIAN_POINT ( 'NONE',  ( 5.034375000614519813, 4.541064518000418104, 2.621784821874999949 ) ) ;
#59859 = CARTESIAN_POINT ( 'NONE',  ( 15.49687500061451750, -3.027376345333614438, 5.243569643749998122 ) ) ;
#59860 = CARTESIAN_POINT ( 'NONE',  ( 4.000000000000000000, 17.84374999877096712, 30.00000000000000000 ) ) ;
#59861 = CARTESIAN_POINT ( 'NONE',  ( 24.56250000000000000, 2.886751345948126879, 4.999999999999999112 ) ) ;
#59862 = CARTESIAN_POINT ( 'NONE',  ( 4.162500001229033408, -4.330127018922190985, -2.500000000000001332 ) ) ;
#59863 = CARTESIAN_POINT ( 'NONE',  ( 27.34687500061451360, -3.027376345333610441, -5.243569643749999898 ) ) ;
#59864 = CARTESIAN_POINT ( 'NONE',  ( 2.655984681222220721E-16, 14.66562499938548214, 25.66244784525396483 ) ) ;
#59865 = CARTESIAN_POINT ( 'NONE',  ( 29.47499999999999787, 4.330127018922191873, 2.499999999999999556 ) ) ;
#59866 = CARTESIAN_POINT ( 'NONE',  ( 9.074999999999999289, 6.123233995736764310E-16, -4.999999999999998224 ) ) ;
#59867 = CARTESIAN_POINT ( 'NONE',  ( 8.859375000614514661, 2.746126346562645981, -4.756430356249997438 ) ) ;
#59868 = CARTESIAN_POINT ( 'NONE',  ( 23.24062500061451786, -3.027376345333610441, -5.243569643749999898 ) ) ;
#59869 = CARTESIAN_POINT ( 'NONE',  ( 11.36250000000000071, 2.886751345948129099, -4.999999999999998224 ) ) ;
#59870 = CARTESIAN_POINT ( 'NONE',  ( 4.228125000614517681, -4.541064518000419881, 2.621784821874995952 ) ) ;
#59871 = CARTESIAN_POINT ( 'NONE',  ( 19.76250000000000639, -5.773502691896255534, -1.060575238724906372E-15 ) ) ;
#59872 = CARTESIAN_POINT ( 'NONE',  ( 17.65312500061451573, 0.000000000000000000, 5.243569643749999010 ) ) ;
#59873 = CARTESIAN_POINT ( 'NONE',  ( -3.999999999999999112, 18.76250000122903216, 30.00000000000000000 ) ) ;
#59874 = CARTESIAN_POINT ( 'NONE',  ( 23.02500000122903145, -5.773502691896255534, -1.060575238724906372E-15 ) ) ;
#59875 = CARTESIAN_POINT ( 'NONE',  ( 1.878215178125000495, 19.01562499938548356, 26.74683588394047007 ) ) ;
#59876 = CARTESIAN_POINT ( 'NONE',  ( 3.525000000000000355, -4.330127018922194537, 2.499999999999995559 ) ) ;
#59877 = VERTEX_POINT ( 'NONE', #48219 ) ;
#59878 = CARTESIAN_POINT ( 'NONE',  ( 18.70312500061451644, -4.541064518000417216, -2.621784821875001281 ) ) ;
#59879 = CARTESIAN_POINT ( 'NONE',  ( 24.10312500061451502, -4.541064518000417216, -2.621784821875001281 ) ) ;
#59880 = CARTESIAN_POINT ( 'NONE',  ( 24.08437500061451786, -4.541064518000419881, 2.621784821874995952 ) ) ;
#59881 = CARTESIAN_POINT ( 'NONE',  ( 9.112500000000000711, 2.886751345948129099, -4.999999999999998224 ) ) ;
#59882 = CARTESIAN_POINT ( 'NONE',  ( 12.06562500061451537, 3.027376345333613106, -5.243569643749998122 ) ) ;
#59883 = CARTESIAN_POINT ( 'NONE',  ( 26.69062500061451715, -3.027376345333614438, 5.243569643749998122 ) ) ;
#59884 = CARTESIAN_POINT ( 'NONE',  ( 17.14687500061451786, 6.054752690667223547, 3.707466751127219781E-16 ) ) ;
#59885 = CARTESIAN_POINT ( 'NONE',  ( 9.815625000614518925, 3.027376345333613106, -5.243569643749998122 ) ) ;
#59886 = DIRECTION ( 'NONE',  ( -0.000000000000000000, -1.000000000000000000, -0.000000000000000000 ) ) ;
#59887 = CARTESIAN_POINT ( 'NONE',  ( 2.121784821875001281, 19.05312500061451431, 33.67503911421598417 ) ) ;
#59888 = AXIS2_PLACEMENT_3D ( 'NONE', #32360, #54898, #52258 ) ;
#59889 = CARTESIAN_POINT ( 'NONE',  ( 23.10000000122903074, -2.886751345948125991, -5.000000000000000000 ) ) ;
#59890 = CARTESIAN_POINT ( 'NONE',  ( 20.67187500061451289, 2.746126346562645981, -4.756430356249997438 ) ) ;
#59891 = CARTESIAN_POINT ( 'NONE',  ( 15.14062500061451644, -3.027376345333610441, -5.243569643749999898 ) ) ;
#59892 = CARTESIAN_POINT ( 'NONE',  ( 8.859375000614518214, -4.541064518000417216, -2.621784821875001281 ) ) ;
#59893 = CARTESIAN_POINT ( 'NONE',  ( 7.509375000614517681, -4.541064518000417216, -2.621784821875001281 ) ) ;
#59894 = ORIENTED_EDGE ( 'NONE', *, *, #16132, .F. ) ;
#59895 = CARTESIAN_POINT ( 'NONE',  ( 29.67187500061451644, 3.027376345333613106, -5.243569643749998122 ) ) ;
#59896 = CARTESIAN_POINT ( 'NONE',  ( 21.25312500061451715, 0.000000000000000000, 5.243569643749999010 ) ) ;
#59897 = EDGE_CURVE ( 'NONE', #10639, #51352, #33590, .T. ) ;
#59898 = CARTESIAN_POINT ( 'NONE',  ( 15.90937500061451892, 0.000000000000000000, 5.243569643749999010 ) ) ;
#59899 = CARTESIAN_POINT ( 'NONE',  ( 21.55312500061451431, 4.541064518000418104, -2.621784821874998173 ) ) ;
#59900 = CARTESIAN_POINT ( 'NONE',  ( -3.999999999999999112, 11.90000000000000036, 30.00000000000000000 ) ) ;
#59901 = CARTESIAN_POINT ( 'NONE',  ( 27.51562500061451644, 3.027376345333611329, 5.243569643749999010 ) ) ;
#59902 = CARTESIAN_POINT ( 'NONE',  ( 6.000000001229033764, -2.886751345948125991, -5.000000000000000000 ) ) ;
#59903 = ORIENTED_EDGE ( 'NONE', *, *, #41229, .F. ) ;
#59904 = CARTESIAN_POINT ( 'NONE',  ( 29.02499999999999858, 4.330127018922191873, 2.499999999999999556 ) ) ;
#59905 = CARTESIAN_POINT ( 'NONE',  ( 8.484601909799253346E-16, 16.96250000000000213, -25.38119784648299770 ) ) ;
#59906 = CARTESIAN_POINT ( 'NONE',  ( 24.48750000122903359, 6.123233995736764310E-16, -4.999999999999998224 ) ) ;
#59907 = CARTESIAN_POINT ( 'NONE',  ( -7.967954043666661671E-16, 15.79062499938548392, 34.33755215474603517 ) ) ;
#59908 = CARTESIAN_POINT ( 'NONE',  ( 6.796875000614516438, 6.054752690667223547, 3.707466751127219781E-16 ) ) ;
#59909 = CARTESIAN_POINT ( 'NONE',  ( 3.999999999999998668, 15.31250000000000000, 27.69059892324149530 ) ) ;
#59910 = CARTESIAN_POINT ( 'NONE',  ( 15.66562500061451857, 3.027376345333613106, -5.243569643749998122 ) ) ;
#59911 = CARTESIAN_POINT ( 'NONE',  ( 7.659375000614518036, 4.541064518000418104, -2.621784821874998173 ) ) ;
#59912 = CARTESIAN_POINT ( 'NONE',  ( 27.11250000122903359, -4.330127018922190985, -2.500000000000001332 ) ) ;
#59913 = CARTESIAN_POINT ( 'NONE',  ( 18.12187500061451928, 3.027376345333611329, 5.243569643749999010 ) ) ;
#59914 = CARTESIAN_POINT ( 'NONE',  ( 4.284375000614518925, -4.541064518000419881, 2.621784821874995952 ) ) ;
#59915 = CARTESIAN_POINT ( 'NONE',  ( 7.837500001229035007, 6.123233995736764310E-16, -4.999999999999998224 ) ) ;
#59916 = CARTESIAN_POINT ( 'NONE',  ( 4.340625000614515727, -3.027376345333610441, -5.243569643749999898 ) ) ;
#59917 = CARTESIAN_POINT ( 'NONE',  ( 16.34062500061451573, -3.027376345333614438, 5.243569643749998122 ) ) ;
#59918 = ORIENTED_EDGE ( 'NONE', *, *, #35474, .F. ) ;
#59919 = CARTESIAN_POINT ( 'NONE',  ( 12.70312500061451821, 0.000000000000000000, 5.243569643749999010 ) ) ;
#59920 = CARTESIAN_POINT ( 'NONE',  ( 6.037500001229035185, 6.123233995736764310E-16, -4.999999999999998224 ) ) ;
#59921 = CARTESIAN_POINT ( 'NONE',  ( 9.140625000614518214, -3.027376345333614438, 5.243569643749998122 ) ) ;
#59922 = CARTESIAN_POINT ( 'NONE',  ( 22.20937500061451431, 0.000000000000000000, 4.756430356249998326 ) ) ;
#59923 = CARTESIAN_POINT ( 'NONE',  ( 8.324999999999999289, 4.330127018922191873, 2.499999999999999556 ) ) ;
#59924 = CARTESIAN_POINT ( 'NONE',  ( 3.600000001229033408, -2.886751345948129988, 4.999999999999997335 ) ) ;
#59925 = CARTESIAN_POINT ( 'NONE',  ( 18.48750000000000071, -2.886751345948125991, -5.000000000000000000 ) ) ;
#59926 = CARTESIAN_POINT ( 'NONE',  ( 19.28437500061451360, 6.421520780324663323E-16, -5.243569643749999010 ) ) ;
#59927 = CARTESIAN_POINT ( 'NONE',  ( 15.41250000122903252, -4.330127018922190985, -2.500000000000001332 ) ) ;
#59928 = CARTESIAN_POINT ( 'NONE',  ( 21.93750000000000000, -2.886751345948129988, 4.999999999999997335 ) ) ;
#59929 = CARTESIAN_POINT ( 'NONE',  ( 4.243569643749999898, 15.49062500061451786, -27.54997392385601529 ) ) ;
#59930 = CARTESIAN_POINT ( 'NONE',  ( -1.071796769724488563, 16.15490381179669654, 34.00000000000000000 ) ) ;
#59931 = CARTESIAN_POINT ( 'NONE',  ( 4.000000000000000000, 16.08124999877096784, 27.69059892324149885 ) ) ;
#59932 = CARTESIAN_POINT ( 'NONE',  ( 28.26562500061451289, 3.027376345333613106, -5.243569643749998122 ) ) ;
#59933 = EDGE_CURVE ( 'NONE', #5936, #57032, #19479, .T. ) ;
#59934 =( NAMED_UNIT ( * ) PLANE_ANGLE_UNIT ( ) SI_UNIT ( $, .RADIAN. ) );
#59935 = CARTESIAN_POINT ( 'NONE',  ( 19.66875000122903216, 2.886751345948126879, 4.999999999999998224 ) ) ;
#59936 = CARTESIAN_POINT ( 'NONE',  ( 16.20937500061451786, 4.541064518000418104, -2.621784821874998173 ) ) ;
#59937 = CARTESIAN_POINT ( 'NONE',  ( 29.77499999999999858, 6.123233995736764310E-16, -4.999999999999998224 ) ) ;
#59938 = CARTESIAN_POINT ( 'NONE',  ( 11.99062500061451608, -3.027376345333610441, -5.243569643749999898 ) ) ;
#59939 = CARTESIAN_POINT ( 'NONE',  ( 8.118750001229033231, -5.773502691896255534, -1.060575238724906372E-15 ) ) ;
#59940 = CARTESIAN_POINT ( 'NONE',  ( 24.75937500061451502, 4.541064518000418104, -2.621784821874998173 ) ) ;
#59941 = CARTESIAN_POINT ( 'NONE',  ( 15.19687500061451502, 4.119189519843966529, -2.378215178124998275 ) ) ;
#59942 = CARTESIAN_POINT ( 'NONE',  ( 6.628125000614517148, 6.421520780324663323E-16, -5.243569643749999010 ) ) ;
#59943 = CARTESIAN_POINT ( 'NONE',  ( 12.45937500061451786, -4.541064518000417216, -2.621784821875001281 ) ) ;
#59944 = EDGE_LOOP ( 'NONE', ( #46901, #45336, #10465, #37270, #47060 ) ) ;
#59945 = CARTESIAN_POINT ( 'NONE',  ( 23.67187500061451999, -6.054752690667223547, -1.112240025338166033E-15 ) ) ;
#59946 = CARTESIAN_POINT ( 'NONE',  ( 27.47812500061451502, 4.541064518000418104, 2.621784821874999949 ) ) ;
#59947 = FACE_OUTER_BOUND ( 'NONE', #5997, .T. ) ;
#59948 = CARTESIAN_POINT ( 'NONE',  ( 6.825000000000001066, 6.123233995736764310E-16, -4.999999999999998224 ) ) ;
#59949 = CARTESIAN_POINT ( 'NONE',  ( 17.17500000122903359, -5.773502691896255534, -1.060575238724906372E-15 ) ) ;
#59950 = CYLINDRICAL_SURFACE ( 'NONE', #677, 4.000000000000000000 ) ;
#59951 = CARTESIAN_POINT ( 'NONE',  ( 8.971875000614515372, 4.119189519843966529, 2.378215178124999607 ) ) ;
#59952 = VERTEX_POINT ( 'NONE', #47854 ) ;
#59953 = CARTESIAN_POINT ( 'NONE',  ( 14.81250000000000000, -5.773502691896255534, -1.060575238724906372E-15 ) ) ;
#59954 = CARTESIAN_POINT ( 'NONE',  ( 19.87500000000000000, 6.123233995736764310E-16, -4.999999999999998224 ) ) ;
#59955 = CARTESIAN_POINT ( 'NONE',  ( 11.95312500061451644, -4.541064518000417216, -2.621784821875001281 ) ) ;
#59956 = VERTEX_POINT ( 'NONE', #3892 ) ;
#59957 = CARTESIAN_POINT ( 'NONE',  ( 18.48750000122903359, -4.330127018922194537, 2.499999999999995559 ) ) ;
#59958 = CARTESIAN_POINT ( 'NONE',  ( -4.243569643749999898, 17.15937500061451715, -30.00000000000000000 ) ) ;
#59959 = CARTESIAN_POINT ( 'NONE',  ( 3.178125000614515638, 4.541064518000418104, 2.621784821874999949 ) ) ;
#59960 = CARTESIAN_POINT ( 'NONE',  ( 3.756430356249998770, 13.50312499938548427, 32.16877607737301759 ) ) ;
#59961 = CARTESIAN_POINT ( 'NONE',  ( 10.16249999999999964, 2.886751345948126879, 4.999999999999999112 ) ) ;
#59962 = ORIENTED_EDGE ( 'NONE', *, *, #51187, .F. ) ;
#59963 = CARTESIAN_POINT ( 'NONE',  ( -2.121784821874999949, 12.07812500061451821, 26.32496088578401938 ) ) ;
#59964 = CARTESIAN_POINT ( 'NONE',  ( 27.36562500061451786, 3.027376345333613106, -5.243569643749998122 ) ) ;
#59965 = CARTESIAN_POINT ( 'NONE',  ( 3.533900615097678610, 3.537227818301726501, 3.601564948538577671 ) ) ;
#59966 = CARTESIAN_POINT ( 'NONE',  ( -3.756430356250000102, 20.51562499938548356, 30.00000000000000000 ) ) ;
#59967 = CARTESIAN_POINT ( 'NONE',  ( 24.75937500061451502, 4.541064518000418104, -2.621784821874998173 ) ) ;
#59968 = CARTESIAN_POINT ( 'NONE',  ( 19.41562500061451146, 3.027376345333611329, 5.243569643749999010 ) ) ;
#59969 = CARTESIAN_POINT ( 'NONE',  ( -4.243569643749999898, 14.85312500061459495, -30.00000000000000000 ) ) ;
#59970 = CARTESIAN_POINT ( 'NONE',  ( 22.57500000122903572, -5.773502691896255534, -1.060575238724906372E-15 ) ) ;
#59971 = CARTESIAN_POINT ( 'NONE',  ( 3.328125000614516438, -4.541064518000419881, 2.621784821874995952 ) ) ;
#59972 = CARTESIAN_POINT ( 'NONE',  ( 26.10937500061451644, 4.119189519843966529, -2.378215178124998275 ) ) ;
#59973 = CARTESIAN_POINT ( 'NONE',  ( 21.55312500061451431, 4.541064518000418104, -2.621784821874998173 ) ) ;
#59974 = CARTESIAN_POINT ( 'NONE',  ( 7.659375000614518036, 4.119189519843966529, -2.378215178124998275 ) ) ;
#59975 = CARTESIAN_POINT ( 'NONE',  ( 3.756430356250000546, 17.17812499938548143, 27.83122392262697886 ) ) ;
#59976 = CARTESIAN_POINT ( 'NONE',  ( 16.05937500061451573, -4.541064518000417216, -2.621784821875001281 ) ) ;
#59977 = CARTESIAN_POINT ( 'NONE',  ( 16.88437500061451502, -4.541064518000419881, 2.621784821874995952 ) ) ;
#59978 = CARTESIAN_POINT ( 'NONE',  ( 24.64687500061451431, -3.027376345333610441, -5.243569643749999898 ) ) ;
#59979 = CARTESIAN_POINT ( 'NONE',  ( 4.243569643749999898, 14.64687500061451964, 32.45002607614398471 ) ) ;
#59980 = CARTESIAN_POINT ( 'NONE',  ( 5.878125000614517148, 4.541064518000418104, 2.621784821874999949 ) ) ;
#59981 = CARTESIAN_POINT ( 'NONE',  ( 27.74062500061451431, -3.027376345333610441, -5.243569643749999898 ) ) ;
#59982 = CARTESIAN_POINT ( 'NONE',  ( 29.24062500061451431, 6.054752690667223547, 3.707466751127219781E-16 ) ) ;
#59983 = DIRECTION ( 'NONE',  ( -1.000000000000000000, -0.000000000000000000, -0.000000000000000000 ) ) ;
#59984 = CARTESIAN_POINT ( 'NONE',  ( -2.828200636599751609E-16, 18.53750000000000142, 25.38119784648299770 ) ) ;
#59985 = CARTESIAN_POINT ( 'NONE',  ( 7.846875000614518036, -3.027376345333614438, 5.243569643749998122 ) ) ;
#59986 = DIRECTION ( 'NONE',  ( 0.000000000000000000, 0.000000000000000000, 1.000000000000000000 ) ) ;
#59987 = CARTESIAN_POINT ( 'NONE',  ( 14.36250000122903359, 0.000000000000000000, 4.999999999999998224 ) ) ;
#59988 = CARTESIAN_POINT ( 'NONE',  ( 8.625000001229034652, -5.773502691896255534, -1.060575238724906372E-15 ) ) ;
#59989 = CARTESIAN_POINT ( 'NONE',  ( 4.715625000614516615, -6.054752690667223547, -1.112240025338166033E-15 ) ) ;
#59990 = CARTESIAN_POINT ( 'NONE',  ( 2.828200636599751609E-16, 15.25624999877096499, 25.38119784648299415 ) ) ;
#59991 = CARTESIAN_POINT ( 'NONE',  ( 20.75625000122903430, -4.330127018922190985, -2.500000000000001332 ) ) ;
#59992 = CARTESIAN_POINT ( 'NONE',  ( 14.25937500061451679, -4.541064518000417216, -2.621784821875001281 ) ) ;
#59993 = CARTESIAN_POINT ( 'NONE',  ( 7.537500000000000533, -2.886751345948063374, 5.000000000000112799 ) ) ;
#59994 = EDGE_LOOP ( 'NONE', ( #3086, #7909, #27863, #59056, #1020, #53261, #37756, #25606, #50013, #44678, #15423, #34286, #46621, #46116, #44979, #12127, #6284, #33874, #10262, #60682, #58374, #58222, #35899, #31117, #65082, #5087, #47103, #57863, #12696, #51716, #66097, #51841, #32995, #14473, #43755, #23429, #13508, #29705, #51096, #53692, #57395, #60315, #37294, #656, #55746, #5150, #51079, #53928 ) ) ;
#59995 = CARTESIAN_POINT ( 'NONE',  ( 21.47812500061451502, 6.421520780324663323E-16, -5.243569643749999010 ) ) ;
#59996 = CARTESIAN_POINT ( 'NONE',  ( 6.328125000614515550, 4.541064518000418104, 2.621784821874999949 ) ) ;
#59997 = CARTESIAN_POINT ( 'NONE',  ( 24.19687500061451502, -3.027376345333610441, -5.243569643749999898 ) ) ;
#59998 = CARTESIAN_POINT ( 'NONE',  ( 6.515625000614516438, -6.054752690667223547, -1.112240025338166033E-15 ) ) ;
#59999 = CARTESIAN_POINT ( 'NONE',  ( 20.92500000000000071, 4.330127018922191873, 2.499999999999999556 ) ) ;
#60001 = EDGE_CURVE ( 'NONE', #15065, #41205, #42308, .T. ) ;
#60000 = CARTESIAN_POINT ( 'NONE',  ( 7.275000001229035007, -5.773502691896255534, -1.060575238724906372E-15 ) ) ;
#60002 = CARTESIAN_POINT ( 'NONE',  ( 21.40312500061451573, -4.541064518000417216, -2.621784821875001281 ) ) ;
#60003 = CARTESIAN_POINT ( 'NONE',  ( -2.121784821874999949, 9.828125000614516438, -33.67503911421598417 ) ) ;
#60004 = CARTESIAN_POINT ( 'NONE',  ( 10.91250000122903252, -4.330127018922190985, -2.500000000000001332 ) ) ;
#60005 = CARTESIAN_POINT ( 'NONE',  ( 20.42812500061451431, -4.541064518000419881, 2.621784821874995952 ) ) ;
#60006 = CARTESIAN_POINT ( 'NONE',  ( 19.11562500061451431, -6.054752690667223547, -1.112240025338166033E-15 ) ) ;
#60007 = CARTESIAN_POINT ( 'NONE',  ( 28.84687500061452070, 5.492252693125287522, 3.363034840372157021E-16 ) ) ;
#60008 = CARTESIAN_POINT ( 'NONE',  ( 18.41250000000000142, -5.773502691896255534, -1.060575238724906372E-15 ) ) ;
#60009 = CARTESIAN_POINT ( 'NONE',  ( 10.35000000122903074, -2.886751345948129988, 4.999999999999997335 ) ) ;
#60010 = CARTESIAN_POINT ( 'NONE',  ( 8.428125000614517859, 6.421520780324663323E-16, -5.243569643749999010 ) ) ;
#60011 = CARTESIAN_POINT ( 'NONE',  ( 11.12812500061451715, 6.421520780324663323E-16, -5.243569643749999010 ) ) ;
#60012 = CARTESIAN_POINT ( 'NONE',  ( 22.91250000122903430, 0.000000000000000000, 4.999999999999998224 ) ) ;
#60013 = CARTESIAN_POINT ( 'NONE',  ( 21.60937500061451644, 4.541064518000418104, -2.621784821874998173 ) ) ;
#60014 = CARTESIAN_POINT ( 'NONE',  ( 4.779965814201476704, -3.457634596098181579, -4.498340493050051236 ) ) ;
#60015 = CARTESIAN_POINT ( 'NONE',  ( 4.725000001229034297, 2.886751345948129099, -4.999999999999998224 ) ) ;
#60016 = CARTESIAN_POINT ( 'NONE',  ( 5.859375000614519102, 4.541064518000418104, -2.621784821874998173 ) ) ;
#60017 = CARTESIAN_POINT ( 'NONE',  ( 23.82187500061451502, 3.027376345333613106, -5.243569643749998122 ) ) ;
#60018 = CARTESIAN_POINT ( 'NONE',  ( 27.52500000000000213, 6.123233995736764310E-16, -4.999999999999998224 ) ) ;
#60019 = CARTESIAN_POINT ( 'NONE',  ( 19.49062500061451431, -3.027376345333614438, 5.243569643749998122 ) ) ;
#60020 = CARTESIAN_POINT ( 'NONE',  ( 25.32187500061451857, 3.027376345333611329, 5.243569643749999010 ) ) ;
#60021 = CARTESIAN_POINT ( 'NONE',  ( 2.655984681222220721E-16, 19.61562499938548143, 25.66244784525396483 ) ) ;
#60022 = CARTESIAN_POINT ( 'NONE',  ( 12.48750000122903359, 4.330127018922191873, 2.499999999999999556 ) ) ;
#60023 = CARTESIAN_POINT ( 'NONE',  ( -5.810221930991193690E-16, 13.25000000122903465, -34.00000000000000000 ) ) ;
#60024 = CARTESIAN_POINT ( 'NONE',  ( 4.696875000614518569, -3.027376345333614438, 5.243569643749998122 ) ) ;
#60025 = CARTESIAN_POINT ( 'NONE',  ( 15.62812500061451537, 6.421520780324663323E-16, -5.243569643749999010 ) ) ;
#60026 = CARTESIAN_POINT ( 'NONE',  ( 12.72187500061451537, 3.027376345333611329, 5.243569643749999010 ) ) ;
#60027 = ORIENTED_EDGE ( 'NONE', *, *, #15468, .F. ) ;
#60028 = CARTESIAN_POINT ( 'NONE',  ( 9.112499999999997158, 2.886751345948062486, -5.000000000000113687 ) ) ;
#60029 = CARTESIAN_POINT ( 'NONE',  ( 25.26562500061451289, 3.027376345333611329, 5.243569643749999010 ) ) ;
#60030 = CARTESIAN_POINT ( 'NONE',  ( -3.999999999999999112, 10.62500000122903643, -32.30940107675850470 ) ) ;
#60031 = CARTESIAN_POINT ( 'NONE',  ( -2.498395430326213790E-14, 20.26249999999999929, 26.00000000000000000 ) ) ;
#60032 = EDGE_CURVE ( 'NONE', #10316, #52965, #67814, .T. ) ;
#60033 = CARTESIAN_POINT ( 'NONE',  ( 15.15000000000000036, 0.000000000000000000, 4.999999999999998224 ) ) ;
#60034 = CARTESIAN_POINT ( 'NONE',  ( 24.37500000122903288, -5.773502691896255534, -1.060575238724906372E-15 ) ) ;
#60035 = CARTESIAN_POINT ( 'NONE',  ( 19.71562500061451928, 3.027376345333613106, -5.243569643749998122 ) ) ;
#60036 = ORIENTED_EDGE ( 'NONE', *, *, #72113, .F. ) ;
#60037 = CARTESIAN_POINT ( 'NONE',  ( 21.37499999999999645, 4.330127018922191873, 2.499999999999999556 ) ) ;
#60038 = CARTESIAN_POINT ( 'NONE',  ( 24.15937500061451715, -4.541064518000417216, -2.621784821875001281 ) ) ;
#60039 = ORIENTED_EDGE ( 'NONE', *, *, #5795, .F. ) ;
#60040 = CARTESIAN_POINT ( 'NONE',  ( 2.970930829860112254, -4.021644987030126295, -3.364735388248410786 ) ) ;
#60041 = CARTESIAN_POINT ( 'NONE',  ( 10.26562500061451644, 3.027376345333613106, -5.243569643749998122 ) ) ;
#60042 = CARTESIAN_POINT ( 'NONE',  ( 2.953125000614516438, -4.541064518000417216, -2.621784821875001281 ) ) ;
#60043 = CARTESIAN_POINT ( 'NONE',  ( 14.44687500061451502, 0.000000000000000000, 4.756430356249998326 ) ) ;
#60044 = CARTESIAN_POINT ( 'NONE',  ( 26.91562500061451146, 3.027376345333613106, -5.243569643749998122 ) ) ;
#60045 = CARTESIAN_POINT ( 'NONE',  ( 17.43750000000000355, -2.886751345948129988, 4.999999999999997335 ) ) ;
#60046 = CARTESIAN_POINT ( 'NONE',  ( 25.83749999999999858, 5.773502691896255534, 3.535250795749688894E-16 ) ) ;
#60047 = CARTESIAN_POINT ( 'NONE',  ( -5.810221930991193690E-16, 10.88749999999999929, -34.00000000000000000 ) ) ;
#60048 = CARTESIAN_POINT ( 'NONE',  ( 6.421875000614519102, 3.027376345333611329, 5.243569643749999010 ) ) ;
#60049 = CARTESIAN_POINT ( 'NONE',  ( 17.29687500061451999, -3.027376345333614438, 5.243569643749998122 ) ) ;
#60050 = CARTESIAN_POINT ( 'NONE',  ( 26.17500000000000071, 6.123233995736764310E-16, -4.999999999999998224 ) ) ;
#60051 = ORIENTED_EDGE ( 'NONE', *, *, #68597, .T. ) ;
#60052 = CARTESIAN_POINT ( 'NONE',  ( 27.21562500061451928, -6.054752690667223547, -1.112240025338166033E-15 ) ) ;
#60053 = CARTESIAN_POINT ( 'NONE',  ( 27.57187500061451857, 3.027376345333611329, 5.243569643749999010 ) ) ;
#60054 = CARTESIAN_POINT ( 'NONE',  ( 45.00000000000000000, -2.499999999999999556, 3.499999999999999556 ) ) ;
#60055 = CARTESIAN_POINT ( 'NONE',  ( 13.19999999999999929, 4.330127018922192761, -2.499999999999997780 ) ) ;
#60056 = CARTESIAN_POINT ( 'NONE',  ( 12.25312500061451537, 0.000000000000000000, 5.243569643749999010 ) ) ;
#60057 = CARTESIAN_POINT ( 'NONE',  ( -1.071796769724496556, 15.14240381056766616, -26.00000000000000355 ) ) ;
#60058 = CARTESIAN_POINT ( 'NONE',  ( 14.06249999999999467, 2.886751345948018077, -5.000000000000190070 ) ) ;
#60059 = CARTESIAN_POINT ( 'NONE',  ( 29.20312500061451644, 4.541064518000418104, -2.621784821874998173 ) ) ;
#60060 = CARTESIAN_POINT ( 'NONE',  ( 16.50000000122903288, 5.773502691896255534, 3.535250795749688894E-16 ) ) ;
#60061 = CARTESIAN_POINT ( 'NONE',  ( 3.866371165286906830, -4.006382843392613857, -3.547880648171726214 ) ) ;
#60062 = CARTESIAN_POINT ( 'NONE',  ( 15.68437500061451573, 5.824947211148865298E-16, -4.756430356249998326 ) ) ;
#60063 = CARTESIAN_POINT ( 'NONE',  ( 4.453125000614517326, 4.541064518000418104, -2.621784821874998173 ) ) ;
#60064 = CARTESIAN_POINT ( 'NONE',  ( 20.97187500061451715, -6.054752690667223547, -1.112240025338166033E-15 ) ) ;
#60065 = CARTESIAN_POINT ( 'NONE',  ( -4.243569643749997233, 17.19687500061451502, 32.45002607614398471 ) ) ;
#60066 = CARTESIAN_POINT ( 'NONE',  ( 23.10937500061451644, 0.000000000000000000, 5.243569643749999010 ) ) ;
#60067 = CARTESIAN_POINT ( 'NONE',  ( 5.775000000000002132, -4.330127018922194537, 2.499999999999995559 ) ) ;
#60068 = CARTESIAN_POINT ( 'NONE',  ( -1.999999999999997113, 10.73750000122903536, 33.46410161513775705 ) ) ;
#60069 = CARTESIAN_POINT ( 'NONE',  ( 12.85312500061451502, -4.541064518000417216, -2.621784821875001281 ) ) ;
#60070 = CARTESIAN_POINT ( 'NONE',  ( 4.837500001229035895, 4.330127018922191873, 2.499999999999999556 ) ) ;
#60071 = CARTESIAN_POINT ( 'NONE',  ( 9.609375000614518214, 0.000000000000000000, 5.243569643749999010 ) ) ;
#60072 = DIRECTION ( 'NONE',  ( 0.000000000000000000, 0.000000000000000000, 1.000000000000000000 ) ) ;
#60073 = CARTESIAN_POINT ( 'NONE',  ( 9.290625000614515017, -3.027376345333610441, -5.243569643749999898 ) ) ;
#60074 = CARTESIAN_POINT ( 'NONE',  ( 14.89687500061451786, 6.054752690667223547, 3.707466751127219781E-16 ) ) ;
#60075 = CARTESIAN_POINT ( 'NONE',  ( 24.65625000122903288, 0.000000000000000000, 4.999999999999998224 ) ) ;
#60076 = CARTESIAN_POINT ( 'NONE',  ( 20.40000000122903145, -2.886751345948125991, -5.000000000000000000 ) ) ;
#60077 = CARTESIAN_POINT ( 'NONE',  ( 10.54687500061451644, -3.027376345333614438, 5.243569643749998122 ) ) ;
#60078 = CARTESIAN_POINT ( 'NONE',  ( 11.84062500061451750, -3.027376345333614438, 5.243569643749998122 ) ) ;
#60079 = CARTESIAN_POINT ( 'NONE',  ( 27.99375000122903501, -2.886751345948125991, -5.000000000000000000 ) ) ;
#60080 = CARTESIAN_POINT ( 'NONE',  ( 21.45937500061451786, -4.541064518000417216, -2.621784821875001281 ) ) ;
#60081 = CARTESIAN_POINT ( 'NONE',  ( 0.000000000000000000, 20.00000000000000000, -36.00000000000000000 ) ) ;
#60082 = CARTESIAN_POINT ( 'NONE',  ( -3.861264241427936117, 3.177798304702606824, 28.92162313090120662 ) ) ;
#60083 = CARTESIAN_POINT ( 'NONE',  ( -4.999999999999996447, 2.928932188134524051, 4.999999999999996447 ) ) ;
#60084 = EDGE_CURVE ( 'NONE', #59218, #17166, #30028, .T. ) ;
#60085 = CARTESIAN_POINT ( 'NONE',  ( 4.243569643749999898, 15.58437500061451786, -30.00000000000000000 ) ) ;
#60086 = CARTESIAN_POINT ( 'NONE',  ( 15.45000000122903216, -2.886751345948125991, -5.000000000000000000 ) ) ;
#60087 =( BOUNDED_CURVE ( )  B_SPLINE_CURVE ( 2, ( #73086, #22467, #49832, #55372, #45018, #67553, #39471 ),
 .UNSPECIFIED., .F., .F. ) 
 B_SPLINE_CURVE_WITH_KNOTS ( ( 3, 2, 2, 3 ),
 ( 0.5100000000000000089, 0.5133333333333333082, 0.5166666666666667185, 0.5200000000000000178 ),
 .UNSPECIFIED. ) 
 CURVE ( )  GEOMETRIC_REPRESENTATION_ITEM ( )  RATIONAL_B_SPLINE_CURVE ( ( 1.000000000000000000, 0.8660254037844387076, 1.000000000000000000, 0.8660254037844387076, 1.000000000000000000, 0.8660254037844387076, 1.000000000000000000 ) ) 
 REPRESENTATION_ITEM ( '' )  );
#60088 = CARTESIAN_POINT ( 'NONE',  ( 9.196875000614518569, -3.027376345333614438, 5.243569643749998122 ) ) ;
#60089 = CARTESIAN_POINT ( 'NONE',  ( -4.243569643749999898, 17.06562500061451360, -32.45002607614398471 ) ) ;
#60090 = CARTESIAN_POINT ( 'NONE',  ( 16.83750000122903145, 6.123233995736764310E-16, -4.999999999999998224 ) ) ;
#60091 = CARTESIAN_POINT ( 'NONE',  ( 11.39062500061451644, -3.027376345333614438, 5.243569643749998122 ) ) ;
#60092 = ORIENTED_EDGE ( 'NONE', *, *, #63628, .T. ) ;
#60093 = CARTESIAN_POINT ( 'NONE',  ( 15.22500000000000142, -4.330127018922194537, 2.499999999999995559 ) ) ;
#60094 = CYLINDRICAL_SURFACE ( 'NONE', #31476, 4.999999999999998224 ) ;
#60095 = CARTESIAN_POINT ( 'NONE',  ( 9.234375000614518214, -4.541064518000419881, 2.621784821874995952 ) ) ;
#60096 = FACE_OUTER_BOUND ( 'NONE', #6130, .T. ) ;
#60097 = CARTESIAN_POINT ( 'NONE',  ( 9.562500001229032875, -4.330127018922190985, -2.500000000000001332 ) ) ;
#60098 = CARTESIAN_POINT ( 'NONE',  ( 18.56250000122903288, -4.330127018922190985, -2.500000000000001332 ) ) ;
#60099 = CARTESIAN_POINT ( 'NONE',  ( 14.69062500061451537, -3.027376345333610441, -5.243569643749999898 ) ) ;
#60100 = CARTESIAN_POINT ( 'NONE',  ( 19.49062500061451431, -3.027376345333614438, 5.243569643749998122 ) ) ;
#60101 = CARTESIAN_POINT ( 'NONE',  ( 27.07500000122903216, -5.773502691896255534, -1.060575238724906372E-15 ) ) ;
#60102 = CARTESIAN_POINT ( 'NONE',  ( 3.590625000614518836, 6.054752690667223547, 3.707466751127219781E-16 ) ) ;
#60103 = CARTESIAN_POINT ( 'NONE',  ( 24.18750000000000355, -2.886751345948129988, 4.999999999999997335 ) ) ;
#60104 = CARTESIAN_POINT ( 'NONE',  ( 1.878215178124997609, 14.81562499938548427, 33.25316411605952993 ) ) ;
#60105 = CARTESIAN_POINT ( 'NONE',  ( 26.66250000000000142, 2.886751345948129099, -4.999999999999998224 ) ) ;
#60106 = CARTESIAN_POINT ( 'NONE',  ( 27.27187500061451431, -6.054752690667223547, -1.112240025338166033E-15 ) ) ;
#60107 = CARTESIAN_POINT ( 'NONE',  ( 3.999999999999999112, 17.52499999999999858, 30.00000000000000000 ) ) ;
#60108 = CARTESIAN_POINT ( 'NONE',  ( 12.75000000122903643, -2.886751345948125991, -5.000000000000000000 ) ) ;
#60109 = CARTESIAN_POINT ( 'NONE',  ( 3.712499999999999911, 2.886751345948129099, -4.999999999999998224 ) ) ;
#60110 = CARTESIAN_POINT ( 'NONE',  ( 12.63749999999999574, -2.886751345948181946, -4.999999999999904077 ) ) ;
#60111 = CARTESIAN_POINT ( 'NONE',  ( 7.171875000614517326, 3.027376345333613106, -5.243569643749998122 ) ) ;
#60112 = CARTESIAN_POINT ( 'NONE',  ( 26.65312500061451573, 0.000000000000000000, 5.243569643749999010 ) ) ;
#60113 = CARTESIAN_POINT ( 'NONE',  ( -7.967954043666661671E-16, 13.54062499938548214, 34.33755215474603517 ) ) ;
#60114 = CARTESIAN_POINT ( 'NONE',  ( 22.46250000000000213, -5.773502691896255534, -1.060575238724906372E-15 ) ) ;
#60115 = DIRECTION ( 'NONE',  ( -1.000000000000000000, -0.000000000000000000, -0.000000000000000000 ) ) ;
#60116 = CARTESIAN_POINT ( 'NONE',  ( 4.284375000614518925, -4.541064518000419881, 2.621784821874995952 ) ) ;
#60117 = CARTESIAN_POINT ( 'NONE',  ( 7.734375000614517326, 4.541064518000418104, 2.621784821874999949 ) ) ;
#60118 = CARTESIAN_POINT ( 'NONE',  ( 4.050000000000001599, -4.330127018922190985, -2.500000000000001332 ) ) ;
#60119 = CARTESIAN_POINT ( 'NONE',  ( 2.121784821875001281, 11.85312500061459673, 33.67503911421598417 ) ) ;
#60120 = CARTESIAN_POINT ( 'NONE',  ( 21.22500000000000142, 6.123233995736764310E-16, -4.999999999999998224 ) ) ;
#60121 = CARTESIAN_POINT ( 'NONE',  ( 29.66249999999999432, -5.773502691896255534, -1.060575238724906372E-15 ) ) ;
#60122 = EDGE_CURVE ( 'NONE', #40700, #51146, #52682, .T. ) ;
#60123 = CARTESIAN_POINT ( 'NONE',  ( 3.300000000000000711, 4.330127018922192761, -2.499999999999997780 ) ) ;
#60124 = ORIENTED_EDGE ( 'NONE', *, *, #41327, .T. ) ;
#60125 = CARTESIAN_POINT ( 'NONE',  ( 18.85312500061451502, 4.541064518000418104, -2.621784821874998173 ) ) ;
#60126 = CARTESIAN_POINT ( 'NONE',  ( 11.24062500061451608, 6.054752690667223547, 3.707466751127219781E-16 ) ) ;
#60127 = CARTESIAN_POINT ( 'NONE',  ( 21.72187500061451715, -4.119189519843968306, 2.378215178124996054 ) ) ;
#60128 = CARTESIAN_POINT ( 'NONE',  ( 8.146875000614516082, 6.054752690667223547, 3.707466751127219781E-16 ) ) ;
#60129 = CARTESIAN_POINT ( 'NONE',  ( 22.91249999999999432, -5.773502691896255534, -1.060575238724906372E-15 ) ) ;
#60130 = CARTESIAN_POINT ( 'NONE',  ( 20.10000000122903074, 5.773502691896255534, 3.535250795749688894E-16 ) ) ;
#60131 = CYLINDRICAL_SURFACE ( 'NONE', #6024, 4.999999999999998224 ) ;
#60132 = CARTESIAN_POINT ( 'NONE',  ( 10.02187500061451964, 3.027376345333611329, 5.243569643749999010 ) ) ;
#60133 = CARTESIAN_POINT ( 'NONE',  ( 13.24687500061451750, -3.027376345333614438, 5.243569643749998122 ) ) ;
#60134 = CARTESIAN_POINT ( 'NONE',  ( 24.49687500061451573, -3.027376345333614438, 5.243569643749998122 ) ) ;
#60135 = CARTESIAN_POINT ( 'NONE',  ( 8.625000001229034652, -5.773502691896255534, -1.060575238724906372E-15 ) ) ;
#60136 = CARTESIAN_POINT ( 'NONE',  ( 13.46249999999999858, -5.773502691896255534, -1.060575238724906372E-15 ) ) ;
#60137 = CARTESIAN_POINT ( 'NONE',  ( 18.38437500061451857, 6.421520780324663323E-16, -5.243569643749999010 ) ) ;
#60138 = CARTESIAN_POINT ( 'NONE',  ( 8.671875000614518214, 3.027376345333611329, 5.243569643749999010 ) ) ;
#60139 = CARTESIAN_POINT ( 'NONE',  ( 3.756430356249998770, 19.91562499938548214, 32.16877607737302469 ) ) ;
#60140 = CARTESIAN_POINT ( 'NONE',  ( 20.77500000000000213, 6.123233995736764310E-16, -4.999999999999998224 ) ) ;
#60141 = CARTESIAN_POINT ( 'NONE',  ( -8.484601909799255319E-16, 15.98750000000000249, 34.61880215351700940 ) ) ;
#60142 = CARTESIAN_POINT ( 'NONE',  ( -3.999999999999999112, 17.18750000000000000, 27.69059892324149530 ) ) ;
#60143 = CARTESIAN_POINT ( 'NONE',  ( 25.65937500061451715, 4.119189519843966529, -2.378215178124998275 ) ) ;
#60144 = CARTESIAN_POINT ( 'NONE',  ( 12.29062500061451857, -3.027376345333614438, 5.243569643749998122 ) ) ;
#60145 = CARTESIAN_POINT ( 'NONE',  ( 29.52187500061451431, -6.054752690667223547, -1.112240025338166033E-15 ) ) ;
#60146 =( NAMED_UNIT ( * ) PLANE_ANGLE_UNIT ( ) SI_UNIT ( $, .RADIAN. ) );
#60147 = CARTESIAN_POINT ( 'NONE',  ( 0.000000000000000000, 27.50000000000000000, 26.00000000000000000 ) ) ;
#60148 = CARTESIAN_POINT ( 'NONE',  ( 12.15000000000000036, -4.330127018922190985, -2.500000000000001332 ) ) ;
#60149 = CARTESIAN_POINT ( 'NONE',  ( -3.999999999999999112, 18.31250000122903288, 30.00000000000000000 ) ) ;
#60150 = CARTESIAN_POINT ( 'NONE',  ( 11.58750000122903501, 4.330127018922191873, 2.499999999999999556 ) ) ;
#60151 = CARTESIAN_POINT ( 'NONE',  ( 21.79687500061451644, -3.027376345333614438, 5.243569643749998122 ) ) ;
#60152 = CARTESIAN_POINT ( 'NONE',  ( 16.62187500061451573, 3.027376345333613106, -5.243569643749998122 ) ) ;
#60153 = CARTESIAN_POINT ( 'NONE',  ( -1.071796769724488563, 16.49240381056766580, -26.00000000000000000 ) ) ;
#60154 = VERTEX_POINT ( 'NONE', #25307 ) ;
#60155 = CARTESIAN_POINT ( 'NONE',  ( 16.75312500061451715, 0.000000000000000000, 5.243569643749999010 ) ) ;
#60156 = CARTESIAN_POINT ( 'NONE',  ( 28.50000000122903288, -2.886751345948125991, -5.000000000000000000 ) ) ;
#60157 = CARTESIAN_POINT ( 'NONE',  ( 17.37187500061451573, -6.054752690667223547, -1.112240025338166033E-15 ) ) ;
#60158 = CARTESIAN_POINT ( 'NONE',  ( 3.628125000614518036, 4.541064518000418104, 2.621784821874999949 ) ) ;
#60159 = CARTESIAN_POINT ( 'NONE',  ( 18.32812500061451644, 6.421520780324663323E-16, -5.243569643749999010 ) ) ;
#60160 = CARTESIAN_POINT ( 'NONE',  ( 3.176339285701963888, -3.861459405730729433, 3.176339285701963888 ) ) ;
#60161 = CARTESIAN_POINT ( 'NONE',  ( 27.83437500061451786, 6.421520780324663323E-16, -5.243569643749999010 ) ) ;
#60162 = CARTESIAN_POINT ( 'NONE',  ( 4.243569643749999898, 13.69062500061451537, 32.45002607614398471 ) ) ;
#60163 = CARTESIAN_POINT ( 'NONE',  ( 17.55000000122903359, -2.886751345948129988, 4.999999999999997335 ) ) ;
#60164 = CARTESIAN_POINT ( 'NONE',  ( 10.43437500061451750, 4.119189519843966529, 2.378215178124999607 ) ) ;
#60165 = CARTESIAN_POINT ( 'NONE',  ( 27.06562500061451004, 3.027376345333611329, 5.243569643749999010 ) ) ;
#60166 = CARTESIAN_POINT ( 'NONE',  ( 1.999999999999997335, 18.66874999877096641, 33.46410161513775705 ) ) ;
#60167 = CARTESIAN_POINT ( 'NONE',  ( 20.97187500061451715, -6.054752690667223547, -1.112240025338166033E-15 ) ) ;
#60168 = CARTESIAN_POINT ( 'NONE',  ( 23.55000000122903359, -2.886751345948125991, -5.000000000000000000 ) ) ;
#60169 = ADVANCED_FACE ( 'NONE', ( #16049 ), #50772, .F. ) ;
#60170 = CARTESIAN_POINT ( 'NONE',  ( 22.19062500061451715, -3.027376345333614438, 5.243569643749998122 ) ) ;
#60171 = CARTESIAN_POINT ( 'NONE',  ( 16.65937500061452070, 4.541064518000418104, -2.621784821874998173 ) ) ;
#60172 = CARTESIAN_POINT ( 'NONE',  ( 11.50312500061451892, -4.541064518000417216, -2.621784821875001281 ) ) ;
#60173 = CARTESIAN_POINT ( 'NONE',  ( -4.243569643749999898, 15.80937500061451573, 30.00000000000000000 ) ) ;
#60174 = CARTESIAN_POINT ( 'NONE',  ( 17.35312500061451502, -4.541064518000417216, -2.621784821875001281 ) ) ;
#60175 = CARTESIAN_POINT ( 'NONE',  ( -3.999999999999999112, 17.63749999999999929, 27.69059892324149530 ) ) ;
#60176 = ORIENTED_EDGE ( 'NONE', *, *, #51752, .T. ) ;
#60177 = EDGE_LOOP ( 'NONE', ( #18308, #57903, #49198, #40159 ) ) ;
#60178 = CARTESIAN_POINT ( 'NONE',  ( 22.50000000000000000, -4.330127018922190985, -2.500000000000001332 ) ) ;
#60179 = CARTESIAN_POINT ( 'NONE',  ( 4.243569643749999898, 19.14687500061451431, -27.54997392385601529 ) ) ;
#60180 = CARTESIAN_POINT ( 'NONE',  ( 16.23750000000000071, -2.886751345948237457, -4.999999999999807265 ) ) ;
#60181 = CARTESIAN_POINT ( 'NONE',  ( 24.02812500061451573, -4.541064518000419881, 2.621784821874995952 ) ) ;
#60182 = CARTESIAN_POINT ( 'NONE',  ( 6.440625000614517148, -3.027376345333614438, 5.243569643749998122 ) ) ;
#60183 = CARTESIAN_POINT ( 'NONE',  ( 17.06250000122903288, 0.000000000000000000, 4.999999999999998224 ) ) ;
#60184 = CARTESIAN_POINT ( 'NONE',  ( 21.36562500061451431, -6.054752690667223547, -1.112240025338166033E-15 ) ) ;
#60185 = CARTESIAN_POINT ( 'NONE',  ( 21.82499999999999574, 4.330127018922191873, 2.499999999999999556 ) ) ;
#60186 = CARTESIAN_POINT ( 'NONE',  ( 27.44062500061451715, 6.054752690667223547, 3.707466751127219781E-16 ) ) ;
#60187 = CARTESIAN_POINT ( 'NONE',  ( 7.528125000614515727, 6.421520780324663323E-16, -5.243569643749999010 ) ) ;
#60188 = VERTEX_POINT ( 'NONE', #175 ) ;
#60189 = CARTESIAN_POINT ( 'NONE',  ( 23.27812500061451573, 6.421520780324663323E-16, -5.243569643749999010 ) ) ;
#60190 = CARTESIAN_POINT ( 'NONE',  ( 4.828125000614518214, 6.421520780324663323E-16, -5.243569643749999010 ) ) ;
#60191 = CARTESIAN_POINT ( 'NONE',  ( 10.73437500061451644, 5.824947211148865298E-16, -4.756430356249998326 ) ) ;
#60192 = LINE ( 'NONE', #4071, #17034 ) ;
#60193 = CARTESIAN_POINT ( 'NONE',  ( -3.999999999999999112, 13.81250000122903465, -30.00000000000000000 ) ) ;
#60194 = CARTESIAN_POINT ( 'NONE',  ( -2.000000000000000000, 10.47500000000000142, -33.46410161513775705 ) ) ;
#60195 = CARTESIAN_POINT ( 'NONE',  ( 10.38750000000000107, -2.886751345948125991, -5.000000000000000000 ) ) ;
#60196 = CARTESIAN_POINT ( 'NONE',  ( 12.38437500061451857, -4.541064518000419881, 2.621784821874995952 ) ) ;
#60197 = CARTESIAN_POINT ( 'NONE',  ( 6.750000001229033764, -2.886751345948129988, 4.999999999999997335 ) ) ;
#60198 = CARTESIAN_POINT ( 'NONE',  ( 15.72187500061451892, 3.027376345333613106, -5.243569643749998122 ) ) ;
#60199 = CARTESIAN_POINT ( 'NONE',  ( 5.409375000614516260, 4.541064518000418104, -2.621784821874998173 ) ) ;
#60200 = DIRECTION ( 'NONE',  ( -1.000000000000000000, -0.000000000000000000, -0.000000000000000000 ) ) ;
#60201 = CARTESIAN_POINT ( 'NONE',  ( -5.000000000000000000, 0.000000000000000000, 50.00000000000000000 ) ) ;
#60202 = CARTESIAN_POINT ( 'NONE',  ( 12.34687500061452070, -3.027376345333614438, 5.243569643749998122 ) ) ;
#60203 = LINE ( 'NONE', #49871, #26499 ) ;
#60204 = CARTESIAN_POINT ( 'NONE',  ( 20.91562500061451502, -6.054752690667223547, -1.112240025338166033E-15 ) ) ;
#60205 = CARTESIAN_POINT ( 'NONE',  ( 3.999999999999998668, 11.71250000000000036, 27.69059892324149530 ) ) ;
#60206 = CARTESIAN_POINT ( 'NONE',  ( 9.299999999999998934, 0.000000000000000000, 4.999999999999998224 ) ) ;
#60207 = CARTESIAN_POINT ( 'NONE',  ( 24.30937500061451573, 4.541064518000418104, -2.621784821874998173 ) ) ;
#60208 = CARTESIAN_POINT ( 'NONE',  ( -3.999999999999999112, 13.77500000122903678, -32.30940107675850470 ) ) ;
#60209 = CARTESIAN_POINT ( 'NONE',  ( 3.890625000614517326, -3.027376345333610441, -5.243569643749999898 ) ) ;
#60210 = CARTESIAN_POINT ( 'NONE',  ( 20.93437500061451217, -2.746126346562642428, -4.756430356249999214 ) ) ;
#60211 = CARTESIAN_POINT ( 'NONE',  ( 18.44062500061451715, 6.054752690667223547, 3.707466751127219781E-16 ) ) ;
#60212 = CARTESIAN_POINT ( 'NONE',  ( 13.73437500061451821, -4.541064518000419881, 2.621784821874995952 ) ) ;
#60213 = CARTESIAN_POINT ( 'NONE',  ( 16.72500000000000142, 6.123233995736764310E-16, -4.999999999999998224 ) ) ;
#60214 = CARTESIAN_POINT ( 'NONE',  ( 27.45000000122903572, -2.886751345948129988, 4.999999999999997335 ) ) ;
#60215 = CARTESIAN_POINT ( 'NONE',  ( 5.671875000614519102, -6.054752690667223547, -1.112240025338166033E-15 ) ) ;
#60216 = CARTESIAN_POINT ( 'NONE',  ( 17.07187500061451502, 3.027376345333613106, -5.243569643749998122 ) ) ;
#60217 = CARTESIAN_POINT ( 'NONE',  ( 15.11249999999999893, 2.886751345948126879, 4.999999999999998224 ) ) ;
#60218 = CARTESIAN_POINT ( 'NONE',  ( 24.97499999999999787, 4.330127018922191873, 2.499999999999999556 ) ) ;
#60219 = CARTESIAN_POINT ( 'NONE',  ( 24.38437500061451502, 4.541064518000418104, 2.621784821874999949 ) ) ;
#60220 = CARTESIAN_POINT ( 'NONE',  ( 16.88437500061451502, -4.541064518000419881, 2.621784821874995952 ) ) ;
#60221 = CARTESIAN_POINT ( 'NONE',  ( 3.756430356250000102, 13.65312499938548285, 30.00000000000000000 ) ) ;
#60222 = CARTESIAN_POINT ( 'NONE',  ( 6.825000000000001066, 6.123233995736764310E-16, -4.999999999999998224 ) ) ;
#60223 = CARTESIAN_POINT ( 'NONE',  ( 9.309375000614515727, 2.746126346562645981, -4.756430356249997438 ) ) ;
#60224 = CARTESIAN_POINT ( 'NONE',  ( 18.70312500061451644, -4.541064518000417216, -2.621784821875001281 ) ) ;
#60225 = CARTESIAN_POINT ( 'NONE',  ( 10.27499999999999858, -4.330127018922194537, 2.499999999999995559 ) ) ;
#60226 =( BOUNDED_CURVE ( )  B_SPLINE_CURVE ( 2, ( #63445, #25271, #47818, #56802, #12831, #19725, #42276 ),
 .UNSPECIFIED., .F., .F. ) 
 B_SPLINE_CURVE_WITH_KNOTS ( ( 3, 2, 2, 3 ),
 ( 0.9855112084356887348, 0.9861111111111111605, 0.9888888888888889284, 0.9894149656234122459 ),
 .UNSPECIFIED. ) 
 CURVE ( )  GEOMETRIC_REPRESENTATION_ITEM ( )  RATIONAL_B_SPLINE_CURVE ( ( 0.9546297447238953904, 0.9710661812649934443, 1.000000000000000000, 0.8660254037844387076, 1.000000000000000000, 0.9746268694889814732, 0.9588644528015497492 ) ) 
 REPRESENTATION_ITEM ( '' )  );
#60227 = CARTESIAN_POINT ( 'NONE',  ( 3.440625000614518036, -3.027376345333610441, -5.243569643749999898 ) ) ;
#60228 = CARTESIAN_POINT ( 'NONE',  ( 18.45000000000000284, -4.330127018922190985, -2.500000000000001332 ) ) ;
#60229 = CARTESIAN_POINT ( 'NONE',  ( 19.00312500061451715, 0.000000000000000000, 5.243569643749999010 ) ) ;
#60230 = CARTESIAN_POINT ( 'NONE',  ( 14.66249999999999964, 2.886751345948182834, 4.999999999999902300 ) ) ;
#60231 = CARTESIAN_POINT ( 'NONE',  ( 22.16250000122903074, -4.330127018922190985, -2.500000000000001332 ) ) ;
#60232 = CARTESIAN_POINT ( 'NONE',  ( 15.03749999999999964, 5.773502691896255534, 3.535250795749688401E-16 ) ) ;
#60233 = CARTESIAN_POINT ( 'NONE',  ( 28.95937500061451431, 0.000000000000000000, 5.243569643749999010 ) ) ;
#60234 = EDGE_LOOP ( 'NONE', ( #38244, #11264, #43054, #53840 ) ) ;
#60235 = CARTESIAN_POINT ( 'NONE',  ( 17.87812500061451715, 6.421520780324663323E-16, -5.243569643749999010 ) ) ;
#60236 = CARTESIAN_POINT ( 'NONE',  ( 24.06562500061451715, -6.054752690667223547, -1.112240025338166033E-15 ) ) ;
#60237 = CARTESIAN_POINT ( 'NONE',  ( 25.24687500061451573, 6.054752690667223547, 3.707466751127219781E-16 ) ) ;
#60238 = CARTESIAN_POINT ( 'NONE',  ( 8.025000000000000355, -4.330127018922194537, 2.499999999999995559 ) ) ;
#60239 = CARTESIAN_POINT ( 'NONE',  ( 11.69062500061451360, 6.054752690667223547, 3.707466751127219781E-16 ) ) ;
#60240 = CARTESIAN_POINT ( 'NONE',  ( 26.54062500061451146, 6.054752690667223547, 3.707466751127219781E-16 ) ) ;
#60241 = CARTESIAN_POINT ( 'NONE',  ( 16.50937500061451502, -4.541064518000417216, -2.621784821875001281 ) ) ;
#60242 = CARTESIAN_POINT ( 'NONE',  ( 19.77187500061451786, 3.027376345333613106, -5.243569643749998122 ) ) ;
#60243 = CARTESIAN_POINT ( 'NONE',  ( 7.050000001229036251, 5.773502691896255534, 3.535250795749688401E-16 ) ) ;
#60244 = CARTESIAN_POINT ( 'NONE',  ( 4.243569643749999010, 10.67187500061451644, 27.54997392385601174 ) ) ;
#60245 = CARTESIAN_POINT ( 'NONE',  ( 23.55000000122903359, -2.886751345948125991, -5.000000000000000000 ) ) ;
#60246 = CARTESIAN_POINT ( 'NONE',  ( 18.19687500061451502, -2.746126346562646425, 4.756430356249996549 ) ) ;
#60247 = CARTESIAN_POINT ( 'NONE',  ( 13.90312500061451750, 4.541064518000418104, -2.621784821874998173 ) ) ;
#60248 = CARTESIAN_POINT ( 'NONE',  ( 7.321875000614516793, 3.027376345333611329, 5.243569643749999010 ) ) ;
#60249 = CARTESIAN_POINT ( 'NONE',  ( 7.471875000614519813, -6.054752690667223547, -1.112240025338166033E-15 ) ) ;
#60250 = EDGE_LOOP ( 'NONE', ( #64733, #58813, #27850, #26225 ) ) ;
#60251 = CARTESIAN_POINT ( 'NONE',  ( 1.071796769724491893, 13.38259618943233598, 33.99999999999999289 ) ) ;
#60252 = CARTESIAN_POINT ( 'NONE',  ( 20.42812500061451431, -4.541064518000419881, 2.621784821874995952 ) ) ;
#60253 = EDGE_CURVE ( 'NONE', #63581, #2667, #50336, .T. ) ;
#60254 = CARTESIAN_POINT ( 'NONE',  ( 23.70937500061451786, -4.541064518000417216, -2.621784821875001281 ) ) ;
#60255 = CARTESIAN_POINT ( 'NONE',  ( 20.69062500061451715, 6.054752690667223547, 3.707466751127219781E-16 ) ) ;
#60256 = CARTESIAN_POINT ( 'NONE',  ( 3.999999999999999112, 12.12500000000000000, 30.00000000000000000 ) ) ;
#60257 = CARTESIAN_POINT ( 'NONE',  ( 26.69062500061451715, -3.027376345333614438, 5.243569643749998122 ) ) ;
#60258 = CARTESIAN_POINT ( 'NONE',  ( 6.525000001229033231, 2.886751345948129099, -4.999999999999998224 ) ) ;
#60259 = VERTEX_POINT ( 'NONE', #27152 ) ;
#60260 = CARTESIAN_POINT ( 'NONE',  ( 2.737500001229034474, -4.330127018922194537, 2.499999999999995559 ) ) ;
#60261 = CARTESIAN_POINT ( 'NONE',  ( -3.999999999999999556, 15.46250000000000036, -32.30940107675850470 ) ) ;
#60262 = CARTESIAN_POINT ( 'NONE',  ( 22.46250000122903501, 0.000000000000000000, 4.999999999999998224 ) ) ;
#60263 = CARTESIAN_POINT ( 'NONE',  ( 3.756430356249998770, 14.51562499938548356, 32.16877607737302469 ) ) ;
#60264 = CARTESIAN_POINT ( 'NONE',  ( 6.871875000614517504, 3.027376345333611329, 5.243569643749999010 ) ) ;
#60265 = CARTESIAN_POINT ( 'NONE',  ( 12.90000000000000213, 0.000000000000000000, 4.999999999999998224 ) ) ;
#60266 = CARTESIAN_POINT ( 'NONE',  ( 11.54062500061451857, -3.027376345333610441, -5.243569643749999898 ) ) ;
#60267 = CARTESIAN_POINT ( 'NONE',  ( 7.396875000614519635, -3.027376345333614438, 5.243569643749998122 ) ) ;
#60268 = CARTESIAN_POINT ( 'NONE',  ( 27.82500000122903572, 2.886751345948126879, 4.999999999999999112 ) ) ;
#60269 = CARTESIAN_POINT ( 'NONE',  ( 14.48437500061451821, 4.541064518000418104, 2.621784821874999949 ) ) ;
#60270 = CARTESIAN_POINT ( 'NONE',  ( 4.509375000614518569, 4.541064518000418104, -2.621784821874998173 ) ) ;
#60271 = CARTESIAN_POINT ( 'NONE',  ( 29.43750000000000000, 5.773502691896255534, 3.535250795749688894E-16 ) ) ;
#60272 = CARTESIAN_POINT ( 'NONE',  ( 5.390625000614518214, 6.054752690667223547, 3.707466751127219781E-16 ) ) ;
#60273 = CARTESIAN_POINT ( 'NONE',  ( 14.46562500061451750, 3.027376345333611329, 5.243569643749999010 ) ) ;
#60274 = ORIENTED_EDGE ( 'NONE', *, *, #59537, .T. ) ;
#60275 = CARTESIAN_POINT ( 'NONE',  ( 11.39062500061451644, -3.027376345333614438, 5.243569643749998122 ) ) ;
#60276 = CARTESIAN_POINT ( 'NONE',  ( 5.137500001229033941, 6.123233995736764310E-16, -4.999999999999998224 ) ) ;
#60277 = CARTESIAN_POINT ( 'NONE',  ( 8.653125000614515727, 0.000000000000000000, 5.243569643749999010 ) ) ;
#60278 = CARTESIAN_POINT ( 'NONE',  ( 20.85937500061451644, 0.000000000000000000, 4.756430356249998326 ) ) ;
#60279 = CARTESIAN_POINT ( 'NONE',  ( 9.412499999999999645, -5.773502691896255534, -1.060575238724906372E-15 ) ) ;
#60280 = CARTESIAN_POINT ( 'NONE',  ( 4.725000001229034297, 2.886751345948129099, -4.999999999999998224 ) ) ;
#60281 = CARTESIAN_POINT ( 'NONE',  ( 17.17500000000000071, 6.123233995736764310E-16, -4.999999999999998224 ) ) ;
#60282 =( BOUNDED_CURVE ( )  B_SPLINE_CURVE ( 2, ( #39011, #50094, #61170, #45644, #28640, #68177, #17540 ),
 .UNSPECIFIED., .F., .F. ) 
 B_SPLINE_CURVE_WITH_KNOTS ( ( 3, 2, 2, 3 ),
 ( 0.3099999999999999978, 0.3133333333333333526, 0.3166666666666665964, 0.3199999999999999512 ),
 .UNSPECIFIED. ) 
 CURVE ( )  GEOMETRIC_REPRESENTATION_ITEM ( )  RATIONAL_B_SPLINE_CURVE ( ( 1.000000000000000000, 0.8660254037844387076, 1.000000000000000000, 0.8660254037844387076, 1.000000000000000000, 0.8660254037844409281, 0.9999999999999977796 ) ) 
 REPRESENTATION_ITEM ( '' )  );
#60283 = CARTESIAN_POINT ( 'NONE',  ( 18.68437500061451928, -4.541064518000419881, 2.621784821874995952 ) ) ;
#60284 = CARTESIAN_POINT ( 'NONE',  ( 13.42500000122903536, 2.886751345948126879, 4.999999999999999112 ) ) ;
#60285 = CARTESIAN_POINT ( 'NONE',  ( 23.13749999999999929, 5.773502691896255534, 3.535250795749688894E-16 ) ) ;
#60286 = CARTESIAN_POINT ( 'NONE',  ( 4.243569643749999010, 16.01562500061451644, -32.45002607614398471 ) ) ;
#60287 = CARTESIAN_POINT ( 'NONE',  ( 1.071796769724479237, 20.24240381056766935, 25.99999999999999645 ) ) ;
#60288 = CARTESIAN_POINT ( 'NONE',  ( 34.99999999999999289, -2.499999999999999556, 3.499999999999999556 ) ) ;
#60289 = CARTESIAN_POINT ( 'NONE',  ( 22.63125000122903430, 6.123233995736764310E-16, -4.999999999999998224 ) ) ;
#60290 = DIRECTION ( 'NONE',  ( -1.000000000000000000, -0.000000000000000000, -0.000000000000000000 ) ) ;
#60291 = CARTESIAN_POINT ( 'NONE',  ( 18.69375000122903430, 5.773502691896255534, 3.535250795749688401E-16 ) ) ;
#60292 = CARTESIAN_POINT ( 'NONE',  ( 16.77187500061451786, 3.027376345333611329, 5.243569643749999010 ) ) ;
#60293 = CARTESIAN_POINT ( 'NONE',  ( 27.18750000000000000, 5.773502691896255534, 3.535250795749688894E-16 ) ) ;
#60294 = EDGE_CURVE ( 'NONE', #9597, #37881, #44876, .T. ) ;
#60295 = CARTESIAN_POINT ( 'NONE',  ( 11.27812500061451573, 4.541064518000418104, 2.621784821874999949 ) ) ;
#60296 = CARTESIAN_POINT ( 'NONE',  ( 28.92187500061451644, -4.119189519843968306, 2.378215178124996054 ) ) ;
#60297 = CARTESIAN_POINT ( 'NONE',  ( 22.47187500061451715, 3.027376345333613106, -5.243569643749998122 ) ) ;
#60298 = CARTESIAN_POINT ( 'NONE',  ( 13.58437500061451431, -2.746126346562646425, 4.756430356249996549 ) ) ;
#60299 = CARTESIAN_POINT ( 'NONE',  ( 6.553125000614518747, -4.541064518000417216, -2.621784821875001281 ) ) ;
#60300 = CARTESIAN_POINT ( 'NONE',  ( 13.77187500061451786, -6.054752690667223547, -1.112240025338166033E-15 ) ) ;
#60301 = VERTEX_POINT ( 'NONE', #50417 ) ;
#60302 = CARTESIAN_POINT ( 'NONE',  ( 23.59687500061451715, -3.027376345333614438, 5.243569643749998122 ) ) ;
#60303 = CYLINDRICAL_SURFACE ( 'NONE', #47746, 4.999999999999998224 ) ;
#60304 = CARTESIAN_POINT ( 'NONE',  ( 28.75312500061451715, 4.541064518000418104, -2.621784821874998173 ) ) ;
#60305 = CARTESIAN_POINT ( 'NONE',  ( 24.75000000000000000, -4.330127018922190985, -2.500000000000001332 ) ) ;
#60306 = CARTESIAN_POINT ( 'NONE',  ( 7.312500000000000000, 2.886751345948129099, -4.999999999999998224 ) ) ;
#60307 = CARTESIAN_POINT ( 'NONE',  ( 17.21250000122903145, -4.330127018922190985, -2.500000000000001332 ) ) ;
#60308 = CARTESIAN_POINT ( 'NONE',  ( 45.00000000000000000, 0.000000000000000000, 4.999999999999998224 ) ) ;
#60309 = CARTESIAN_POINT ( 'NONE',  ( 9.196875000614515017, -4.119189519843965641, -2.378215178125001383 ) ) ;
#60310 = COLOUR_RGB ( '',0.8941176470588234615, 0.8941176470588234615, 0.8941176470588234615 ) ;
#60311 = VERTEX_POINT ( 'NONE', #38966 ) ;
#60312 = CARTESIAN_POINT ( 'NONE',  ( 15.75000000000000000, -4.330127018922190985, -2.500000000000001332 ) ) ;
#60313 = CARTESIAN_POINT ( 'NONE',  ( 19.27500000000000213, -4.330127018922194537, 2.499999999999995559 ) ) ;
#60314 = CARTESIAN_POINT ( 'NONE',  ( 10.82812500061451644, 4.541064518000418104, 2.621784821874999949 ) ) ;
#60315 = ORIENTED_EDGE ( 'NONE', *, *, #69831, .T. ) ;
#60316 = CARTESIAN_POINT ( 'NONE',  ( 26.32499999999999929, 4.330127018922191873, 2.499999999999999556 ) ) ;
#60317 = CARTESIAN_POINT ( 'NONE',  ( 9.001249775931846008E-16, 16.82187500061451857, -25.09994784771203058 ) ) ;
#60318 = CARTESIAN_POINT ( 'NONE',  ( 2.803125000614518747, 0.000000000000000000, 5.243569643749999010 ) ) ;
#60319 = CARTESIAN_POINT ( 'NONE',  ( 4.648177544792955741E-15, 14.18750000000000000, 33.99999999999999289 ) ) ;
#60320 = CARTESIAN_POINT ( 'NONE',  ( 9.600000000000001421, 4.330127018922192761, -2.499999999999997780 ) ) ;
#60321 = CARTESIAN_POINT ( 'NONE',  ( 3.727827348360245097, 3.332161949968362347, -3.727827348360304605 ) ) ;
#60322 = VERTEX_POINT ( 'NONE', #5705 ) ;
#60323 = CARTESIAN_POINT ( 'NONE',  ( -3.000416591977282496E-16, 12.04062500061451857, 25.09994784771203058 ) ) ;
#60324 = CARTESIAN_POINT ( 'NONE',  ( 25.07812500061451644, 6.421520780324663323E-16, -5.243569643749999010 ) ) ;
#60325 = CARTESIAN_POINT ( 'NONE',  ( 4.206174892561018730, -2.703348437251418268, 4.492986738870575536 ) ) ;
#60326 = CARTESIAN_POINT ( 'NONE',  ( 3.756430356250000546, 20.32812499938548356, 27.83122392262697886 ) ) ;
#60327 = CARTESIAN_POINT ( 'NONE',  ( 21.57187500061451502, 3.027376345333613106, -5.243569643749998122 ) ) ;
#60328 = EDGE_CURVE ( 'NONE', #58564, #43716, #67411, .T. ) ;
#60329 = CARTESIAN_POINT ( 'NONE',  ( 19.15312500061451573, -4.541064518000417216, -2.621784821875001281 ) ) ;
#60330 = CARTESIAN_POINT ( 'NONE',  ( -4.243569643749999898, 13.95312500061459282, -30.00000000000000000 ) ) ;
#60331 = CARTESIAN_POINT ( 'NONE',  ( 22.20000000122903216, -2.886751345948125991, -5.000000000000000000 ) ) ;
#60332 = CARTESIAN_POINT ( 'NONE',  ( 4.153125000614515727, 0.000000000000000000, 5.243569643749999010 ) ) ;
#60333 = CARTESIAN_POINT ( 'NONE',  ( 25.05937500061451573, -4.119189519843965641, -2.378215178125001383 ) ) ;
#60334 = CARTESIAN_POINT ( 'NONE',  ( 20.99062500061451431, -3.027376345333610441, -5.243569643749999898 ) ) ;
#60335 = CARTESIAN_POINT ( 'NONE',  ( 9.009375000614518569, 4.119189519843966529, -2.378215178124998275 ) ) ;
#60336 = CARTESIAN_POINT ( 'NONE',  ( -1.878215178124999163, 17.74062499938548498, 26.74683588394047007 ) ) ;
#60337 = CARTESIAN_POINT ( 'NONE',  ( 15.04687500061451644, -3.027376345333614438, 5.243569643749998122 ) ) ;
#60338 = CARTESIAN_POINT ( 'NONE',  ( 13.28437500061451715, -4.541064518000419881, 2.621784821874995952 ) ) ;
#60339 = CARTESIAN_POINT ( 'NONE',  ( 23.40937500061451715, 4.541064518000418104, -2.621784821874998173 ) ) ;
#60340 = CARTESIAN_POINT ( 'NONE',  ( 4.243569643749999898, 11.53437500061451892, 30.00000000000000000 ) ) ;
#60341 = CARTESIAN_POINT ( 'NONE',  ( 5.953125000614519102, 0.000000000000000000, 5.243569643749999010 ) ) ;
#60342 = CARTESIAN_POINT ( 'NONE',  ( 29.50312500061451360, -4.541064518000417216, -2.621784821875001281 ) ) ;
#60343 = CARTESIAN_POINT ( 'NONE',  ( 27.62812500061451360, -4.541064518000419881, 2.621784821874995952 ) ) ;
#60344 = CARTESIAN_POINT ( 'NONE',  ( 1.071796769724490339, 19.52990381179669654, -34.00000000000000000 ) ) ;
#60345 = CARTESIAN_POINT ( 'NONE',  ( -3.999999999999999112, 18.19999999999999929, 30.00000000000000000 ) ) ;
#60346 = CARTESIAN_POINT ( 'NONE',  ( 6.496875000614517504, -3.027376345333614438, 5.243569643749998122 ) ) ;
#60347 = SHAPE_DEFINITION_REPRESENTATION ( #11961, #68023 ) ;
#60348 = CARTESIAN_POINT ( 'NONE',  ( 14.88750000122903394, -4.330127018922194537, 2.499999999999995559 ) ) ;
#60349 = CARTESIAN_POINT ( 'NONE',  ( 10.27500000122903323, 2.886751345948126879, 4.999999999999999112 ) ) ;
#60350 = CARTESIAN_POINT ( 'NONE',  ( 28.53750000122903074, 6.123233995736764310E-16, -4.999999999999998224 ) ) ;
#60351 = CARTESIAN_POINT ( 'NONE',  ( 2.828200636599751609E-16, 15.70624999877096606, 25.38119784648299415 ) ) ;
#60352 = CARTESIAN_POINT ( 'NONE',  ( 17.49375000122903145, -2.886751345948129988, 4.999999999999997335 ) ) ;
#60353 = CARTESIAN_POINT ( 'NONE',  ( 13.35937500061451821, -4.541064518000417216, -2.621784821875001281 ) ) ;
#60354 = LINE ( 'NONE', #9038, #57309 ) ;
#60355 = ORIENTED_EDGE ( 'NONE', *, *, #25207, .F. ) ;
#60356 = CARTESIAN_POINT ( 'NONE',  ( 20.87812500061451715, -4.541064518000419881, 2.621784821874995952 ) ) ;
#60357 = CARTESIAN_POINT ( 'NONE',  ( 6.665625000614515905, 3.027376345333613106, -5.243569643749998122 ) ) ;
#60358 = CARTESIAN_POINT ( 'NONE',  ( 24.15937500061451715, -4.541064518000417216, -2.621784821875001281 ) ) ;
#60359 = CARTESIAN_POINT ( 'NONE',  ( 8.465625000614515727, 3.027376345333613106, -5.243569643749998122 ) ) ;
#60360 = CARTESIAN_POINT ( 'NONE',  ( -4.000000000000000000, 16.26874999877096784, 30.00000000000000000 ) ) ;
#60361 = CARTESIAN_POINT ( 'NONE',  ( 7.837500001229035007, 6.123233995736764310E-16, -4.999999999999998224 ) ) ;
#60362 = EDGE_CURVE ( 'NONE', #50794, #31197, #39795, .T. ) ;
#60363 = CARTESIAN_POINT ( 'NONE',  ( 23.20312500061451644, -4.541064518000417216, -2.621784821875001281 ) ) ;
#60364 = CARTESIAN_POINT ( 'NONE',  ( 2.000000000000001332, 18.01250000122903572, -26.53589838486224650 ) ) ;
#60365 = CARTESIAN_POINT ( 'NONE',  ( 10.35000000122903074, -2.886751345948129988, 4.999999999999997335 ) ) ;
#60366 = CARTESIAN_POINT ( 'NONE',  ( 20.46562500061451928, -6.054752690667223547, -1.112240025338166033E-15 ) ) ;
#60367 = CARTESIAN_POINT ( 'NONE',  ( 15.70312500061451644, 4.541064518000418104, -2.621784821874998173 ) ) ;
#60368 = CARTESIAN_POINT ( 'NONE',  ( 28.95937500061451431, 0.000000000000000000, 4.756430356249998326 ) ) ;
#60369 = CARTESIAN_POINT ( 'NONE',  ( 15.59999999999999964, 0.000000000000000000, 4.999999999999998224 ) ) ;
#60370 = CARTESIAN_POINT ( 'NONE',  ( 11.70000000122903216, -2.886751345948129988, 4.999999999999997335 ) ) ;
#60371 = CARTESIAN_POINT ( 'NONE',  ( 8.878125000614515372, 6.421520780324663323E-16, -5.243569643749999010 ) ) ;
#60372 = AXIS2_PLACEMENT_3D ( 'NONE', #18264, #29735, #49291 ) ;
#60373 = CARTESIAN_POINT ( 'NONE',  ( 10.97812500061451679, -4.541064518000419881, 2.621784821874995952 ) ) ;
#60374 = VECTOR ( 'NONE', #71468, 1000.000000000000000 ) ;
#60375 = CARTESIAN_POINT ( 'NONE',  ( 20.36250000122903359, -4.330127018922190985, -2.500000000000001332 ) ) ;
#60376 = CARTESIAN_POINT ( 'NONE',  ( 19.24687500061452283, -3.027376345333610441, -5.243569643749999898 ) ) ;
#60377 = CARTESIAN_POINT ( 'NONE',  ( -1.999999999999999112, 18.50000000000000000, 26.53589838486224650 ) ) ;
#60378 = CARTESIAN_POINT ( 'NONE',  ( 4.162500001229033408, -4.330127018922190985, -2.500000000000001332 ) ) ;
#60379 = CARTESIAN_POINT ( 'NONE',  ( 3.346875000614518036, -3.027376345333614438, 5.243569643749998122 ) ) ;
#60380 = CARTESIAN_POINT ( 'NONE',  ( 22.13437500061451502, 4.541064518000418104, 2.621784821874999949 ) ) ;
#60381 = CARTESIAN_POINT ( 'NONE',  ( 27.63749999999999929, 5.773502691896255534, 3.535250795749688401E-16 ) ) ;
#60382 = CARTESIAN_POINT ( 'NONE',  ( 18.40312500061451573, 4.541064518000418104, -2.621784821874998173 ) ) ;
#60383 = CARTESIAN_POINT ( 'NONE',  ( 23.25937500061451857, -4.541064518000417216, -2.621784821875001281 ) ) ;
#60384 = CARTESIAN_POINT ( 'NONE',  ( -3.756430356250000102, 20.17812499938548143, 30.00000000000000000 ) ) ;
#60385 = FACE_OUTER_BOUND ( 'NONE', #73110, .T. ) ;
#60386 = CARTESIAN_POINT ( 'NONE',  ( 29.52187500061451431, -6.054752690667223547, -1.112240025338166033E-15 ) ) ;
#60387 = CARTESIAN_POINT ( 'NONE',  ( 21.64687500061451431, 0.000000000000000000, 4.756430356249998326 ) ) ;
#60388 = CARTESIAN_POINT ( 'NONE',  ( 15.59062500061451573, -3.027376345333610441, -5.243569643749999898 ) ) ;
#60389 = CARTESIAN_POINT ( 'NONE',  ( 13.88437500061451679, 6.421520780324663323E-16, -5.243569643749999010 ) ) ;
#60390 = ORIENTED_EDGE ( 'NONE', *, *, #8224, .T. ) ;
#60391 = CARTESIAN_POINT ( 'NONE',  ( 9.074999999999999289, 6.123233995736764310E-16, -4.999999999999998224 ) ) ;
#60392 = CARTESIAN_POINT ( 'NONE',  ( 23.80312500061451786, 4.541064518000418104, -2.621784821874998173 ) ) ;
#60393 = CARTESIAN_POINT ( 'NONE',  ( 1.592000809091587073E-14, 17.18750000000000355, 26.00000000000000000 ) ) ;
#60394 = CARTESIAN_POINT ( 'NONE',  ( 65.00000000000000000, -6.363961030678871644, 6.363961030678982667 ) ) ;
#60395 = CARTESIAN_POINT ( 'NONE',  ( 14.66249999999999964, 2.886751345948126879, 4.999999999999999112 ) ) ;
#60396 = CARTESIAN_POINT ( 'NONE',  ( 24.26250000122903216, 0.000000000000000000, 4.999999999999998224 ) ) ;
#60397 = CARTESIAN_POINT ( 'NONE',  ( 19.04062500061451146, -3.027376345333614438, 5.243569643749998122 ) ) ;
#60398 = ORIENTED_EDGE ( 'NONE', *, *, #55968, .T. ) ;
#60399 = CARTESIAN_POINT ( 'NONE',  ( 22.57499999999999929, 6.123233995736764310E-16, -4.999999999999998224 ) ) ;
#60400 = ADVANCED_FACE ( 'NONE', ( #67052 ), #49686, .F. ) ;
#60401 = CARTESIAN_POINT ( 'NONE',  ( 23.48437500061451644, 4.541064518000418104, 2.621784821874999949 ) ) ;
#60402 = ORIENTED_EDGE ( 'NONE', *, *, #36932, .F. ) ;
#60403 = CARTESIAN_POINT ( 'NONE',  ( 11.69062500061451360, 6.054752690667223547, 3.707466751127219781E-16 ) ) ;
#60404 = CARTESIAN_POINT ( 'NONE',  ( 2.803125000614518747, 0.000000000000000000, 5.243569643749999010 ) ) ;
#60405 = CARTESIAN_POINT ( 'NONE',  ( 15.30937500061451573, 2.746126346562643317, 4.756430356249998326 ) ) ;
#60406 = CARTESIAN_POINT ( 'NONE',  ( 26.50312500061451360, 4.541064518000418104, -2.621784821874998173 ) ) ;
#60407 = CARTESIAN_POINT ( 'NONE',  ( 17.84999999999999787, 0.000000000000000000, 4.999999999999998224 ) ) ;
#60408 = CARTESIAN_POINT ( 'NONE',  ( 24.97499999999999787, 4.330127018922191873, 2.499999999999999556 ) ) ;
#60409 = CARTESIAN_POINT ( 'NONE',  ( 4.243569643749999898, 19.12812500061451715, 30.00000000000000000 ) ) ;
#60410 = CARTESIAN_POINT ( 'NONE',  ( 5.971875000614516260, 3.027376345333611329, 5.243569643749999010 ) ) ;
#60411 = CARTESIAN_POINT ( 'NONE',  ( 16.50937500061451502, -4.541064518000417216, -2.621784821875001281 ) ) ;
#60412 = CARTESIAN_POINT ( 'NONE',  ( 28.20937500061451786, -4.541064518000417216, -2.621784821875001281 ) ) ;
#60413 = ORIENTED_EDGE ( 'NONE', *, *, #20857, .T. ) ;
#60414 = CARTESIAN_POINT ( 'NONE',  ( 27.14062500061451644, -3.027376345333614438, 5.243569643749998122 ) ) ;
#60415 = CARTESIAN_POINT ( 'NONE',  ( 28.09687500061451360, -3.027376345333614438, 5.243569643749998122 ) ) ;
#60416 = CARTESIAN_POINT ( 'NONE',  ( 3.309375000614518836, 0.000000000000000000, 5.243569643749999010 ) ) ;
#60417 = CARTESIAN_POINT ( 'NONE',  ( 12.59999999999999964, -4.330127018922190985, -2.500000000000001332 ) ) ;
#60418 = CARTESIAN_POINT ( 'NONE',  ( 11.69062500061451360, 6.054752690667223547, 3.707466751127219781E-16 ) ) ;
#60419 = CARTESIAN_POINT ( 'NONE',  ( 9.431250001229033231, -4.330127018922194537, 2.499999999999995559 ) ) ;
#60420 = CARTESIAN_POINT ( 'NONE',  ( 19.57500000000000284, 4.330127018922191873, 2.499999999999999556 ) ) ;
#60421 = CARTESIAN_POINT ( 'NONE',  ( 28.34062500061451928, 6.054752690667223547, 3.707466751127219781E-16 ) ) ;
#60422 = CARTESIAN_POINT ( 'NONE',  ( 15.37500000122903465, -5.773502691896255534, -1.060575238724906372E-15 ) ) ;
#60423 = DIRECTION ( 'NONE',  ( 1.000000000000000000, 0.000000000000000000, 0.000000000000000000 ) ) ;
#60424 = CARTESIAN_POINT ( 'NONE',  ( 16.24687500061451573, 5.492252693125287522, 3.363034840372157021E-16 ) ) ;
#60425 = CARTESIAN_POINT ( 'NONE',  ( 5.653125000614517504, -4.541064518000417216, -2.621784821875001281 ) ) ;
#60426 = CARTESIAN_POINT ( 'NONE',  ( 21.53437500061451715, 6.421520780324663323E-16, -5.243569643749999010 ) ) ;
#60427 = CARTESIAN_POINT ( 'NONE',  ( -3.000416591977282496E-16, 16.14687500061451431, 25.09994784771203058 ) ) ;
#60428 = CARTESIAN_POINT ( 'NONE',  ( 22.35937500061451644, -4.541064518000417216, -2.621784821875001281 ) ) ;
#60429 = CARTESIAN_POINT ( 'NONE',  ( 4.012500000000001954, -5.773502691896255534, -1.060575238724906372E-15 ) ) ;
#60430 = CARTESIAN_POINT ( 'NONE',  ( 4.000000000000000000, 11.30000000122903536, 32.30940107675849049 ) ) ;
#60431 = CARTESIAN_POINT ( 'NONE',  ( 11.76562500061451644, 3.027376345333611329, 5.243569643749999010 ) ) ;
#60432 = CARTESIAN_POINT ( 'NONE',  ( 4.087500001229035007, -4.330127018922194537, 2.499999999999995559 ) ) ;
#60433 = VECTOR ( 'NONE', #40023, 1000.000000000000000 ) ;
#60434 = CARTESIAN_POINT ( 'NONE',  ( 8.596875000614518925, 6.054752690667223547, 3.707466751127219781E-16 ) ) ;
#60435 = CARTESIAN_POINT ( 'NONE',  ( 12.99375000122903323, -2.886751345948130876, 4.999999999999996447 ) ) ;
#60436 = CARTESIAN_POINT ( 'NONE',  ( 9.553125000614517859, 0.000000000000000000, 5.243569643749999010 ) ) ;
#60437 = CARTESIAN_POINT ( 'NONE',  ( 14.63437500061451679, -4.541064518000419881, 2.621784821874995952 ) ) ;
#60438 = CARTESIAN_POINT ( 'NONE',  ( 25.64999999999999858, -4.330127018922190985, -2.500000000000001332 ) ) ;
#60439 = CARTESIAN_POINT ( 'NONE',  ( 22.35000000122903074, 5.773502691896255534, 3.535250795749688894E-16 ) ) ;
#60440 = CARTESIAN_POINT ( 'NONE',  ( 7.584375000614516082, 6.421520780324663323E-16, -5.243569643749999010 ) ) ;
#60441 = CARTESIAN_POINT ( 'NONE',  ( 12.25312500061451537, 0.000000000000000000, 5.243569643749999010 ) ) ;
#60442 = CARTESIAN_POINT ( 'NONE',  ( 24.99375000122903145, 5.773502691896255534, 3.535250795749688894E-16 ) ) ;
#60443 = CARTESIAN_POINT ( 'NONE',  ( 22.65937500061451715, 0.000000000000000000, 5.243569643749999010 ) ) ;
#60444 = CARTESIAN_POINT ( 'NONE',  ( 14.21249999999999858, 2.886751345948193936, 4.999999999999883649 ) ) ;
#60445 = EDGE_CURVE ( 'NONE', #34725, #28470, #47953, .T. ) ;
#60446 = CARTESIAN_POINT ( 'NONE',  ( -0.5556303621801399473, 4.970948098741851950, 26.03636520952240474 ) ) ;
#60447 = DIRECTION ( 'NONE',  ( -0.000000000000000000, -1.000000000000000000, -0.000000000000000000 ) ) ;
#60448 = CARTESIAN_POINT ( 'NONE',  ( -4.243569643749999898, 11.30937500061451928, -30.00000000000000000 ) ) ;
#60449 =( BOUNDED_CURVE ( )  B_SPLINE_CURVE ( 2, ( #66871, #39151, #10346, #32515, #44705, #67240, #4810, #27342, #21779 ),
 .UNSPECIFIED., .F., .F. ) 
 B_SPLINE_CURVE_WITH_KNOTS ( ( 3, 2, 2, 2, 3 ),
 ( 0.6847826086956522174, 0.6884057971014492239, 0.6956521739130434590, 0.7028985507246376940, 0.7065217391304348116 ),
 .UNSPECIFIED. ) 
 CURVE ( )  GEOMETRIC_REPRESENTATION_ITEM ( )  RATIONAL_B_SPLINE_CURVE ( ( 0.9330127018922192983, 0.9330127018922202975, 1.000000000000000000, 0.8660254037844387076, 1.000000000000000000, 0.8660254037844387076, 1.000000000000000000, 0.9330127018922194093, 0.9330127018922194093 ) ) 
 REPRESENTATION_ITEM ( '' )  );
#60450 = CARTESIAN_POINT ( 'NONE',  ( 16.46250000122903501, 4.330127018922192761, -2.499999999999997780 ) ) ;
#60451 = CARTESIAN_POINT ( 'NONE',  ( -4.243569643749999898, 18.45312500061451644, -30.00000000000000000 ) ) ;
#60452 = CARTESIAN_POINT ( 'NONE',  ( 16.61250000122903359, 0.000000000000000000, 4.999999999999998224 ) ) ;
#60453 = CARTESIAN_POINT ( 'NONE',  ( 10.34062500061451750, 6.054752690667223547, 3.707466751127219781E-16 ) ) ;
#60454 = VERTEX_POINT ( 'NONE', #67763 ) ;
#60455 = CARTESIAN_POINT ( 'NONE',  ( 16.50000000000000000, 0.000000000000000000, 4.999999999999998224 ) ) ;
#60456 = CARTESIAN_POINT ( 'NONE',  ( 22.30312500061451431, -4.541064518000417216, -2.621784821875001281 ) ) ;
#60457 = CARTESIAN_POINT ( 'NONE',  ( 10.28437500061451715, 6.421520780324663323E-16, -5.243569643749999010 ) ) ;
#60458 = ADVANCED_FACE ( 'NONE', ( #10520 ), #4623, .F. ) ;
#60459 = CARTESIAN_POINT ( 'NONE',  ( 9.262500001229033941, 4.330127018922192761, -2.499999999999997780 ) ) ;
#60460 = CARTESIAN_POINT ( 'NONE',  ( 17.73750000122903359, 6.123233995736764310E-16, -4.999999999999998224 ) ) ;
#60461 = CARTESIAN_POINT ( 'NONE',  ( 15.21562500061451750, 3.027376345333613106, -5.243569643749998122 ) ) ;
#60462 = CARTESIAN_POINT ( 'NONE',  ( 17.20312500061451644, 0.000000000000000000, 5.243569643749999010 ) ) ;
#60463 = CARTESIAN_POINT ( 'NONE',  ( 24.75000000122902932, -2.886751345948129988, 4.999999999999997335 ) ) ;
#60464 = CARTESIAN_POINT ( 'NONE',  ( 29.36250000122903003, -4.330127018922190985, -2.500000000000001332 ) ) ;
#60465 = CARTESIAN_POINT ( 'NONE',  ( 24.37500000000000000, 6.123233995736764310E-16, -4.999999999999998224 ) ) ;
#60466 = CARTESIAN_POINT ( 'NONE',  ( 3.756430356249998770, 13.50312499938548250, 32.16877607737302469 ) ) ;
#60467 = CARTESIAN_POINT ( 'NONE',  ( 26.10937500061451644, 4.541064518000418104, -2.621784821874998173 ) ) ;
#60468 = CARTESIAN_POINT ( 'NONE',  ( 1.071796769724491893, 12.48259618943233384, -26.00000000000000355 ) ) ;
#60469 = CARTESIAN_POINT ( 'NONE',  ( 12.67500000122903536, -5.773502691896255534, -1.060575238724906372E-15 ) ) ;
#60470 = EDGE_CURVE ( 'NONE', #17166, #16088, #66212, .T. ) ;
#60471 = CARTESIAN_POINT ( 'NONE',  ( 3.225000000000002309, 6.123233995736764310E-16, -4.999999999999998224 ) ) ;
#60472 = DIRECTION ( 'NONE',  ( -0.000000000000000000, -1.000000000000000000, -0.000000000000000000 ) ) ;
#60473 = CARTESIAN_POINT ( 'NONE',  ( 6.759375000614516793, 4.541064518000418104, -2.621784821874998173 ) ) ;
#60474 = VECTOR ( 'NONE', #5169, 1000.000000000000000 ) ;
#60475 = CARTESIAN_POINT ( 'NONE',  ( 26.50312500061451360, 4.541064518000418104, -2.621784821874998173 ) ) ;
#60476 = CARTESIAN_POINT ( 'NONE',  ( 4.000000000000000000, 17.00000000000000000, 30.00000000000000000 ) ) ;
#60477 = CARTESIAN_POINT ( 'NONE',  ( -1.393485112971538653, 9.904374691868481406, -24.16067974760139236 ) ) ;
#60478 = CARTESIAN_POINT ( 'NONE',  ( 27.39375000122904069, -2.886751345948157965, 4.999999999999948486 ) ) ;
#60479 = CARTESIAN_POINT ( 'NONE',  ( 5.859375000614519102, 4.541064518000418104, -2.621784821874998173 ) ) ;
#60480 = CARTESIAN_POINT ( 'NONE',  ( 8.259375000614518569, 0.000000000000000000, 5.243569643749999010 ) ) ;
#60481 = CARTESIAN_POINT ( 'NONE',  ( 29.82187500061451502, 3.027376345333611329, 5.243569643749999010 ) ) ;
#60482 =( BOUNDED_CURVE ( )  B_SPLINE_CURVE ( 2, ( #6195, #56085, #67182, #50544, #33899, #17268, #12100 ),
 .UNSPECIFIED., .F., .F. ) 
 B_SPLINE_CURVE_WITH_KNOTS ( ( 3, 2, 2, 3 ),
 ( 0.7600000000000000089, 0.7633333333333333082, 0.7666666666666668295, 0.7700000000000001288 ),
 .UNSPECIFIED. ) 
 CURVE ( )  GEOMETRIC_REPRESENTATION_ITEM ( )  RATIONAL_B_SPLINE_CURVE ( ( 1.000000000000000000, 0.8660254037844387076, 1.000000000000000000, 0.8660254037844387076, 1.000000000000000000, 0.8660254037844342667, 1.000000000000004441 ) ) 
 REPRESENTATION_ITEM ( '' )  );
#60483 = EDGE_CURVE ( 'NONE', #41970, #8994, #2215, .T. ) ;
#60484 = CARTESIAN_POINT ( 'NONE',  ( -2.121784821874996840, 12.22812500061459673, 33.67503911421598417 ) ) ;
#60485 = CARTESIAN_POINT ( 'NONE',  ( 21.52499999999999858, -4.330127018922194537, 2.499999999999995559 ) ) ;
#60486 = CARTESIAN_POINT ( 'NONE',  ( 29.02499999999999858, 4.330127018922191873, 2.499999999999999556 ) ) ;
#60487 = CARTESIAN_POINT ( 'NONE',  ( 3.825000000000001954, 4.330127018922191873, 2.499999999999999556 ) ) ;
#60488 = ORIENTED_EDGE ( 'NONE', *, *, #26844, .T. ) ;
#60489 = CARTESIAN_POINT ( 'NONE',  ( 18.62812500061451715, -4.541064518000419881, 2.621784821874995952 ) ) ;
#60490 = CARTESIAN_POINT ( 'NONE',  ( 10.97812500061451679, -4.541064518000419881, 2.621784821874995952 ) ) ;
#60491 = CARTESIAN_POINT ( 'NONE',  ( 22.43437500061451217, 5.492252693125287522, 3.363034840372157021E-16 ) ) ;
#60492 = CARTESIAN_POINT ( 'NONE',  ( 7.584375000614516082, 6.421520780324663323E-16, -5.243569643749999010 ) ) ;
#60493 = CARTESIAN_POINT ( 'NONE',  ( 24.29999999999999716, -4.330127018922190985, -2.500000000000001332 ) ) ;
#60494 = CARTESIAN_POINT ( 'NONE',  ( 20.62500000122903288, 2.886751345948126879, 4.999999999999999112 ) ) ;
#60495 = LINE ( 'NONE', #14703, #37860 ) ;
#60496 = CARTESIAN_POINT ( 'NONE',  ( 6.084375000614518747, -4.541064518000419881, 2.621784821874995952 ) ) ;
#60497 = CARTESIAN_POINT ( 'NONE',  ( 13.02187500061451608, 3.027376345333613106, -5.243569643749998122 ) ) ;
#60498 = CARTESIAN_POINT ( 'NONE',  ( 23.37187500061451573, 3.027376345333613106, -5.243569643749998122 ) ) ;
#60499 = CARTESIAN_POINT ( 'NONE',  ( 1.071796769724497445, 15.92990381179669868, -33.99999999999998579 ) ) ;
#60500 = EDGE_LOOP ( 'NONE', ( #27259, #37435, #45706, #9725 ) ) ;
#60501 = CARTESIAN_POINT ( 'NONE',  ( 12.48750000000000249, -2.886751345948129988, 4.999999999999997335 ) ) ;
#60502 = CARTESIAN_POINT ( 'NONE',  ( 18.57187500061451857, 3.027376345333611329, 5.243569643749999010 ) ) ;
#60503 = CARTESIAN_POINT ( 'NONE',  ( 10.09687500061451715, -3.027376345333614438, 5.243569643749998122 ) ) ;
#60504 = CARTESIAN_POINT ( 'NONE',  ( -3.756430356249999214, 15.52812499938548108, 27.83122392262697531 ) ) ;
#60505 = CARTESIAN_POINT ( 'NONE',  ( 21.78750000000000142, 5.773502691896255534, 3.535250795749688894E-16 ) ) ;
#60506 = CARTESIAN_POINT ( 'NONE',  ( 4.000000000000000000, 14.30000000000000071, 30.00000000000000000 ) ) ;
#60507 = CARTESIAN_POINT ( 'NONE',  ( -2.121784821874996840, 10.48437500061451821, -26.32496088578401583 ) ) ;
#60508 = CARTESIAN_POINT ( 'NONE',  ( 23.25937500061451857, -4.119189519843965641, -2.378215178125001383 ) ) ;
#60509 = CARTESIAN_POINT ( 'NONE',  ( 13.11562500061451786, 3.027376345333611329, 5.243569643749999010 ) ) ;
#60510 = CARTESIAN_POINT ( 'NONE',  ( 3.112500000000000711, -5.773502691896255534, -1.060575238724906372E-15 ) ) ;
#60511 = CARTESIAN_POINT ( 'NONE',  ( -3.999999999999999112, 19.17500000122903359, -32.30940107675850470 ) ) ;
#60512 = DIRECTION ( 'NONE',  ( -1.000000000000000000, -0.000000000000000000, -0.000000000000000000 ) ) ;
#60513 = CARTESIAN_POINT ( 'NONE',  ( 12.97499999999999964, -4.330127018922194537, 2.499999999999995559 ) ) ;
#60514 = CARTESIAN_POINT ( 'NONE',  ( -3.999999999999999112, 16.96250000122903145, 30.00000000000000000 ) ) ;
#60516 =( BOUNDED_CURVE ( )  B_SPLINE_CURVE ( 2, ( #42744, #25753, #65264, #14652, #37195, #59718, #9125, #3593, #12656 ),
 .UNSPECIFIED., .F., .F. ) 
 B_SPLINE_CURVE_WITH_KNOTS ( ( 3, 2, 2, 2, 3 ),
 ( 0.7282608695652174058, 0.7318840579710145233, 0.7391304347826086474, 0.7463768115942028825, 0.7500000000000000000 ),
 .UNSPECIFIED. ) 
 CURVE ( )  GEOMETRIC_REPRESENTATION_ITEM ( )  RATIONAL_B_SPLINE_CURVE ( ( 0.9330127018922194093, 0.9330127018922194093, 1.000000000000000000, 0.8660254037844387076, 1.000000000000000000, 0.8660254037844387076, 1.000000000000000000, 0.9330127018922194093, 0.9330127018922194093 ) ) 
 REPRESENTATION_ITEM ( '' )  );
#60515 = CARTESIAN_POINT ( 'NONE',  ( 11.92500000122903181, 2.886751345948129099, -4.999999999999998224 ) ) ;
#60517 = CARTESIAN_POINT ( 'NONE',  ( 22.65937500061451715, 0.000000000000000000, 5.243569643749999010 ) ) ;
#60518 = CARTESIAN_POINT ( 'NONE',  ( 17.48437500061451999, 6.421520780324663323E-16, -5.243569643749999010 ) ) ;
#60519 = CARTESIAN_POINT ( 'NONE',  ( 45.00000000000000000, 6.123233995736764310E-16, -4.999999999999998224 ) ) ;
#60520 = ORIENTED_EDGE ( 'NONE', *, *, #66521, .F. ) ;
#60521 = CARTESIAN_POINT ( 'NONE',  ( 17.57812500061451644, 4.541064518000418104, 2.621784821874999949 ) ) ;
#60522 = CARTESIAN_POINT ( 'NONE',  ( 29.10000000122903074, 5.773502691896255534, 3.535250795749688894E-16 ) ) ;
#60523 = CARTESIAN_POINT ( 'NONE',  ( 18.12187500061451573, 3.027376345333611329, 5.243569643749999010 ) ) ;
#60524 = CARTESIAN_POINT ( 'NONE',  ( 3.203040009831849222, 9.474684130322206244, -24.92277861900284819 ) ) ;
#60525 = CARTESIAN_POINT ( 'NONE',  ( 20.50312500061451715, -4.541064518000417216, -2.621784821875001281 ) ) ;
#60526 = CARTESIAN_POINT ( 'NONE',  ( 7.950000000000001954, 0.000000000000000000, 4.999999999999998224 ) ) ;
#60527 = CARTESIAN_POINT ( 'NONE',  ( 29.44687500061451857, -3.027376345333614438, 5.243569643749998122 ) ) ;
#60528 = CARTESIAN_POINT ( 'NONE',  ( 2.121784821874999061, 12.00312500061451715, 26.32496088578401583 ) ) ;
#60529 = CARTESIAN_POINT ( 'NONE',  ( 16.58437500061451786, 6.421520780324663323E-16, -5.243569643749999010 ) ) ;
#60530 = CARTESIAN_POINT ( 'NONE',  ( 17.17500000122903359, -5.773502691896255534, -1.060575238724906372E-15 ) ) ;
#60531 = CARTESIAN_POINT ( 'NONE',  ( 9.871875000614517504, 2.746126346562645981, -4.756430356249997438 ) ) ;
#60532 = CARTESIAN_POINT ( 'NONE',  ( 2.121784821874999061, 19.70937500061451786, -33.67503911421598417 ) ) ;
#60533 = CARTESIAN_POINT ( 'NONE',  ( 20.14687500061451786, -3.027376345333610441, -5.243569643749999898 ) ) ;
#60534 = CARTESIAN_POINT ( 'NONE',  ( 21.52500000122903145, 2.886751345948126879, 4.999999999999999112 ) ) ;
#60535 = CARTESIAN_POINT ( 'NONE',  ( 22.79062500061451502, -3.027376345333610441, -5.243569643749999898 ) ) ;
#60536 = CARTESIAN_POINT ( 'NONE',  ( 16.32187500061451502, 3.027376345333611329, 5.243569643749999010 ) ) ;
#60537 = CARTESIAN_POINT ( 'NONE',  ( 11.91562500061451857, -6.054752690667223547, -1.112240025338166033E-15 ) ) ;
#60538 = CARTESIAN_POINT ( 'NONE',  ( 2.121784821875001281, 13.70937500061451786, 33.67503911421598417 ) ) ;
#60539 =( BOUNDED_CURVE ( )  B_SPLINE_CURVE ( 2, ( #59835, #3344, #43594, #2965, #59463, #31408, #72028, #66482, #53947 ),
 .UNSPECIFIED., .F., .F. ) 
 B_SPLINE_CURVE_WITH_KNOTS ( ( 3, 2, 2, 2, 3 ),
 ( 0.9021739130434782705, 0.9057971014492753881, 0.9130434782608695121, 0.9202898550724637472, 0.9239130434782608647 ),
 .UNSPECIFIED. ) 
 CURVE ( )  GEOMETRIC_REPRESENTATION_ITEM ( )  RATIONAL_B_SPLINE_CURVE ( ( 0.9330127018922194093, 0.9330127018922194093, 1.000000000000000000, 0.8660254037844387076, 1.000000000000000000, 0.8660254037844387076, 1.000000000000000000, 0.9330127018922194093, 0.9330127018922194093 ) ) 
 REPRESENTATION_ITEM ( '' )  );
#60540 = CARTESIAN_POINT ( 'NONE',  ( 16.67812500061451786, 4.541064518000418104, 2.621784821874999949 ) ) ;
#60541 = EDGE_LOOP ( 'NONE', ( #35147, #8182, #56174, #51742 ) ) ;
#60542 = ORIENTED_EDGE ( 'NONE', *, *, #13034, .F. ) ;
#60543 = CARTESIAN_POINT ( 'NONE',  ( 22.87500000000000000, -4.330127018922194537, 2.499999999999995559 ) ) ;
#60544 = CARTESIAN_POINT ( 'NONE',  ( -4.243569643749997233, 18.99687500061451928, -27.54997392385601174 ) ) ;
#60545 = DIRECTION ( 'NONE',  ( 0.000000000000000000, 0.000000000000000000, 1.000000000000000000 ) ) ;
#60546 = CARTESIAN_POINT ( 'NONE',  ( 24.59062500061451573, -3.027376345333610441, -5.243569643749999898 ) ) ;
#60547 = CARTESIAN_POINT ( 'NONE',  ( 5.953125000614519102, 0.000000000000000000, 5.243569643749999010 ) ) ;
#60548 = CARTESIAN_POINT ( 'NONE',  ( 18.30000000122903359, 5.773502691896255534, 3.535250795749688894E-16 ) ) ;
#60549 = CARTESIAN_POINT ( 'NONE',  ( 21.25312500061451715, 0.000000000000000000, 5.243569643749999010 ) ) ;
#60550 = CARTESIAN_POINT ( 'NONE',  ( 22.72499999999999787, 4.330127018922191873, 2.499999999999999556 ) ) ;
#60551 = CARTESIAN_POINT ( 'NONE',  ( 24.85312500061451502, 0.000000000000000000, 5.243569643749999010 ) ) ;
#60552 = CARTESIAN_POINT ( 'NONE',  ( 8.353125000614518569, -4.541064518000417216, -2.621784821875001281 ) ) ;
#60553 = EDGE_LOOP ( 'NONE', ( #4193, #65136, #52909, #45032 ) ) ;
#60554 = CARTESIAN_POINT ( 'NONE',  ( 22.52812500061451573, 4.541064518000418104, 2.621784821874999949 ) ) ;
#60555 = CARTESIAN_POINT ( 'NONE',  ( 3.853125000614517681, -4.541064518000417216, -2.621784821875001281 ) ) ;
#60556 = CARTESIAN_POINT ( 'NONE',  ( 11.89687500061451608, -2.746126346562646425, 4.756430356249996549 ) ) ;
#60557 = CARTESIAN_POINT ( 'NONE',  ( -3.999999999999997335, 11.15000000122903501, 32.30940107675850470 ) ) ;
#60558 = CARTESIAN_POINT ( 'NONE',  ( 1.999999999999998668, 13.21250000122903501, -33.46410161513775705 ) ) ;
#60559 = EDGE_CURVE ( 'NONE', #35360, #57346, #52935, .T. ) ;
#60560 = FACE_OUTER_BOUND ( 'NONE', #48600, .T. ) ;
#60561 = CARTESIAN_POINT ( 'NONE',  ( 9.600000000000001421, 4.330127018922192761, -2.499999999999997780 ) ) ;
#60562 = CARTESIAN_POINT ( 'NONE',  ( 12.04687500061451821, -3.027376345333610441, -5.243569643749999898 ) ) ;
#60563 = CARTESIAN_POINT ( 'NONE',  ( 7.612500001229035362, 0.000000000000000000, 4.999999999999998224 ) ) ;
#60564 = CARTESIAN_POINT ( 'NONE',  ( 14.07187500061451679, 3.027376345333611329, 5.243569643749999010 ) ) ;
#60565 = CARTESIAN_POINT ( 'NONE',  ( 5.259375000614518569, -4.541064518000417216, -2.621784821875001281 ) ) ;
#60566 = LINE ( 'NONE', #65757, #34956 ) ;
#60567 = CARTESIAN_POINT ( 'NONE',  ( -3.999999999999999112, 10.62500000122903643, 27.69059892324149885 ) ) ;
#60568 = CARTESIAN_POINT ( 'NONE',  ( 13.28437500061451715, -4.541064518000419881, 2.621784821874995952 ) ) ;
#60569 = CARTESIAN_POINT ( 'NONE',  ( 45.00000000000000000, -2.499999999999999556, -3.499999999999999556 ) ) ;
#60570 = CARTESIAN_POINT ( 'NONE',  ( 21.47812500061451502, 6.421520780324663323E-16, -5.243569643749999010 ) ) ;
#60571 = CARTESIAN_POINT ( 'NONE',  ( 19.53749999999999432, 5.773502691896255534, 3.535250795749688401E-16 ) ) ;
#60572 = CARTESIAN_POINT ( 'NONE',  ( 9.001249775931846008E-16, 19.46562500061459033, 34.90005215228797653 ) ) ;
#60573 = CARTESIAN_POINT ( 'NONE',  ( 24.79687500061451999, 6.054752690667223547, 3.707466751127219781E-16 ) ) ;
#60574 = CARTESIAN_POINT ( 'NONE',  ( 0.000000000000000000, 27.50000000000000000, 26.00000000000000000 ) ) ;
#60575 = EDGE_CURVE ( 'NONE', #31017, #28731, #12561, .T. ) ;
#60576 = CARTESIAN_POINT ( 'NONE',  ( 29.32500000122903216, -5.773502691896255534, -1.060575238724906372E-15 ) ) ;
#60577 = CARTESIAN_POINT ( 'NONE',  ( 20.07187500061451502, 5.824947211148865298E-16, -4.756430356249998326 ) ) ;
#60578 = CARTESIAN_POINT ( 'NONE',  ( 25.90312500061451573, -4.541064518000417216, -2.621784821875001281 ) ) ;
#60579 = CARTESIAN_POINT ( 'NONE',  ( 17.54062500061451502, 6.054752690667223547, 3.707466751127219781E-16 ) ) ;
#60580 = CARTESIAN_POINT ( 'NONE',  ( 13.18125000122903323, 6.123233995736764310E-16, -4.999999999999998224 ) ) ;
#60581 = CARTESIAN_POINT ( 'NONE',  ( 14.59687500061452070, -3.027376345333614438, 5.243569643749998122 ) ) ;
#60582 = CARTESIAN_POINT ( 'NONE',  ( 7.387500001229032165, 6.123233995736764310E-16, -4.999999999999998224 ) ) ;
#60583 = CARTESIAN_POINT ( 'NONE',  ( 27.00000000122903288, -2.886751345948129988, 4.999999999999997335 ) ) ;
#60584 = CARTESIAN_POINT ( 'NONE',  ( 5.409375000614516260, 4.541064518000418104, -2.621784821874998173 ) ) ;
#60585 = CARTESIAN_POINT ( 'NONE',  ( 15.87187500061451573, 3.027376345333611329, 5.243569643749999010 ) ) ;
#60586 = CARTESIAN_POINT ( 'NONE',  ( 15.07499999999999929, 4.330127018922191873, 2.499999999999999556 ) ) ;
#60587 = CARTESIAN_POINT ( 'NONE',  ( 3.525000001229034119, 2.886751345948126879, 4.999999999999999112 ) ) ;
#60588 = CARTESIAN_POINT ( 'NONE',  ( 24.64687500061451431, -3.027376345333610441, -5.243569643749999898 ) ) ;
#60589 = CARTESIAN_POINT ( 'NONE',  ( 17.03437500061451715, 6.421520780324663323E-16, -5.243569643749999010 ) ) ;
#60590 = CARTESIAN_POINT ( 'NONE',  ( 2.655984681222220721E-16, 13.76562499938548179, 25.66244784525396483 ) ) ;
#60591 = CARTESIAN_POINT ( 'NONE',  ( 28.72500000000000142, -4.330127018922194537, 2.499999999999995559 ) ) ;
#60592 = CARTESIAN_POINT ( 'NONE',  ( 4.800000000000002487, 0.000000000000000000, 4.999999999999998224 ) ) ;
#60593 = CARTESIAN_POINT ( 'NONE',  ( 29.14687500061451075, -2.746126346562642428, -4.756430356249999214 ) ) ;
#60594 = CARTESIAN_POINT ( 'NONE',  ( 20.80312500061451431, 0.000000000000000000, 5.243569643749999010 ) ) ;
#60595 = CARTESIAN_POINT ( 'NONE',  ( 8.849999999999999645, 0.000000000000000000, 4.999999999999998224 ) ) ;
#60596 = CARTESIAN_POINT ( 'NONE',  ( 2.990625000614519191, -3.027376345333610441, -5.243569643749999898 ) ) ;
#60597 = CARTESIAN_POINT ( 'NONE',  ( 18.63749999999999929, 5.773502691896255534, 3.535250795749688894E-16 ) ) ;
#60598 = CARTESIAN_POINT ( 'NONE',  ( 15.56250000122903465, 4.330127018922192761, -2.499999999999997780 ) ) ;
#60599 = CARTESIAN_POINT ( 'NONE',  ( 22.27500000122903145, 2.886751345948129099, -4.999999999999998224 ) ) ;
#60600 = CARTESIAN_POINT ( 'NONE',  ( 4.519730000842645978, 8.925305311771492001, 33.96464799308335358 ) ) ;
#60601 = CARTESIAN_POINT ( 'NONE',  ( 3.675000000000001155, 6.123233995736764310E-16, -4.999999999999998224 ) ) ;
#60602 = ORIENTED_EDGE ( 'NONE', *, *, #38674, .F. ) ;
#60603 = CARTESIAN_POINT ( 'NONE',  ( 16.34062500061451573, -3.027376345333614438, 5.243569643749998122 ) ) ;
#60604 = CARTESIAN_POINT ( 'NONE',  ( 23.61562500061451431, -6.054752690667223547, -1.112240025338166033E-15 ) ) ;
#60605 = CARTESIAN_POINT ( 'NONE',  ( 24.00937500061451502, 0.000000000000000000, 5.243569643749999010 ) ) ;
#60606 = CARTESIAN_POINT ( 'NONE',  ( 7.162500000000001421, -5.773502691896255534, -1.060575238724906372E-15 ) ) ;
#60607 = CARTESIAN_POINT ( 'NONE',  ( 12.74062500061451786, -3.027376345333614438, 5.243569643749998122 ) ) ;
#60608 = CARTESIAN_POINT ( 'NONE',  ( 26.16562500061451502, 3.027376345333611329, 5.243569643749999010 ) ) ;
#60609 = CARTESIAN_POINT ( 'NONE',  ( 15.04687500061451644, -3.027376345333614438, 5.243569643749998122 ) ) ;
#60610 = CARTESIAN_POINT ( 'NONE',  ( 20.33437500061451786, 4.541064518000418104, 2.621784821874999949 ) ) ;
#60611 = DIRECTION ( 'NONE',  ( -0.000000000000000000, -1.000000000000000000, -0.000000000000000000 ) ) ;
#60612 = CARTESIAN_POINT ( 'NONE',  ( 2.121784821874999061, 19.65312500061451573, 26.32496088578401583 ) ) ;
#60613 = CARTESIAN_POINT ( 'NONE',  ( 22.95000000122903216, -2.886751345948129988, 4.999999999999997335 ) ) ;
#60614 = CARTESIAN_POINT ( 'NONE',  ( 17.03437500061451715, 5.824947211148865298E-16, -4.756430356249998326 ) ) ;
#60615 = CARTESIAN_POINT ( 'NONE',  ( 14.72812500061451679, 6.421520780324663323E-16, -5.243569643749999010 ) ) ;
#60616 = CARTESIAN_POINT ( 'NONE',  ( 7.471875000614519813, -6.054752690667223547, -1.112240025338166033E-15 ) ) ;
#60617 = CARTESIAN_POINT ( 'NONE',  ( 7.584375000614516082, 6.421520780324663323E-16, -5.243569643749999010 ) ) ;
#60618 = ORIENTED_EDGE ( 'NONE', *, *, #18452, .T. ) ;
#60619 = CARTESIAN_POINT ( 'NONE',  ( 27.53437500061451360, 4.541064518000418104, 2.621784821874999949 ) ) ;
#60620 = CARTESIAN_POINT ( 'NONE',  ( 19.19062500061452070, -3.027376345333610441, -5.243569643749999898 ) ) ;
#60621 = CARTESIAN_POINT ( 'NONE',  ( 28.80000000122903003, -2.886751345948129988, 4.999999999999997335 ) ) ;
#60622 = CARTESIAN_POINT ( 'NONE',  ( 2.896875000614518747, -3.027376345333614438, 5.243569643749998122 ) ) ;
#60623 = CARTESIAN_POINT ( 'NONE',  ( 24.12187500061451217, -6.054752690667223547, -1.112240025338166033E-15 ) ) ;
#60624 = CARTESIAN_POINT ( 'NONE',  ( 19.07812500061451644, -4.541064518000419881, 2.621784821874995952 ) ) ;
#60625 = CARTESIAN_POINT ( 'NONE',  ( -2.000000000000000000, 12.72499999999999964, 26.53589838486224650 ) ) ;
#60626 = CARTESIAN_POINT ( 'NONE',  ( 24.89062500061451644, -3.027376345333614438, 5.243569643749998122 ) ) ;
#60627 = CARTESIAN_POINT ( 'NONE',  ( 6.300000001229033586, -2.886751345948129988, 4.999999999999997335 ) ) ;
#60628 = ORIENTED_EDGE ( 'NONE', *, *, #27801, .T. ) ;
#60629 = CARTESIAN_POINT ( 'NONE',  ( 2.000000000000001332, 15.65000000000000036, -26.53589838486224650 ) ) ;
#60630 = CARTESIAN_POINT ( 'NONE',  ( 22.05000000122903714, -2.886751345948129988, 4.999999999999997335 ) ) ;
#60631 = CARTESIAN_POINT ( 'NONE',  ( 1.878215178124997609, 14.02812499938548285, 33.25316411605952993 ) ) ;
#60632 = CARTESIAN_POINT ( 'NONE',  ( 4.396875000614516971, -3.027376345333610441, -5.243569643749999898 ) ) ;
#60633 = CARTESIAN_POINT ( 'NONE',  ( 29.54062500061451502, -3.027376345333610441, -5.243569643749999898 ) ) ;
#60634 = CARTESIAN_POINT ( 'NONE',  ( 12.29062500061451857, -3.027376345333614438, 5.243569643749998122 ) ) ;
#60635 = CARTESIAN_POINT ( 'NONE',  ( 7.246875000614518392, 6.054752690667223547, 3.707466751127219781E-16 ) ) ;
#60636 = CARTESIAN_POINT ( 'NONE',  ( 25.01250000122903216, 4.330127018922192761, -2.499999999999997780 ) ) ;
#60637 = CARTESIAN_POINT ( 'NONE',  ( 14.93437500061451750, 4.541064518000418104, 2.621784821874999949 ) ) ;
#60638 = CARTESIAN_POINT ( 'NONE',  ( 3.384375000614517237, -4.541064518000419881, 2.621784821874995952 ) ) ;
#60639 = CARTESIAN_POINT ( 'NONE',  ( 29.84999999999999787, 4.330127018922192761, -2.499999999999997780 ) ) ;
#60640 = CARTESIAN_POINT ( 'NONE',  ( 5.578125000614518214, -4.541064518000419881, 2.621784821874995952 ) ) ;
#60641 = CARTESIAN_POINT ( 'NONE',  ( 14.72812500061451679, 6.421520780324663323E-16, -5.243569643749999010 ) ) ;
#60642 = VERTEX_POINT ( 'NONE', #897 ) ;
#60643 = CARTESIAN_POINT ( 'NONE',  ( 9.703125000614514661, -4.541064518000417216, -2.621784821875001281 ) ) ;
#60644 = CARTESIAN_POINT ( 'NONE',  ( 9.553125000614517859, 0.000000000000000000, 5.243569643749999010 ) ) ;
#60645 = CARTESIAN_POINT ( 'NONE',  ( 17.59687500061451715, 5.492252693125287522, 3.363034840372157021E-16 ) ) ;
#60646 = CARTESIAN_POINT ( 'NONE',  ( 8.662499999999999645, 2.886751345948129099, -4.999999999999998224 ) ) ;
#60647 = CARTESIAN_POINT ( 'NONE',  ( 3.862500001229035362, 4.330127018922192761, -2.499999999999997780 ) ) ;
#60648 = CARTESIAN_POINT ( 'NONE',  ( 17.84999999999999787, 0.000000000000000000, 4.999999999999998224 ) ) ;
#60649 = B_SPLINE_CURVE_WITH_KNOTS ( 'NONE', 3,
 ( #7437, #1915, #29963, #58754, #65404, #36240, #41778, #24780, #25142, #47324, #8899, #13326, #69857, #19224, #31057, #52504, #25517, #36600, #35865, #58388, #59487, #2989, #48062, #13697, #8164, #64676, #46968, #30693, #7801, #53224, #70219, #3369, #30338, #14061 ),
 .UNSPECIFIED., .F., .F.,
 ( 4, 2, 2, 2, 2, 2, 2, 2, 2, 2, 2, 2, 2, 2, 2, 2, 4 ),
 ( 0.01256276550582235453, 0.01334772285915210993, 0.01413268021248186360, 0.01491763756581161900, 0.01570259491914137440, 0.01648755227247112806, 0.01727250962580088173, 0.01805746697913063886, 0.01884242433246039253, 0.01962738168579014619, 0.02041233903911990333, 0.02119729639244965352, 0.02198225374577941066, 0.02276721109910916432, 0.02355216845243891799, 0.02433712580576867512, 0.02512208315909842879 ),
 .UNSPECIFIED. ) ;
#60650 = CARTESIAN_POINT ( 'NONE',  ( 19.20937500061451786, -4.541064518000417216, -2.621784821875001281 ) ) ;
#60651 = CARTESIAN_POINT ( 'NONE',  ( 12.86250000122903359, 4.330127018922192761, -2.499999999999997780 ) ) ;
#60652 = CARTESIAN_POINT ( 'NONE',  ( 21.67500000000000071, 6.123233995736764310E-16, -4.999999999999998224 ) ) ;
#60653 = CARTESIAN_POINT ( 'NONE',  ( 4.243569643749999898, 16.84062500061451573, -27.54997392385601529 ) ) ;
#60654 = CYLINDRICAL_SURFACE ( 'NONE', #72546, 3.999999999999996447 ) ;
#60655 = CARTESIAN_POINT ( 'NONE',  ( 19.03125000122902932, 6.123233995736764310E-16, -4.999999999999998224 ) ) ;
#60656 = DIRECTION ( 'NONE',  ( 0.000000000000000000, 0.000000000000000000, -1.000000000000000000 ) ) ;
#60657 = CARTESIAN_POINT ( 'NONE',  ( 19.98750000122903359, 6.123233995736764310E-16, -4.999999999999998224 ) ) ;
#60658 = DIRECTION ( 'NONE',  ( -0.000000000000000000, -1.000000000000000000, -0.000000000000000000 ) ) ;
#60659 = CARTESIAN_POINT ( 'NONE',  ( 14.55937500061451573, 0.000000000000000000, 5.243569643749999010 ) ) ;
#60660 =( BOUNDED_CURVE ( )  B_SPLINE_CURVE ( 2, ( #36489, #59008, #68667, #18031, #40587, #63107, #3249 ),
 .UNSPECIFIED., .F., .F. ) 
 B_SPLINE_CURVE_WITH_KNOTS ( ( 3, 2, 2, 3 ),
 ( 0.04166666666666671293, 0.04444444444444448777, 0.04722222222222225568, 0.05000000000000003053 ),
 .UNSPECIFIED. ) 
 CURVE ( )  GEOMETRIC_REPRESENTATION_ITEM ( )  RATIONAL_B_SPLINE_CURVE ( ( 0.9999999999999976685, 0.8660254037844410391, 1.000000000000000000, 0.8660254037844387076, 1.000000000000000000, 0.8660254037844373753, 1.000000000000001332 ) ) 
 REPRESENTATION_ITEM ( '' )  );
#60661 = CARTESIAN_POINT ( 'NONE',  ( 26.47499999999999787, -4.330127018922194537, 2.499999999999995559 ) ) ;
#60662 = ADVANCED_FACE ( 'NONE', ( #52214 ), #51497, .F. ) ;
#60663 = CARTESIAN_POINT ( 'NONE',  ( 9.703125000614514661, -4.541064518000417216, -2.621784821875001281 ) ) ;
#60664 = CARTESIAN_POINT ( 'NONE',  ( 26.48437500061450933, 5.492252693125287522, 3.363034840372157021E-16 ) ) ;
#60665 = CARTESIAN_POINT ( 'NONE',  ( 22.65937500061451715, 0.000000000000000000, 5.243569643749999010 ) ) ;
#60666 = CARTESIAN_POINT ( 'NONE',  ( 13.02187500061451786, 4.119189519843966529, 2.378215178124999607 ) ) ;
#60667 = CARTESIAN_POINT ( 'NONE',  ( 8.615625000614517859, 3.027376345333611329, 5.243569643749999010 ) ) ;
#60668 = CARTESIAN_POINT ( 'NONE',  ( 13.32187500061451502, -6.054752690667223547, -1.112240025338166033E-15 ) ) ;
#60669 = VERTEX_POINT ( 'NONE', #23760 ) ;
#60670 = CARTESIAN_POINT ( 'NONE',  ( 22.77187500061451786, -6.054752690667223547, -1.112240025338166033E-15 ) ) ;
#60671 = CARTESIAN_POINT ( 'NONE',  ( 30.00000000000000000, 6.123233995736764310E-16, -4.999999999999998224 ) ) ;
#60672 = FACE_OUTER_BOUND ( 'NONE', #17276, .T. ) ;
#60673 = CARTESIAN_POINT ( 'NONE',  ( 4.537500000000000533, -2.886751345948125991, -5.000000000000000000 ) ) ;
#60674 = CARTESIAN_POINT ( 'NONE',  ( 16.91250000122903430, 4.330127018922192761, -2.499999999999997780 ) ) ;
#60675 = CARTESIAN_POINT ( 'NONE',  ( 20.78732959644809952, 4.500000000000000888, -3.500000000000000000 ) ) ;
#60676 = CARTESIAN_POINT ( 'NONE',  ( 30.00000000000000000, 6.123233995736764310E-16, -4.999999999999998224 ) ) ;
#60677 = ORIENTED_EDGE ( 'NONE', *, *, #52008, .F. ) ;
#60678 = CARTESIAN_POINT ( 'NONE',  ( 13.31250000000000178, 2.886751345948126879, 4.999999999999999112 ) ) ;
#60679 = CARTESIAN_POINT ( 'NONE',  ( 17.17500000000000071, 6.123233995736764310E-16, -4.999999999999998224 ) ) ;
#60680 = CARTESIAN_POINT ( 'NONE',  ( 12.86250000122903359, 4.330127018922192761, -2.499999999999997780 ) ) ;
#60681 = CARTESIAN_POINT ( 'NONE',  ( 11.35312500061451679, 0.000000000000000000, 5.243569643749999010 ) ) ;
#60682 = ORIENTED_EDGE ( 'NONE', *, *, #51310, .T. ) ;
#60683 = CARTESIAN_POINT ( 'NONE',  ( -1.071796769724483234, 16.87009619066137134, -34.00000000000000711 ) ) ;
#60684 = CARTESIAN_POINT ( 'NONE',  ( 2.121784821875001281, 17.30937500061451573, -26.32496088578401938 ) ) ;
#60685 = CARTESIAN_POINT ( 'NONE',  ( 3.778125000614519280, -4.541064518000419881, 2.621784821874995952 ) ) ;
#60686 = CARTESIAN_POINT ( 'NONE',  ( 1.878215178125000495, 14.96562499938548463, 26.74683588394047007 ) ) ;
#60687 = CARTESIAN_POINT ( 'NONE',  ( 10.12500000000000178, 4.330127018922191873, 2.499999999999999556 ) ) ;
#60688 = FACE_OUTER_BOUND ( 'NONE', #10628, .T. ) ;
#60689 = AXIS2_PLACEMENT_3D ( 'NONE', #8602, #25214, #1618 ) ;
#60690 = EDGE_LOOP ( 'NONE', ( #30710, #40518, #55514, #49711 ) ) ;
#60691 = CARTESIAN_POINT ( 'NONE',  ( 23.20312500061451644, -4.541064518000417216, -2.621784821875001281 ) ) ;
#60692 = CARTESIAN_POINT ( 'NONE',  ( 29.43750000000000000, 5.773502691896255534, 3.535250795749688401E-16 ) ) ;
#60693 = CARTESIAN_POINT ( 'NONE',  ( -3.756430356250001434, 18.75312499938548427, 32.16877607737301048 ) ) ;
#60694 = CARTESIAN_POINT ( 'NONE',  ( 20.25937500061451857, 4.541064518000418104, -2.621784821874998173 ) ) ;
#60695 = CARTESIAN_POINT ( 'NONE',  ( 20.31562500061451715, 3.027376345333611329, 5.243569643749999010 ) ) ;
#60696 = CARTESIAN_POINT ( 'NONE',  ( -4.243569643749999898, 14.36562500061459424, -32.45002607614398471 ) ) ;
#60697 = CARTESIAN_POINT ( 'NONE',  ( 7.453125000614516438, -4.541064518000417216, -2.621784821875001281 ) ) ;
#60698 = CARTESIAN_POINT ( 'NONE',  ( 4.865625000614517859, 3.027376345333613106, -5.243569643749998122 ) ) ;
#60699 = CARTESIAN_POINT ( 'NONE',  ( 25.09687500061451715, -2.746126346562641984, -4.756430356249999214 ) ) ;
#60700 = CARTESIAN_POINT ( 'NONE',  ( 21.29062500061451502, -3.027376345333614438, 5.243569643749998122 ) ) ;
#60701 = CARTESIAN_POINT ( 'NONE',  ( 9.121875000614517504, 2.746126346562643317, 4.756430356249998326 ) ) ;
#60702 = CARTESIAN_POINT ( 'NONE',  ( 3.756430356250000546, 18.97812499938548214, 27.83122392262697886 ) ) ;
#60703 = CARTESIAN_POINT ( 'NONE',  ( 14.82187500061451679, 3.027376345333613106, -5.243569643749998122 ) ) ;
#60704 = CARTESIAN_POINT ( 'NONE',  ( 13.50937500061451679, 4.541064518000418104, -2.621784821874998173 ) ) ;
#60705 = CARTESIAN_POINT ( 'NONE',  ( 23.44687500061451502, 6.054752690667223547, 3.707466751127219781E-16 ) ) ;
#60706 = ORIENTED_EDGE ( 'NONE', *, *, #62922, .F. ) ;
#60707 = CARTESIAN_POINT ( 'NONE',  ( -4.243569643749999898, 11.30937500061451928, 30.00000000000000000 ) ) ;
#60708 = CARTESIAN_POINT ( 'NONE',  ( 2.840625000614518392, -3.027376345333614438, 5.243569643749998122 ) ) ;
#60709 = CARTESIAN_POINT ( 'NONE',  ( 26.31562500061451715, -6.054752690667223547, -1.112240025338166033E-15 ) ) ;
#60710 = VECTOR ( 'NONE', #19068, 1000.000000000000000 ) ;
#60711 = CARTESIAN_POINT ( 'NONE',  ( 26.12812500061451360, 4.541064518000418104, 2.621784821874999949 ) ) ;
#60712 = CARTESIAN_POINT ( 'NONE',  ( 1.071796769724485232, 15.29240381056766651, 25.99999999999999645 ) ) ;
#60713 = CARTESIAN_POINT ( 'NONE',  ( -3.999999999999999556, 19.51250000000000284, 27.69059892324149530 ) ) ;
#60714 = CARTESIAN_POINT ( 'NONE',  ( 4.509375000614518569, 4.541064518000418104, -2.621784821874998173 ) ) ;
#60715 = PRODUCT_CONTEXT ( 'NONE', #50292, 'mechanical' ) ;
#60716 = CARTESIAN_POINT ( 'NONE',  ( 13.83750000122903323, 4.330127018922191873, 2.499999999999999556 ) ) ;
#60717 = VECTOR ( 'NONE', #64379, 1000.000000000000000 ) ;
#60718 = CARTESIAN_POINT ( 'NONE',  ( 10.20000000122903572, 5.773502691896255534, 3.535250795749688894E-16 ) ) ;
#60719 = CARTESIAN_POINT ( 'NONE',  ( 3.328125000614516438, -4.541064518000419881, 2.621784821874995952 ) ) ;
#60720 = CARTESIAN_POINT ( 'NONE',  ( -2.000000000000001776, 15.89374999877096784, 33.46410161513775705 ) ) ;
#60721 = CARTESIAN_POINT ( 'NONE',  ( 18.39375000122903003, -2.886751345948129988, 4.999999999999997335 ) ) ;
#60722 = CARTESIAN_POINT ( 'NONE',  ( 11.07187500061451679, -6.054752690667223547, -1.112240025338166033E-15 ) ) ;
#60723 = ORIENTED_EDGE ( 'NONE', *, *, #2879, .T. ) ;
#60724 = CARTESIAN_POINT ( 'NONE',  ( 20.42812500061451431, -4.541064518000419881, 2.621784821874995952 ) ) ;
#60725 = CARTESIAN_POINT ( 'NONE',  ( 16.35937500061451644, 0.000000000000000000, 5.243569643749999010 ) ) ;
#60726 = CARTESIAN_POINT ( 'NONE',  ( 4.265625000614517326, -6.054752690667223547, -1.112240025338166033E-15 ) ) ;
#60727 = CARTESIAN_POINT ( 'NONE',  ( 21.38437500061451502, -4.541064518000419881, 2.621784821874995952 ) ) ;
#60728 = CARTESIAN_POINT ( 'NONE',  ( 4.978125000614518569, 4.541064518000418104, 2.621784821874999949 ) ) ;
#60729 = CARTESIAN_POINT ( 'NONE',  ( 20.96250000000000213, 2.886751345948154857, 4.999999999999951150 ) ) ;
#60730 = CARTESIAN_POINT ( 'NONE',  ( 6.900000001229035007, -2.886751345948125991, -5.000000000000000000 ) ) ;
#60731 =( BOUNDED_CURVE ( )  B_SPLINE_CURVE ( 2, ( #4309, #65983, #31642, #70792, #26834, #14269, #66349 ),
 .UNSPECIFIED., .F., .F. ) 
 B_SPLINE_CURVE_WITH_KNOTS ( ( 3, 2, 2, 3 ),
 ( 0.1099999999999999312, 0.1133333333333333137, 0.1166666666666666963, 0.1200000000000000788 ),
 .UNSPECIFIED. ) 
 CURVE ( )  GEOMETRIC_REPRESENTATION_ITEM ( )  RATIONAL_B_SPLINE_CURVE ( ( 1.000000000000002887, 0.8660254037844359321, 1.000000000000000000, 0.8660254037844387076, 1.000000000000000000, 0.8660254037844353769, 1.000000000000003331 ) ) 
 REPRESENTATION_ITEM ( '' )  );
#60732 = EDGE_CURVE ( 'NONE', #24253, #26902, #22489, .T. ) ;
#60733 = CARTESIAN_POINT ( 'NONE',  ( 22.71562500061451573, -6.054752690667223547, -1.112240025338166033E-15 ) ) ;
#60734 = CARTESIAN_POINT ( 'NONE',  ( 8.484601909799253346E-16, 17.07500000122903572, -25.38119784648299770 ) ) ;
#60735 = CARTESIAN_POINT ( 'NONE',  ( 8.812500001229034652, 4.330127018922192761, -2.499999999999997780 ) ) ;
#60736 = CARTESIAN_POINT ( 'NONE',  ( 20.69062500061451715, 6.054752690667223547, 3.707466751127219781E-16 ) ) ;
#60737 = CARTESIAN_POINT ( 'NONE',  ( 16.64062500061451289, 6.054752690667223547, 3.707466751127219781E-16 ) ) ;
#60738 = CARTESIAN_POINT ( 'NONE',  ( 27.08437500061451786, 4.119189519843966529, 2.378215178124999607 ) ) ;
#60739 = CARTESIAN_POINT ( 'NONE',  ( 15.18750000000000000, -2.886751345948129988, 4.999999999999997335 ) ) ;
#60740 = CARTESIAN_POINT ( 'NONE',  ( 10.76250000122903572, 0.000000000000000000, 4.999999999999998224 ) ) ;
#60741 = CARTESIAN_POINT ( 'NONE',  ( 7.115625000614516082, 3.027376345333613106, -5.243569643749998122 ) ) ;
#60742 = CARTESIAN_POINT ( 'NONE',  ( 11.87812500061451537, -4.541064518000419881, 2.621784821874995952 ) ) ;
#60743 = CARTESIAN_POINT ( 'NONE',  ( 20.55000000122903359, 5.773502691896255534, 3.535250795749688894E-16 ) ) ;
#60744 = CARTESIAN_POINT ( 'NONE',  ( -4.243569643749999898, 14.00937500061451857, -30.00000000000000000 ) ) ;
#60745 = CARTESIAN_POINT ( 'NONE',  ( 19.62187500061451573, -6.054752690667223547, -1.112240025338166033E-15 ) ) ;
#60746 = CARTESIAN_POINT ( 'NONE',  ( -1.999999999999999112, 14.39374999877096606, 26.53589838486224650 ) ) ;
#60747 = ADVANCED_FACE ( 'NONE', ( #46313 ), #63649, .T. ) ;
#60748 = CARTESIAN_POINT ( 'NONE',  ( 5.587500001229033231, 6.123233995736764310E-16, -4.999999999999998224 ) ) ;
#60749 = AXIS2_PLACEMENT_3D ( 'NONE', #44057, #49235, #43328 ) ;
#60750 = CARTESIAN_POINT ( 'NONE',  ( 3.646875000614520079, 6.054752690667223547, 3.707466751127219781E-16 ) ) ;
#60751 = CARTESIAN_POINT ( 'NONE',  ( 21.34687500061451715, -3.027376345333614438, 5.243569643749998122 ) ) ;
#60752 = CARTESIAN_POINT ( 'NONE',  ( -5.810221930991193690E-16, 14.93750000000000000, 26.00000000000000355 ) ) ;
#60753 = AXIS2_PLACEMENT_3D ( 'NONE', #32442, #49438, #38344 ) ;
#60754 = CARTESIAN_POINT ( 'NONE',  ( 18.25312500061451715, -4.541064518000417216, -2.621784821875001281 ) ) ;
#60755 = CARTESIAN_POINT ( 'NONE',  ( 12.16875000122903394, -5.773502691896255534, -1.060575238724906372E-15 ) ) ;
#60756 = CARTESIAN_POINT ( 'NONE',  ( 23.25000000000000000, 0.000000000000000000, 4.999999999999998224 ) ) ;
#60757 = CARTESIAN_POINT ( 'NONE',  ( -3.999999999999999112, 15.46250000000000036, 27.69059892324149885 ) ) ;
#60758 = CARTESIAN_POINT ( 'NONE',  ( 28.28437500061451715, 6.421520780324663323E-16, -5.243569643749999010 ) ) ;
#60759 = CARTESIAN_POINT ( 'NONE',  ( 21.53437500061451715, 5.492252693125287522, 3.363034840372157021E-16 ) ) ;
#60760 = CARTESIAN_POINT ( 'NONE',  ( 15.51562500061451644, -6.054752690667223547, -1.112240025338166033E-15 ) ) ;
#60761 = AXIS2_PLACEMENT_3D ( 'NONE', #50869, #68588, #6891 ) ;
#60762 = CARTESIAN_POINT ( 'NONE',  ( 13.32187500061451502, -6.054752690667223547, -1.112240025338166033E-15 ) ) ;
#60763 = ORIENTED_EDGE ( 'NONE', *, *, #3608, .T. ) ;
#60764 = CARTESIAN_POINT ( 'NONE',  ( 10.63125000122903252, 4.330127018922191873, 2.499999999999999556 ) ) ;
#60765 = CARTESIAN_POINT ( 'NONE',  ( 22.79062500061451502, -3.027376345333610441, -5.243569643749999898 ) ) ;
#60766 = CARTESIAN_POINT ( 'NONE',  ( -3.999999999999997335, 10.70000000122903394, -27.69059892324149530 ) ) ;
#60767 = CARTESIAN_POINT ( 'NONE',  ( 12.86250000000000071, 2.886751345948126879, 4.999999999999999112 ) ) ;
#60768 = CARTESIAN_POINT ( 'NONE',  ( 23.06250000122903288, -4.330127018922190985, -2.500000000000001332 ) ) ;
#60769 = CARTESIAN_POINT ( 'NONE',  ( 19.41562500061451146, 3.027376345333611329, 5.243569643749999010 ) ) ;
#60770 = ORIENTED_EDGE ( 'NONE', *, *, #9282, .F. ) ;
#60771 = CARTESIAN_POINT ( 'NONE',  ( 21.44999999999999929, 0.000000000000000000, 4.999999999999998224 ) ) ;
#60772 = CARTESIAN_POINT ( 'NONE',  ( 24.00937500061451502, 0.000000000000000000, 5.243569643749999010 ) ) ;
#60773 = ORIENTED_EDGE ( 'NONE', *, *, #12396, .T. ) ;
#60774 = CARTESIAN_POINT ( 'NONE',  ( 2.090614718769495450, 4.666716435056564194, -2.090614718769495450 ) ) ;
#60775 = CARTESIAN_POINT ( 'NONE',  ( 10.71562500061451928, 3.027376345333613106, -5.243569643749998122 ) ) ;
#60776 = CARTESIAN_POINT ( 'NONE',  ( 12.33750000000000213, 5.773502691896255534, 3.535250795749688401E-16 ) ) ;
#60777 = CARTESIAN_POINT ( 'NONE',  ( 13.95937500061451608, 2.746126346562643317, 4.756430356249998326 ) ) ;
#60778 = CARTESIAN_POINT ( 'NONE',  ( 16.08749999999999503, -2.886751345948129988, 4.999999999999997335 ) ) ;
#60779 = CARTESIAN_POINT ( 'NONE',  ( 24.52499999999999858, 4.330127018922191873, 2.499999999999999556 ) ) ;
#60780 = CARTESIAN_POINT ( 'NONE',  ( 7.950000000000001954, 0.000000000000000000, 4.999999999999998224 ) ) ;
#60781 = CARTESIAN_POINT ( 'NONE',  ( 3.909375000614518481, -4.541064518000417216, -2.621784821875001281 ) ) ;
#60782 = CARTESIAN_POINT ( 'NONE',  ( 17.55937500061451573, 4.541064518000418104, -2.621784821874998173 ) ) ;
#60783 = CARTESIAN_POINT ( 'NONE',  ( 27.68437500061451573, -4.541064518000419881, 2.621784821874995952 ) ) ;
#60784 = ORIENTED_EDGE ( 'NONE', *, *, #44946, .F. ) ;
#60785 = CARTESIAN_POINT ( 'NONE',  ( 26.80312500061451431, -4.541064518000417216, -2.621784821875001281 ) ) ;
#60786 = CARTESIAN_POINT ( 'NONE',  ( 27.83437500061451786, 6.421520780324663323E-16, -5.243569643749999010 ) ) ;
#60787 = LINE ( 'NONE', #4302, #67577 ) ;
#60788 = CARTESIAN_POINT ( 'NONE',  ( 14.55000000000000071, 4.330127018922192761, -2.499999999999997780 ) ) ;
#60789 = CARTESIAN_POINT ( 'NONE',  ( 12.32812500061451821, -4.541064518000419881, 2.621784821874995952 ) ) ;
#60790 = CARTESIAN_POINT ( 'NONE',  ( 6.150000000000003020, 0.000000000000000000, 4.999999999999998224 ) ) ;
#60791 = CARTESIAN_POINT ( 'NONE',  ( 1.071796769724505438, 11.31740381056766864, 26.00000000000001421 ) ) ;
#60792 = CARTESIAN_POINT ( 'NONE',  ( 27.81562500061452070, 3.027376345333612662, -5.243569643749998122 ) ) ;
#60793 = CARTESIAN_POINT ( 'NONE',  ( 16.42500000122903359, 2.886751345948129099, -4.999999999999998224 ) ) ;
#60794 = LINE ( 'NONE', #71157, #32460 ) ;
#60795 = CARTESIAN_POINT ( 'NONE',  ( 14.07187500061451679, 2.746126346562643317, 4.756430356249998326 ) ) ;
#60796 = CARTESIAN_POINT ( 'NONE',  ( 6.178125000614518747, 6.421520780324663323E-16, -5.243569643749999010 ) ) ;
#60797 = CARTESIAN_POINT ( 'NONE',  ( 22.99687500061451573, 6.054752690667223547, 3.707466751127219781E-16 ) ) ;
#60798 = CARTESIAN_POINT ( 'NONE',  ( -4.243569643749999898, 18.02187500061452141, 27.54997392385601529 ) ) ;
#60799 = CARTESIAN_POINT ( 'NONE',  ( 22.80937500061451573, -4.541064518000417216, -2.621784821875001281 ) ) ;
#60800 = CARTESIAN_POINT ( 'NONE',  ( 3.187500000000002220, -2.886751345948125991, -5.000000000000000000 ) ) ;
#60801 = CARTESIAN_POINT ( 'NONE',  ( 10.53750000000000320, 5.773502691896255534, 3.535250795749688401E-16 ) ) ;
#60802 = CARTESIAN_POINT ( 'NONE',  ( 11.24062500061451608, 6.054752690667223547, 3.707466751127219781E-16 ) ) ;
#60803 = CARTESIAN_POINT ( 'NONE',  ( 2.962500001229034119, 4.330127018922192761, -2.499999999999997780 ) ) ;
#60804 = CARTESIAN_POINT ( 'NONE',  ( 7.884375000614517681, -4.541064518000419881, 2.621784821874995952 ) ) ;
#60805 = CARTESIAN_POINT ( 'NONE',  ( 7.537500001229033408, 4.330127018922191873, 2.499999999999999556 ) ) ;
#60806 = CARTESIAN_POINT ( 'NONE',  ( 10.94062500061451537, -3.027376345333614438, 5.243569643749998122 ) ) ;
#60807 = CARTESIAN_POINT ( 'NONE',  ( 15.15937500061451715, -4.541064518000417216, -2.621784821875001281 ) ) ;
#60808 = CARTESIAN_POINT ( 'NONE',  ( 24.43125000122903145, 6.123233995736764310E-16, -4.999999999999998224 ) ) ;
#60809 = CARTESIAN_POINT ( 'NONE',  ( 21.60000000122903430, -2.886751345948129988, 4.999999999999997335 ) ) ;
#60810 = CARTESIAN_POINT ( 'NONE',  ( 7.021875000614518747, -6.054752690667223547, -1.112240025338166033E-15 ) ) ;
#60811 = CARTESIAN_POINT ( 'NONE',  ( 10.19062500061451892, -3.027376345333610441, -5.243569643749999898 ) ) ;
#60812 = CARTESIAN_POINT ( 'NONE',  ( 26.90625000122902932, 0.000000000000000000, 4.999999999999998224 ) ) ;
#60813 = CARTESIAN_POINT ( 'NONE',  ( 21.23437500061451644, 4.541064518000418104, 2.621784821874999949 ) ) ;
#60814 = FACE_BOUND ( 'NONE', #72891, .T. ) ;
#60815 = CARTESIAN_POINT ( 'NONE',  ( 4.907911205059083602E-16, 5.000000000000000000, 33.99999999999999289 ) ) ;
#60816 = FACE_OUTER_BOUND ( 'NONE', #8496, .T. ) ;
#60817 = CARTESIAN_POINT ( 'NONE',  ( 4.243569643749999898, 11.08437500061451786, -30.00000000000000000 ) ) ;
#60818 = CARTESIAN_POINT ( 'NONE',  ( 15.90000000122903501, -2.886751345948125991, -5.000000000000000000 ) ) ;
#60819 = ADVANCED_FACE ( 'NONE', ( #17847 ), #46676, .F. ) ;
#60820 = AXIS2_PLACEMENT_3D ( 'NONE', #36832, #8390, #54924 ) ;
#60821 = CARTESIAN_POINT ( 'NONE',  ( 2.121784821875001281, 14.55312500061451786, -26.32496088578401938 ) ) ;
#60822 = CARTESIAN_POINT ( 'NONE',  ( 17.10000000122903430, -2.886751345948129988, 4.999999999999997335 ) ) ;
#60823 = CARTESIAN_POINT ( 'NONE',  ( 11.01562500061451821, -6.054752690667223547, -1.112240025338166033E-15 ) ) ;
#60824 = ORIENTED_EDGE ( 'NONE', *, *, #55867, .F. ) ;
#60825 = CARTESIAN_POINT ( 'NONE',  ( 13.64999999999999858, 4.330127018922192761, -2.499999999999997780 ) ) ;
#60826 = CARTESIAN_POINT ( 'NONE',  ( -3.999999999999999112, 13.66250000000000142, 27.69059892324149885 ) ) ;
#60827 = CARTESIAN_POINT ( 'NONE',  ( 22.15312500061451573, 0.000000000000000000, 5.243569643749999010 ) ) ;
#60828 = CARTESIAN_POINT ( 'NONE',  ( 10.05937500061451750, 0.000000000000000000, 5.243569643749999010 ) ) ;
#60829 = EDGE_CURVE ( 'NONE', #54070, #48258, #40777, .T. ) ;
#60830 = CARTESIAN_POINT ( 'NONE',  ( 4.395499815916704911, -2.383214571124957271, -4.670699935784250911 ) ) ;
#60831 = CARTESIAN_POINT ( 'NONE',  ( 10.27500000122903323, 2.886751345948126879, 4.999999999999999112 ) ) ;
#60832 = CARTESIAN_POINT ( 'NONE',  ( 19.68750000122903288, 4.330127018922191873, 2.499999999999999556 ) ) ;
#60833 = CARTESIAN_POINT ( 'NONE',  ( 14.65312500061451573, -4.541064518000417216, -2.621784821875001281 ) ) ;
#60834 = EDGE_CURVE ( 'NONE', #65514, #18562, #20101, .T. ) ;
#60835 = CARTESIAN_POINT ( 'NONE',  ( 17.05312500061451786, 4.541064518000418104, -2.621784821874998173 ) ) ;
#60836 = CARTESIAN_POINT ( 'NONE',  ( 26.21250000122903501, -4.330127018922190985, -2.500000000000001332 ) ) ;
#60837 = CARTESIAN_POINT ( 'NONE',  ( 28.87500000122902932, -5.773502691896255534, -1.060575238724906372E-15 ) ) ;
#60838 = CARTESIAN_POINT ( 'NONE',  ( 21.89999999999999858, 0.000000000000000000, 4.999999999999998224 ) ) ;
#60839 = CARTESIAN_POINT ( 'NONE',  ( 3.756430356249998770, 14.40312499938548463, 32.16877607737302469 ) ) ;
#60840 = CARTESIAN_POINT ( 'NONE',  ( 26.37187500061451217, -6.054752690667223547, -1.112240025338166033E-15 ) ) ;
#60841 = CARTESIAN_POINT ( 'NONE',  ( 11.66249999999999964, -5.773502691896255534, -1.060575238724906372E-15 ) ) ;
#60842 = CARTESIAN_POINT ( 'NONE',  ( 12.37500000122903465, 2.886751345948129099, -4.999999999999998224 ) ) ;
#60843 = CARTESIAN_POINT ( 'NONE',  ( 4.050000000000001599, -4.330127018922190985, -2.500000000000001332 ) ) ;
#60844 = DIRECTION ( 'NONE',  ( -1.000000000000000000, -0.000000000000000000, -0.000000000000000000 ) ) ;
#60845 = CARTESIAN_POINT ( 'NONE',  ( 6.121875000614517504, -6.054752690667223547, -1.112240025338166033E-15 ) ) ;
#60846 = CARTESIAN_POINT ( 'NONE',  ( 25.67812500061451431, 4.541064518000418104, 2.621784821874999949 ) ) ;
#60847 = CARTESIAN_POINT ( 'NONE',  ( 1.878215178124997609, 13.12812499938548427, 33.25316411605952993 ) ) ;
#60848 = DIRECTION ( 'NONE',  ( -1.000000000000000000, -0.000000000000000000, -0.000000000000000000 ) ) ;
#60849 = AXIS2_PLACEMENT_3D ( 'NONE', #10612, #20217, #5076 ) ;
#60850 = CARTESIAN_POINT ( 'NONE',  ( 10.32187500061451679, 3.027376345333613106, -5.243569643749998122 ) ) ;
#60851 = AXIS2_PLACEMENT_3D ( 'NONE', #45869, #62845, #1172 ) ;
#60852 = CARTESIAN_POINT ( 'NONE',  ( 4.305944032607977867, -2.541529510831473271, 4.468189746291087339 ) ) ;
#60853 = CARTESIAN_POINT ( 'NONE',  ( 28.75312500061451715, 4.541064518000418104, -2.621784821874998173 ) ) ;
#60854 = CARTESIAN_POINT ( 'NONE',  ( 9.084375000614517859, 4.541064518000418104, 2.621784821874999949 ) ) ;
#60855 = CARTESIAN_POINT ( 'NONE',  ( 29.74687500061451217, 6.054752690667223547, 3.707466751127219781E-16 ) ) ;
#60856 = EDGE_CURVE ( 'NONE', #66791, #64403, #9770, .T. ) ;
#60857 = CARTESIAN_POINT ( 'NONE',  ( 9.001249775931846008E-16, 12.71562500061459389, 34.90005215228797653 ) ) ;
#60858 = CARTESIAN_POINT ( 'NONE',  ( 21.07499999999999929, -4.330127018922194537, 2.499999999999995559 ) ) ;
#60859 = ORIENTED_EDGE ( 'NONE', *, *, #34767, .F. ) ;
#60860 = CARTESIAN_POINT ( 'NONE',  ( 29.81250000000000000, 2.886751345948129099, -4.999999999999998224 ) ) ;
#60861 = CARTESIAN_POINT ( 'NONE',  ( 5.212500000000002132, 2.886751345948126879, 4.999999999999999112 ) ) ;
#60862 = ORIENTED_EDGE ( 'NONE', *, *, #18371, .F. ) ;
#60863 = CARTESIAN_POINT ( 'NONE',  ( 17.87812500061451715, 6.421520780324663323E-16, -5.243569643749999010 ) ) ;
#60864 = CARTESIAN_POINT ( 'NONE',  ( 7.340625000614518392, -3.027376345333614438, 5.243569643749998122 ) ) ;
#60865 = CARTESIAN_POINT ( 'NONE',  ( 21.94687500061451146, 4.119189519843966529, -2.378215178124998275 ) ) ;
#60866 = CARTESIAN_POINT ( 'NONE',  ( 6.384375000614516793, 4.541064518000418104, 2.621784821874999949 ) ) ;
#60867 = CARTESIAN_POINT ( 'NONE',  ( 17.06250000122903288, 0.000000000000000000, 4.999999999999998224 ) ) ;
#60868 = CARTESIAN_POINT ( 'NONE',  ( 20.78732959644809952, -2.499999999999999556, 3.499999999999999556 ) ) ;
#60869 = CARTESIAN_POINT ( 'NONE',  ( 5.859375000614519102, 4.541064518000418104, -2.621784821874998173 ) ) ;
#60870 = CARTESIAN_POINT ( 'NONE',  ( 11.89687500061451608, -3.027376345333614438, 5.243569643749998122 ) ) ;
#60871 = CARTESIAN_POINT ( 'NONE',  ( 23.14687500061451786, -3.027376345333614438, 5.243569643749998122 ) ) ;
#60872 = CARTESIAN_POINT ( 'NONE',  ( 26.84999999999999787, 0.000000000000000000, 4.999999999999998224 ) ) ;
#60873 = VERTEX_POINT ( 'NONE', #24850 ) ;
#60874 = CARTESIAN_POINT ( 'NONE',  ( 12.07499999999999929, -4.330127018922194537, 2.499999999999995559 ) ) ;
#60875 = CARTESIAN_POINT ( 'NONE',  ( 18.27187500061451431, -6.054752690667223547, -1.112240025338166033E-15 ) ) ;
#60876 = CARTESIAN_POINT ( 'NONE',  ( 9.084375000614517859, 4.541064518000418104, 2.621784821874999949 ) ) ;
#60877 = CARTESIAN_POINT ( 'NONE',  ( -3.756430356249999214, 14.17812499938548498, 27.83122392262697531 ) ) ;
#60878 = CARTESIAN_POINT ( 'NONE',  ( 22.16250000000000142, 2.886751345948129099, -4.999999999999998224 ) ) ;
#60879 = CARTESIAN_POINT ( 'NONE',  ( -1.999999999999999112, 17.14999999999999858, 26.53589838486224650 ) ) ;
#60880 = CARTESIAN_POINT ( 'NONE',  ( -4.000000000000000000, 17.22500000000000142, 30.00000000000000000 ) ) ;
#60881 = CARTESIAN_POINT ( 'NONE',  ( 21.79687500061451644, -2.746126346562646425, 4.756430356249996549 ) ) ;
#60882 = CARTESIAN_POINT ( 'NONE',  ( 13.41562500061451502, 3.027376345333613106, -5.243569643749998122 ) ) ;
#60883 = CARTESIAN_POINT ( 'NONE',  ( 28.09687500061451360, -3.027376345333614438, 5.243569643749998122 ) ) ;
#60884 = CARTESIAN_POINT ( 'NONE',  ( 6.787500001229032520, -4.330127018922194537, 2.499999999999995559 ) ) ;
#60885 = CARTESIAN_POINT ( 'NONE',  ( 29.22187500061451715, 3.027376345333613106, -5.243569643749998122 ) ) ;
#60886 = CARTESIAN_POINT ( 'NONE',  ( 10.20000000000000107, 0.000000000000000000, 4.999999999999998224 ) ) ;
#60887 = CARTESIAN_POINT ( 'NONE',  ( 1.999999999999998668, 15.46250000122903501, 26.53589838486224650 ) ) ;
#60888 = CARTESIAN_POINT ( 'NONE',  ( 8.175000001229031810, -5.773502691896255534, -1.060575238724906372E-15 ) ) ;
#60889 = CARTESIAN_POINT ( 'NONE',  ( 22.43437500061451573, 6.421520780324663323E-16, -5.243569643749999010 ) ) ;
#60890 = CARTESIAN_POINT ( 'NONE',  ( 14.63437500061451679, -4.541064518000419881, 2.621784821874995952 ) ) ;
#60891 = CARTESIAN_POINT ( 'NONE',  ( 4.013004193198248970, 2.982582328347916700, -4.312681910770049143 ) ) ;
#60892 = VERTEX_POINT ( 'NONE', #68130 ) ;
#60893 = CARTESIAN_POINT ( 'NONE',  ( 17.50312500061451715, 4.541064518000418104, -2.621784821874998173 ) ) ;
#60894 = CARTESIAN_POINT ( 'NONE',  ( 29.21250000122903145, 0.000000000000000000, 4.999999999999998224 ) ) ;
#60895 = CARTESIAN_POINT ( 'NONE',  ( 14.59687500061452070, -3.027376345333614438, 5.243569643749998122 ) ) ;
#60896 = CARTESIAN_POINT ( 'NONE',  ( 5.838630383562667170, 8.118670948950970967, -28.60360171723054634 ) ) ;
#60897 = CARTESIAN_POINT ( 'NONE',  ( 16.90312500061451573, -4.541064518000417216, -2.621784821875001281 ) ) ;
#60898 = CYLINDRICAL_SURFACE ( 'NONE', #26788, 10.00000000000000000 ) ;
#60899 = CARTESIAN_POINT ( 'NONE',  ( 29.59687500061451715, -3.027376345333610441, -5.243569643749999898 ) ) ;
#60900 = CARTESIAN_POINT ( 'NONE',  ( 2.121784821875001281, 13.20312500061451821, 33.67503911421598417 ) ) ;
#60901 = CARTESIAN_POINT ( 'NONE',  ( 18.27187500061451431, -6.054752690667223547, -1.112240025338166033E-15 ) ) ;
#60902 = CARTESIAN_POINT ( 'NONE',  ( 14.21250000122903323, 4.330127018922192761, -2.499999999999997780 ) ) ;
#60903 = CARTESIAN_POINT ( 'NONE',  ( 10.99687500061451928, -2.746126346562646425, 4.756430356249996549 ) ) ;
#60904 = CARTESIAN_POINT ( 'NONE',  ( 2.121784821875001281, 19.55937500061451573, -26.32496088578401938 ) ) ;
#60905 = CARTESIAN_POINT ( 'NONE',  ( 19.95937500061451786, 0.000000000000000000, 5.243569643749999010 ) ) ;
#60906 = CARTESIAN_POINT ( 'NONE',  ( 21.86250000122903003, 4.330127018922192761, -2.499999999999997780 ) ) ;
#60907 = CARTESIAN_POINT ( 'NONE',  ( 15.94687500061451502, -3.027376345333614438, 5.243569643749998122 ) ) ;
#60908 = CARTESIAN_POINT ( 'NONE',  ( 13.49062500061451608, 6.054752690667223547, 3.707466751127219781E-16 ) ) ;
#60909 = CARTESIAN_POINT ( 'NONE',  ( -4.243569643749999898, 12.17187500061451999, 27.54997392385601529 ) ) ;
#60910 = AXIS2_PLACEMENT_3D ( 'NONE', #37678, #60200, #9612 ) ;
#60911 = CARTESIAN_POINT ( 'NONE',  ( 17.69062500061451715, -3.027376345333614438, 5.243569643749998122 ) ) ;
#60912 = ORIENTED_EDGE ( 'NONE', *, *, #69480, .F. ) ;
#60913 = VERTEX_POINT ( 'NONE', #17496 ) ;
#60914 = CARTESIAN_POINT ( 'NONE',  ( 21.60000000000000142, -4.330127018922190985, -2.500000000000001332 ) ) ;
#60915 = DIRECTION ( 'NONE',  ( 1.000000000000000000, -0.000000000000000000, -0.000000000000000000 ) ) ;
#60916 = CARTESIAN_POINT ( 'NONE',  ( 25.07812500061451644, 6.421520780324663323E-16, -5.243569643749999010 ) ) ;
#60917 = CARTESIAN_POINT ( 'NONE',  ( 5.915625000614515905, 3.027376345333611329, 5.243569643749999010 ) ) ;
#60918 = CARTESIAN_POINT ( 'NONE',  ( 17.25000000122903288, -2.886751345948125991, -5.000000000000000000 ) ) ;
#60919 = CARTESIAN_POINT ( 'NONE',  ( 22.15312500061451573, 0.000000000000000000, 5.243569643749999010 ) ) ;
#60920 = CARTESIAN_POINT ( 'NONE',  ( 22.61250000000000071, 2.886751345948129099, -4.999999999999998224 ) ) ;
#60921 = EDGE_CURVE ( 'NONE', #43636, #57370, #57849, .T. ) ;
#60922 = CARTESIAN_POINT ( 'NONE',  ( 26.01562500061451289, 3.027376345333613106, -5.243569643749998122 ) ) ;
#60923 = CARTESIAN_POINT ( 'NONE',  ( 4.828125000614518214, 6.421520780324663323E-16, -5.243569643749999010 ) ) ;
#60924 = ORIENTED_EDGE ( 'NONE', *, *, #17853, .T. ) ;
#60925 = CARTESIAN_POINT ( 'NONE',  ( 26.96250000122903145, 0.000000000000000000, 4.999999999999998224 ) ) ;
#60926 = CARTESIAN_POINT ( 'NONE',  ( 10.62187500061451928, -5.492252693125287522, -1.008910452111647106E-15 ) ) ;
#60927 = DIRECTION ( 'NONE',  ( -1.000000000000000000, -0.000000000000000000, -0.000000000000000000 ) ) ;
#60928 = CARTESIAN_POINT ( 'NONE',  ( 3.999999999999998668, 12.72500000122903430, -32.30940107675850470 ) ) ;
#60929 = CARTESIAN_POINT ( 'NONE',  ( -4.243569643749999898, 18.47187500061451715, -32.45002607614398471 ) ) ;
#60930 =( BOUNDED_CURVE ( )  B_SPLINE_CURVE ( 2, ( #4829, #38816, #7526, #62946, #29698, #18954, #18225, #57761, #36334 ),
 .UNSPECIFIED., .F., .F. ) 
 B_SPLINE_CURVE_WITH_KNOTS ( ( 3, 2, 2, 2, 3 ),
 ( 0.9239130434782608647, 0.9275362318840579823, 0.9347826086956522174, 0.9420289855072463414, 0.9456521739130434590 ),
 .UNSPECIFIED. ) 
 CURVE ( )  GEOMETRIC_REPRESENTATION_ITEM ( )  RATIONAL_B_SPLINE_CURVE ( ( 0.9330127018922194093, 0.9330127018922194093, 1.000000000000000000, 0.8660254037844387076, 1.000000000000000000, 0.8660254037844387076, 1.000000000000000000, 0.9330127018922194093, 0.9330127018922194093 ) ) 
 REPRESENTATION_ITEM ( '' )  );
#60931 = CARTESIAN_POINT ( 'NONE',  ( 11.55000000000000071, 0.000000000000000000, 4.999999999999998224 ) ) ;
#60932 = CARTESIAN_POINT ( 'NONE',  ( 10.77187500061451786, 3.027376345333613106, -5.243569643749998122 ) ) ;
#60933 = CARTESIAN_POINT ( 'NONE',  ( 6.375000001229031987, -5.773502691896255534, -1.060575238724906372E-15 ) ) ;
#60934 = CARTESIAN_POINT ( 'NONE',  ( 11.67187500061451821, 3.027376345333613106, -5.243569643749998122 ) ) ;
#60935 = CARTESIAN_POINT ( 'NONE',  ( 5.334375000614517859, 6.421520780324663323E-16, -5.243569643749999010 ) ) ;
#60936 = FACE_OUTER_BOUND ( 'NONE', #22251, .T. ) ;
#60937 = AXIS2_PLACEMENT_3D ( 'NONE', #50575, #11773, #72740 ) ;
#60938 = CARTESIAN_POINT ( 'NONE',  ( -1.071796769724488563, 10.75490381179670152, 34.00000000000000000 ) ) ;
#60939 = CARTESIAN_POINT ( 'NONE',  ( 10.35937500061451644, 4.541064518000418104, -2.621784821874998173 ) ) ;
#60940 = CARTESIAN_POINT ( 'NONE',  ( 13.35000000000000142, 0.000000000000000000, 4.999999999999998224 ) ) ;
#60941 = CARTESIAN_POINT ( 'NONE',  ( 20.27812500061451573, 4.541064518000418104, 2.621784821874999949 ) ) ;
#60942 = CARTESIAN_POINT ( 'NONE',  ( 19.46250000000000213, 2.886751345948045611, -5.000000000000141220 ) ) ;
#60943 = CARTESIAN_POINT ( 'NONE',  ( -4.243569643749999898, 19.31562500061459176, 27.54997392385601529 ) ) ;
#60944 = CARTESIAN_POINT ( 'NONE',  ( 23.59687500061451715, -3.027376345333614438, 5.243569643749998122 ) ) ;
#60945 = CARTESIAN_POINT ( 'NONE',  ( 4.167140676845648706, 2.763139261668956514, -4.167140676845877856 ) ) ;
#60946 =( BOUNDED_CURVE ( )  B_SPLINE_CURVE ( 2, ( #34740, #51745, #1144, #12931, #26584, #59449, #37297, #31762, #48755 ),
 .UNSPECIFIED., .F., .F. ) 
 B_SPLINE_CURVE_WITH_KNOTS ( ( 3, 2, 2, 2, 3 ),
 ( 0.1413043478260869734, 0.1449275362318840632, 0.1521739130434782705, 0.1594202898550724501, 0.1630434782608695676 ),
 .UNSPECIFIED. ) 
 CURVE ( )  GEOMETRIC_REPRESENTATION_ITEM ( )  RATIONAL_B_SPLINE_CURVE ( ( 0.9330127018922194093, 0.9330127018922196314, 1.000000000000000000, 0.8660254037844387076, 1.000000000000000000, 0.8660254037844387076, 1.000000000000000000, 0.9330127018922190762, 0.9330127018922194093 ) ) 
 REPRESENTATION_ITEM ( '' )  );
#60947 = CARTESIAN_POINT ( 'NONE',  ( 28.80000000122903003, -2.886751345948129988, 4.999999999999997335 ) ) ;
#60948 = CARTESIAN_POINT ( 'NONE',  ( 19.50937500061451857, -5.492252693125287522, -1.008910452111647106E-15 ) ) ;
#60949 = CARTESIAN_POINT ( 'NONE',  ( 24.32812500061451289, 4.541064518000418104, 2.621784821874999949 ) ) ;
#60950 = CARTESIAN_POINT ( 'NONE',  ( 17.12812500061451715, 4.541064518000418104, 2.621784821874999949 ) ) ;
#60951 = CARTESIAN_POINT ( 'NONE',  ( 14.45625000122903359, -4.330127018922190985, -2.500000000000001332 ) ) ;
#60952 = CARTESIAN_POINT ( 'NONE',  ( 15.30937500061451750, 4.541064518000418104, -2.621784821874998173 ) ) ;
#60953 = CARTESIAN_POINT ( 'NONE',  ( 16.91250000000000142, 2.886751345948161074, 4.999999999999941380 ) ) ;
#60954 = VECTOR ( 'NONE', #40967, 1000.000000000000000 ) ;
#60955 = CARTESIAN_POINT ( 'NONE',  ( 26.62500000122903288, -5.773502691896255534, -1.060575238724906372E-15 ) ) ;
#60956 = CARTESIAN_POINT ( 'NONE',  ( 4.096875000614518925, 6.054752690667223547, 3.707466751127219781E-16 ) ) ;
#60957 = CARTESIAN_POINT ( 'NONE',  ( 15.19687500061451857, -3.027376345333610441, -5.243569643749999898 ) ) ;
#60958 = CARTESIAN_POINT ( 'NONE',  ( 4.869423765992945796, -1.135214599616954256, -5.119209941160161037 ) ) ;
#60959 = B_SPLINE_CURVE_WITH_KNOTS ( 'NONE', 1,
 ( #15022, #32757 ),
 .UNSPECIFIED., .F., .F.,
 ( 2, 2 ),
 ( 0.000000000000000000, 1.000000000000000000 ),
 .UNSPECIFIED. ) ;
#60960 = CARTESIAN_POINT ( 'NONE',  ( 10.70625000122903536, 0.000000000000000000, 4.999999999999998224 ) ) ;
#60961 = EDGE_CURVE ( 'NONE', #30519, #48240, #56027, .T. ) ;
#60962 = CARTESIAN_POINT ( 'NONE',  ( 3.600000001229033408, -2.886751345948129988, 4.999999999999997335 ) ) ;
#60963 = CARTESIAN_POINT ( 'NONE',  ( 24.08437500061451786, -4.541064518000419881, 2.621784821874995952 ) ) ;
#60964 = CARTESIAN_POINT ( 'NONE',  ( 17.18437500061451573, 4.541064518000418104, 2.621784821874999949 ) ) ;
#60965 = CARTESIAN_POINT ( 'NONE',  ( 3.756430356249998770, 16.31562499938548427, 32.16877607737302469 ) ) ;
#60966 = CARTESIAN_POINT ( 'NONE',  ( 28.87499999999999645, 6.123233995736764310E-16, -4.999999999999998224 ) ) ;
#60967 = CARTESIAN_POINT ( 'NONE',  ( 3.787500001229033408, 6.123233995736764310E-16, -4.999999999999998224 ) ) ;
#60968 = CARTESIAN_POINT ( 'NONE',  ( 4.987500000000002487, -2.886751345948125991, -5.000000000000000000 ) ) ;
#60969 = CARTESIAN_POINT ( 'NONE',  ( 28.88437500061451502, 4.119189519843966529, 2.378215178124999607 ) ) ;
#60970 = CARTESIAN_POINT ( 'NONE',  ( 19.37812500061451715, 4.541064518000418104, 2.621784821874999949 ) ) ;
#60971 = CARTESIAN_POINT ( 'NONE',  ( 9.787499999999999645, -2.886751345948129988, 4.999999999999997335 ) ) ;
#60972 = CARTESIAN_POINT ( 'NONE',  ( 3.328125000614516438, -4.541064518000419881, 2.621784821874995952 ) ) ;
#60973 = CARTESIAN_POINT ( 'NONE',  ( 19.20000000000000284, 0.000000000000000000, 4.999999999999998224 ) ) ;
#60974 = DIRECTION ( 'NONE',  ( -1.000000000000000000, -0.000000000000000000, -0.000000000000000000 ) ) ;
#60975 = CARTESIAN_POINT ( 'NONE',  ( 22.83750000122903501, 4.330127018922191873, 2.499999999999999556 ) ) ;
#60976 = CARTESIAN_POINT ( 'NONE',  ( 5.800002967315413649, 8.146762937617078038, 28.41205895484640820 ) ) ;
#60977 =( BOUNDED_CURVE ( )  B_SPLINE_CURVE ( 2, ( #58439, #7850, #23739, #875, #46287, #46652, #2313 ),
 .UNSPECIFIED., .F., .F. ) 
 B_SPLINE_CURVE_WITH_KNOTS ( ( 3, 2, 2, 3 ),
 ( 0.1999999999999999556, 0.2027777777777777235, 0.2055555555555554914, 0.2083333333333332871 ),
 .UNSPECIFIED. ) 
 CURVE ( )  GEOMETRIC_REPRESENTATION_ITEM ( )  RATIONAL_B_SPLINE_CURVE ( ( 1.000000000000002665, 0.8660254037844360431, 1.000000000000000000, 0.8660254037844387076, 1.000000000000000000, 0.8660254037844413721, 0.9999999999999973355 ) ) 
 REPRESENTATION_ITEM ( '' )  );
#60978 = CARTESIAN_POINT ( 'NONE',  ( 29.10937500061451644, -4.541064518000417216, -2.621784821875001281 ) ) ;
#60979 = ORIENTED_EDGE ( 'NONE', *, *, #5722, .F. ) ;
#60980 = CARTESIAN_POINT ( 'NONE',  ( 16.56562500061451715, 3.027376345333613106, -5.243569643749998122 ) ) ;
#60981 = CARTESIAN_POINT ( 'NONE',  ( 25.15312500061451217, 4.541064518000418104, -2.621784821874998173 ) ) ;
#60982 = CARTESIAN_POINT ( 'NONE',  ( 22.17187500061451644, 3.027376345333611329, 5.243569643749999010 ) ) ;
#60983 = CARTESIAN_POINT ( 'NONE',  ( 7.462500000000001243, 2.886751345948126879, 4.999999999999999112 ) ) ;
#60984 = CARTESIAN_POINT ( 'NONE',  ( 9.065625000614517148, 3.027376345333611329, 5.243569643749999010 ) ) ;
#60985 = CARTESIAN_POINT ( 'NONE',  ( 26.42812500061451431, 6.421520780324663323E-16, -5.243569643749999010 ) ) ;
#60986 = CARTESIAN_POINT ( 'NONE',  ( 14.70937500061451786, -4.541064518000417216, -2.621784821875001281 ) ) ;
#60987 = CARTESIAN_POINT ( 'NONE',  ( 20.37187500061451573, 3.027376345333611329, 5.243569643749999010 ) ) ;
#60988 = CARTESIAN_POINT ( 'NONE',  ( 3.999999999999999112, 11.78750000122903430, -30.00000000000000000 ) ) ;
#60989 = CARTESIAN_POINT ( 'NONE',  ( -3.000416591977282496E-16, 10.29687500061451644, 25.09994784771203058 ) ) ;
#60990 = CARTESIAN_POINT ( 'NONE',  ( 21.18750000122903288, -4.330127018922194537, 2.499999999999995559 ) ) ;
#60991 = CARTESIAN_POINT ( 'NONE',  ( 17.07187500061451502, 2.746126346562645981, -4.756430356249997438 ) ) ;
#60992 = CARTESIAN_POINT ( 'NONE',  ( 12.36562500061451786, -6.054752690667223547, -1.112240025338166033E-15 ) ) ;
#60993 = CARTESIAN_POINT ( 'NONE',  ( 8.896875000614517859, -3.027376345333610441, -5.243569643749999898 ) ) ;
#60994 = CARTESIAN_POINT ( 'NONE',  ( 8.409375000614518925, -4.541064518000417216, -2.621784821875001281 ) ) ;
#60995 = VERTEX_POINT ( 'NONE', #53297 ) ;
#60996 = CARTESIAN_POINT ( 'NONE',  ( 28.84687500061452070, 6.054752690667223547, 3.707466751127219781E-16 ) ) ;
#60997 = CARTESIAN_POINT ( 'NONE',  ( 18.40312500061451573, 4.541064518000418104, -2.621784821874998173 ) ) ;
#60998 = CARTESIAN_POINT ( 'NONE',  ( 2.915625000614516793, -6.054752690667223547, -1.112240025338166033E-15 ) ) ;
#60999 = CARTESIAN_POINT ( 'NONE',  ( 3.121875000614518836, 3.027376345333613106, -5.243569643749998122 ) ) ;
#61000 = CARTESIAN_POINT ( 'NONE',  ( 24.64687500061451431, -3.027376345333610441, -5.243569643749999898 ) ) ;
#61001 = CARTESIAN_POINT ( 'NONE',  ( 18.89062500061451644, 6.054752690667223547, 3.707466751127219781E-16 ) ) ;
#61002 = CARTESIAN_POINT ( 'NONE',  ( -2.828200636599751609E-16, 10.43750000000000178, 25.38119784648299770 ) ) ;
#61003 = CARTESIAN_POINT ( 'NONE',  ( 23.65312500061451573, -4.541064518000417216, -2.621784821875001281 ) ) ;
#61004 = CARTESIAN_POINT ( 'NONE',  ( 5.625000001229036428, 2.886751345948129099, -4.999999999999998224 ) ) ;
#61005 = ORIENTED_EDGE ( 'NONE', *, *, #68031, .T. ) ;
#61006 = CARTESIAN_POINT ( 'NONE',  ( 3.262500001229035718, -4.330127018922190985, -2.500000000000001332 ) ) ;
#61007 = CARTESIAN_POINT ( 'NONE',  ( -2.828200636599751609E-16, 16.28749999999999787, -34.61880215351700230 ) ) ;
#61008 = CARTESIAN_POINT ( 'NONE',  ( -1.878215178124999163, 17.85312499938548214, 26.74683588394047007 ) ) ;
#61009 = CARTESIAN_POINT ( 'NONE',  ( 4.359375000614517326, -4.541064518000417216, -2.621784821875001281 ) ) ;
#61010 = CARTESIAN_POINT ( 'NONE',  ( 25.34999999999999787, 4.330127018922192761, -2.499999999999997780 ) ) ;
#61011 = CARTESIAN_POINT ( 'NONE',  ( 11.91562500061451857, -6.054752690667223547, -1.112240025338166033E-15 ) ) ;
#61012 = CARTESIAN_POINT ( 'NONE',  ( 6.571875000614517681, -6.054752690667223547, -1.112240025338166033E-15 ) ) ;
#61013 = CARTESIAN_POINT ( 'NONE',  ( 25.12500000122903288, 2.886751345948126879, 4.999999999999999112 ) ) ;
#61014 = VECTOR ( 'NONE', #61848, 1000.000000000000000 ) ;
#61015 = CARTESIAN_POINT ( 'NONE',  ( 15.23437500061451644, 6.421520780324663323E-16, -5.243569643749999010 ) ) ;
#61016 = CARTESIAN_POINT ( 'NONE',  ( 28.52812500061451573, -4.541064518000419881, 2.621784821874995952 ) ) ;
#61017 = CARTESIAN_POINT ( 'NONE',  ( 29.25000000000000000, -4.330127018922190985, -2.500000000000001332 ) ) ;
#61018 = CARTESIAN_POINT ( 'NONE',  ( 25.84687500061451360, -3.027376345333614438, 5.243569643749998122 ) ) ;
#61019 = CARTESIAN_POINT ( 'NONE',  ( 3.178125000614515638, 4.541064518000418104, 2.621784821874999949 ) ) ;
#61020 = CARTESIAN_POINT ( 'NONE',  ( 12.06562500061451537, 3.027376345333613106, -5.243569643749998122 ) ) ;
#61021 = EDGE_CURVE ( 'NONE', #54204, #49855, #17306, .T. ) ;
#61022 = VERTEX_POINT ( 'NONE', #71396 ) ;
#61023 = CARTESIAN_POINT ( 'NONE',  ( 10.94062500061451537, -3.027376345333614438, 5.243569643749998122 ) ) ;
#61024 = CARTESIAN_POINT ( 'NONE',  ( 9.065625000614517148, 3.027376345333611329, 5.243569643749999010 ) ) ;
#61025 = CARTESIAN_POINT ( 'NONE',  ( 18.19687500061451502, -2.746126346562646425, 4.756430356249996549 ) ) ;
#61026 = CARTESIAN_POINT ( 'NONE',  ( 8.812500000000000000, 2.886751345948126879, 4.999999999999999112 ) ) ;
#61027 = CARTESIAN_POINT ( 'NONE',  ( 5.062500001229035540, -4.330127018922190985, -2.500000000000001332 ) ) ;
#61028 = CARTESIAN_POINT ( 'NONE',  ( 17.43750000000000355, -2.886751345948129988, 4.999999999999997335 ) ) ;
#61029 = CARTESIAN_POINT ( 'NONE',  ( 18.94687500061451502, 6.054752690667223547, 3.707466751127219781E-16 ) ) ;
#61030 = CARTESIAN_POINT ( 'NONE',  ( 13.38750000122903394, 4.330127018922191873, 2.499999999999999556 ) ) ;
#61031 = CARTESIAN_POINT ( 'NONE',  ( 19.94999999999999929, 4.330127018922192761, -2.499999999999997780 ) ) ;
#61032 = CARTESIAN_POINT ( 'NONE',  ( 4.243569643749999898, 15.52812500061451750, -30.00000000000000000 ) ) ;
#61033 = CARTESIAN_POINT ( 'NONE',  ( 21.97500000000000142, -4.330127018922194537, 2.499999999999995559 ) ) ;
#61034 = DIRECTION ( 'NONE',  ( 0.000000000000000000, 0.000000000000000000, -1.000000000000000000 ) ) ;
#61035 = DIRECTION ( 'NONE',  ( -0.000000000000000000, -1.000000000000000000, -0.000000000000000000 ) ) ;
#61036 = FACE_BOUND ( 'NONE', #21614, .T. ) ;
#61037 = CARTESIAN_POINT ( 'NONE',  ( 4.000000000000000000, 16.13749999999999929, -27.69059892324149885 ) ) ;
#61038 = CARTESIAN_POINT ( 'NONE',  ( 13.54687500061451999, 6.054752690667223547, 3.707466751127219781E-16 ) ) ;
#61039 = CARTESIAN_POINT ( 'NONE',  ( 27.33750000000000213, -2.886751345948129988, 4.999999999999997335 ) ) ;
#61040 = CARTESIAN_POINT ( 'NONE',  ( 9.328125000614518214, 6.421520780324663323E-16, -5.243569643749999010 ) ) ;
#61041 = CARTESIAN_POINT ( 'NONE',  ( 27.57187500061451502, -4.119189519843968306, 2.378215178124996054 ) ) ;
#61042 = CARTESIAN_POINT ( 'NONE',  ( 21.27187500061451786, 3.027376345333611329, 5.243569643749999010 ) ) ;
#61043 = CARTESIAN_POINT ( 'NONE',  ( 12.64687500061451786, 0.000000000000000000, 4.756430356249998326 ) ) ;
#61044 = CARTESIAN_POINT ( 'NONE',  ( 8.540625000614518569, 6.054752690667223547, 3.707466751127219781E-16 ) ) ;
#61045 = CARTESIAN_POINT ( 'NONE',  ( 11.44687500061451857, -3.027376345333614438, 5.243569643749998122 ) ) ;
#61046 = EDGE_LOOP ( 'NONE', ( #37878, #51526, #26158, #17258 ) ) ;
#61047 = CARTESIAN_POINT ( 'NONE',  ( 21.27187500061451786, 3.027376345333611329, 5.243569643749999010 ) ) ;
#61048 = CARTESIAN_POINT ( 'NONE',  ( 29.06249999999999645, 2.886751345948164182, 4.999999999999933387 ) ) ;
#61049 = CARTESIAN_POINT ( 'NONE',  ( 5.025000000000002132, 6.123233995736764310E-16, -4.999999999999998224 ) ) ;
#61050 = AXIS2_PLACEMENT_3D ( 'NONE', #30563, #64535, #13193 ) ;
#61051 = CARTESIAN_POINT ( 'NONE',  ( 13.91250000122903252, 0.000000000000000000, 4.999999999999998224 ) ) ;
#61052 = CARTESIAN_POINT ( 'NONE',  ( 30.00000000000000000, 6.123233995736764310E-16, -4.999999999999998224 ) ) ;
#61053 = CARTESIAN_POINT ( 'NONE',  ( 3.802324603042571027, -3.246905036188573845, 4.117364570290419579 ) ) ;
#61054 = VERTEX_POINT ( 'NONE', #14868 ) ;
#61055 = CARTESIAN_POINT ( 'NONE',  ( 13.19999999999999929, 4.330127018922192761, -2.499999999999997780 ) ) ;
#61056 = CARTESIAN_POINT ( 'NONE',  ( 15.59999999999999964, 0.000000000000000000, 4.999999999999998224 ) ) ;
#61057 = CARTESIAN_POINT ( 'NONE',  ( 13.53750000122903430, -4.330127018922194537, 2.499999999999995559 ) ) ;
#61058 = CARTESIAN_POINT ( 'NONE',  ( 11.72812500061451857, 4.541064518000418104, 2.621784821874999949 ) ) ;
#61059 = PRESENTATION_LAYER_ASSIGNMENT (  '', '', ( #41039 ) ) ;
#61060 = EDGE_LOOP ( 'NONE', ( #4740, #58111, #55660, #41765 ) ) ;
#61061 = CARTESIAN_POINT ( 'NONE',  ( 8.849999999999999645, 0.000000000000000000, 4.999999999999998224 ) ) ;
#61062 = CARTESIAN_POINT ( 'NONE',  ( 26.36250000000000071, 2.886751345948110892, 5.000000000000026645 ) ) ;
#61063 = CARTESIAN_POINT ( 'NONE',  ( -2.121784821874999949, 13.48437500061451821, -33.67503911421598417 ) ) ;
#61064 = CARTESIAN_POINT ( 'NONE',  ( 2.840625000614518392, -3.027376345333614438, 5.243569643749998122 ) ) ;
#61065 = CARTESIAN_POINT ( 'NONE',  ( -3.756430356250000102, 15.56562499938548427, 30.00000000000000000 ) ) ;
#61066 = CARTESIAN_POINT ( 'NONE',  ( 9.225000000000001421, 4.330127018922191873, 2.499999999999999556 ) ) ;
#61067 = CARTESIAN_POINT ( 'NONE',  ( 3.171572016300020724, 3.865480461419896763, 3.489665696640699810 ) ) ;
#61068 = ORIENTED_EDGE ( 'NONE', *, *, #28164, .F. ) ;
#61069 = CARTESIAN_POINT ( 'NONE',  ( 24.17812500061451786, 6.421520780324663323E-16, -5.243569643749999010 ) ) ;
#61070 = CARTESIAN_POINT ( 'NONE',  ( 30.00000000000000000, 6.123233995736764310E-16, -4.999999999999998224 ) ) ;
#61071 = CARTESIAN_POINT ( 'NONE',  ( -7.967954043666661671E-16, 20.17812499938548143, 34.33755215474603517 ) ) ;
#61072 = CARTESIAN_POINT ( 'NONE',  ( 21.98437500061451644, 6.421520780324663323E-16, -5.243569643749999010 ) ) ;
#61073 = CARTESIAN_POINT ( 'NONE',  ( 17.35312500061451502, -4.541064518000417216, -2.621784821875001281 ) ) ;
#61074 = CARTESIAN_POINT ( 'NONE',  ( -2.121784821874999949, 10.72812500061459318, -33.67503911421598417 ) ) ;
#61075 = CARTESIAN_POINT ( 'NONE',  ( 5.615625000614517859, -6.054752690667223547, -1.112240025338166033E-15 ) ) ;
#61076 = CARTESIAN_POINT ( 'NONE',  ( 3.103125000614517237, 4.541064518000418104, -2.621784821874998173 ) ) ;
#61077 = CARTESIAN_POINT ( 'NONE',  ( 24.57187500061451502, -5.492252693125287522, -1.008910452111647106E-15 ) ) ;
#61078 = CARTESIAN_POINT ( 'NONE',  ( 20.31562500061451715, 3.027376345333611329, 5.243569643749999010 ) ) ;
#61079 = CARTESIAN_POINT ( 'NONE',  ( 8.821875000614518569, -5.492252693125287522, -1.008910452111647106E-15 ) ) ;
#61080 = CARTESIAN_POINT ( 'NONE',  ( 3.756430356250000102, 18.49062499938548143, 30.00000000000000000 ) ) ;
#61081 = CARTESIAN_POINT ( 'NONE',  ( 14.85937500061451644, 4.541064518000418104, -2.621784821874998173 ) ) ;
#61082 = CARTESIAN_POINT ( 'NONE',  ( 14.22187500061451537, -6.054752690667223547, -1.112240025338166033E-15 ) ) ;
#61083 = CARTESIAN_POINT ( 'NONE',  ( 23.10937500061451644, 0.000000000000000000, 5.243569643749999010 ) ) ;
#61084 = ORIENTED_EDGE ( 'NONE', *, *, #62019, .T. ) ;
#61085 = CARTESIAN_POINT ( 'NONE',  ( 4.243569643749999898, 11.98437500061451821, 30.00000000000000000 ) ) ;
#61086 = CARTESIAN_POINT ( 'NONE',  ( -2.000000000000000000, 14.63750000122903394, -33.46410161513775705 ) ) ;
#61087 = CARTESIAN_POINT ( 'NONE',  ( 26.12812500061451360, 4.541064518000418104, 2.621784821874999949 ) ) ;
#61088 = EDGE_CURVE ( 'NONE', #25347, #68777, #71024, .T. ) ;
#61089 = CARTESIAN_POINT ( 'NONE',  ( 26.05312500061451431, 4.541064518000418104, -2.621784821874998173 ) ) ;
#61090 = CARTESIAN_POINT ( 'NONE',  ( 8.287500001229034297, 6.123233995736764310E-16, -4.999999999999998224 ) ) ;
#61091 = CARTESIAN_POINT ( 'NONE',  ( -3.999999999999999556, 19.96250000000000213, 27.69059892324149530 ) ) ;
#61092 = CARTESIAN_POINT ( 'NONE',  ( 4.921875000614518214, 3.027376345333613106, -5.243569643749998122 ) ) ;
#61093 = DIRECTION ( 'NONE',  ( 0.000000000000000000, 0.000000000000000000, 1.000000000000000000 ) ) ;
#61094 = CARTESIAN_POINT ( 'NONE',  ( 12.45000000122903394, 5.773502691896255534, 3.535250795749688894E-16 ) ) ;
#61095 = CARTESIAN_POINT ( 'NONE',  ( 8.475000001229034297, 2.886751345948126879, 4.999999999999999112 ) ) ;
#61096 = CARTESIAN_POINT ( 'NONE',  ( 29.36250000122903003, -4.330127018922190985, -2.500000000000001332 ) ) ;
#61097 = CARTESIAN_POINT ( 'NONE',  ( 4.000000000000000000, 15.14374999877096606, 30.00000000000000000 ) ) ;
#61098 = CARTESIAN_POINT ( 'NONE',  ( 19.44375000122903430, -2.886751345948125991, -5.000000000000000000 ) ) ;
#61099 = CARTESIAN_POINT ( 'NONE',  ( 11.97187500061451892, -6.054752690667223547, -1.112240025338166033E-15 ) ) ;
#61100 = CARTESIAN_POINT ( 'NONE',  ( -1.071796769724490339, 17.52634618820329848, 26.00000000000000000 ) ) ;
#61101 = ORIENTED_EDGE ( 'NONE', *, *, #26912, .T. ) ;
#61102 = CARTESIAN_POINT ( 'NONE',  ( 19.41562500061451146, 3.027376345333611329, 5.243569643749999010 ) ) ;
#61103 = CARTESIAN_POINT ( 'NONE',  ( 12.83437500061451786, -4.541064518000419881, 2.621784821874995952 ) ) ;
#61104 = CARTESIAN_POINT ( 'NONE',  ( 5.428125000614517859, 4.541064518000418104, 2.621784821874999949 ) ) ;
#61105 = EDGE_CURVE ( 'NONE', #14078, #34155, #5162, .T. ) ;
#61106 = CARTESIAN_POINT ( 'NONE',  ( 23.10937500061451644, 0.000000000000000000, 5.243569643749999010 ) ) ;
#61107 = CARTESIAN_POINT ( 'NONE',  ( 6.178125000614518747, 6.421520780324663323E-16, -5.243569643749999010 ) ) ;
#61108 = DIRECTION ( 'NONE',  ( -1.000000000000000000, -0.000000000000000000, -0.000000000000000000 ) ) ;
#61109 = CARTESIAN_POINT ( 'NONE',  ( 5.400000001229032343, -2.886751345948129988, 4.999999999999997335 ) ) ;
#61110 = CARTESIAN_POINT ( 'NONE',  ( 21.36562500061451431, -6.054752690667223547, -1.112240025338166033E-15 ) ) ;
#61111 = EDGE_CURVE ( 'NONE', #30507, #12269, #14501, .T. ) ;
#61112 = CARTESIAN_POINT ( 'NONE',  ( -2.828200636599751609E-16, 17.75000000122903288, -34.61880215351700230 ) ) ;
#61113 = CARTESIAN_POINT ( 'NONE',  ( 7.950000001229033053, 5.773502691896255534, 3.535250795749688894E-16 ) ) ;
#61114 = CARTESIAN_POINT ( 'NONE',  ( 16.94062500061451715, -3.027376345333610441, -5.243569643749999898 ) ) ;
#61115 = CARTESIAN_POINT ( 'NONE',  ( 15.17812500061451608, 6.421520780324663323E-16, -5.243569643749999010 ) ) ;
#61116 = CARTESIAN_POINT ( 'NONE',  ( 26.10937500061451644, 4.119189519843966529, -2.378215178124998275 ) ) ;
#61117 = CARTESIAN_POINT ( 'NONE',  ( 16.31250000000000000, 2.886751345948129099, -4.999999999999998224 ) ) ;
#61118 = CARTESIAN_POINT ( 'NONE',  ( 12.22500000122903430, -5.773502691896255534, -1.060575238724906372E-15 ) ) ;
#61119 = CARTESIAN_POINT ( 'NONE',  ( 6.965625000614518392, -6.054752690667223547, -1.112240025338166033E-15 ) ) ;
#61120 = CARTESIAN_POINT ( 'NONE',  ( 11.20312500061451644, 4.541064518000418104, -2.621784821874998173 ) ) ;
#61121 = EDGE_CURVE ( 'NONE', #10824, #31619, #34771, .T. ) ;
#61122 =( BOUNDED_CURVE ( )  B_SPLINE_CURVE ( 2, ( #8788, #31322, #43143, #25413, #48323, #54227, #20221 ),
 .UNSPECIFIED., .F., .F. ) 
 B_SPLINE_CURVE_WITH_KNOTS ( ( 3, 2, 2, 3 ),
 ( 0.5749999999999999556, 0.5777777777777777235, 0.5805555555555557135, 0.5833333333333334814 ),
 .UNSPECIFIED. ) 
 CURVE ( )  GEOMETRIC_REPRESENTATION_ITEM ( )  RATIONAL_B_SPLINE_CURVE ( ( 1.000000000000000000, 0.8660254037844387076, 1.000000000000000000, 0.8660254037844387076, 1.000000000000000000, 0.8660254037844333785, 1.000000000000005329 ) ) 
 REPRESENTATION_ITEM ( '' )  );
#61123 = CARTESIAN_POINT ( 'NONE',  ( 22.01250000122903216, 0.000000000000000000, 4.999999999999998224 ) ) ;
#61124 = CARTESIAN_POINT ( 'NONE',  ( -4.243569643749997233, 13.14687500061451786, -27.54997392385601174 ) ) ;
#61125 = CARTESIAN_POINT ( 'NONE',  ( 4.929940333177246004, 0.8485134343999930495, 4.980930601228622301 ) ) ;
#61126 = CARTESIAN_POINT ( 'NONE',  ( 5.700000001229033941, 5.773502691896255534, 3.535250795749688894E-16 ) ) ;
#61127 = CARTESIAN_POINT ( 'NONE',  ( 4.509375000614518569, 4.541064518000418104, -2.621784821874998173 ) ) ;
#61128 = CARTESIAN_POINT ( 'NONE',  ( 21.90937500061451715, -4.541064518000417216, -2.621784821875001281 ) ) ;
#61129 = CARTESIAN_POINT ( 'NONE',  ( 27.52500000000000213, 6.123233995736764310E-16, -4.999999999999998224 ) ) ;
#61130 = CARTESIAN_POINT ( 'NONE',  ( 16.56562500061451715, 3.027376345333613106, -5.243569643749998122 ) ) ;
#61131 = CARTESIAN_POINT ( 'NONE',  ( 11.30625000122903501, -4.330127018922190985, -2.500000000000001332 ) ) ;
#61132 = CARTESIAN_POINT ( 'NONE',  ( 29.55937500061451573, -4.541064518000417216, -2.621784821875001281 ) ) ;
#61133 = CARTESIAN_POINT ( 'NONE',  ( 20.82187500061451502, -4.119189519843968306, 2.378215178124996054 ) ) ;
#61134 = CARTESIAN_POINT ( 'NONE',  ( 15.96562500061451573, -6.054752690667223547, -1.112240025338166033E-15 ) ) ;
#61135 = CARTESIAN_POINT ( 'NONE',  ( 12.04687500061451821, -3.027376345333610441, -5.243569643749999898 ) ) ;
#61136 = ORIENTED_EDGE ( 'NONE', *, *, #19011, .F. ) ;
#61137 = CARTESIAN_POINT ( 'NONE',  ( 22.23750000000000071, 5.773502691896255534, 3.535250795749688401E-16 ) ) ;
#61138 = CARTESIAN_POINT ( 'NONE',  ( 22.41562500061451502, 3.027376345333613106, -5.243569643749998122 ) ) ;
#61139 = CARTESIAN_POINT ( 'NONE',  ( 3.999999999999999112, 11.22500000000000142, -30.00000000000000000 ) ) ;
#61140 = CARTESIAN_POINT ( 'NONE',  ( -1.999999999999997113, 18.38750000122903572, 33.46410161513775705 ) ) ;
#61141 = VECTOR ( 'NONE', #19583, 1000.000000000000000 ) ;
#61142 = CARTESIAN_POINT ( 'NONE',  ( 12.71250000000000036, 2.886751345948129099, -4.999999999999998224 ) ) ;
#61143 = CARTESIAN_POINT ( 'NONE',  ( 24.60000000122903430, 5.773502691896255534, 3.535250795749688894E-16 ) ) ;
#61144 = CARTESIAN_POINT ( 'NONE',  ( 18.85312500061451502, 4.541064518000418104, -2.621784821874998173 ) ) ;
#61145 = CARTESIAN_POINT ( 'NONE',  ( 13.02187500061451786, 4.119189519843966529, 2.378215178124999607 ) ) ;
#61146 = VERTEX_POINT ( 'NONE', #37407 ) ;
#61147 = CARTESIAN_POINT ( 'NONE',  ( 19.38749999999999929, -2.886751345948125991, -5.000000000000000000 ) ) ;
#61148 = CARTESIAN_POINT ( 'NONE',  ( 21.94687500061451857, -3.027376345333610441, -5.243569643749999898 ) ) ;
#61149 = CARTESIAN_POINT ( 'NONE',  ( 27.62812500061451360, -4.541064518000419881, 2.621784821874995952 ) ) ;
#61150 = ORIENTED_EDGE ( 'NONE', *, *, #33221, .F. ) ;
#61151 = CARTESIAN_POINT ( 'NONE',  ( 2.000000000000001332, 17.89999999999999858, -26.53589838486224650 ) ) ;
#61152 = CARTESIAN_POINT ( 'NONE',  ( 11.46562500061451573, -6.054752690667223547, -1.112240025338166033E-15 ) ) ;
#61153 = CARTESIAN_POINT ( 'NONE',  ( -1.626862140677534273E-15, 15.53749999999999964, 34.00000000000000000 ) ) ;
#61154 = CARTESIAN_POINT ( 'NONE',  ( 14.25937500061451679, 2.746126346562645981, -4.756430356249997438 ) ) ;
#61155 = CARTESIAN_POINT ( 'NONE',  ( 17.62500000000000000, 6.123233995736764310E-16, -4.999999999999998224 ) ) ;
#61156 = CARTESIAN_POINT ( 'NONE',  ( 24.11249999999999716, 2.886751345948126879, 4.999999999999999112 ) ) ;
#61157 = CARTESIAN_POINT ( 'NONE',  ( 3.619842856578028734, -3.449164782042274169, -3.619842856578066481 ) ) ;
#61158 = CARTESIAN_POINT ( 'NONE',  ( 3.759375000614517681, 0.000000000000000000, 5.243569643749999010 ) ) ;
#61159 = CARTESIAN_POINT ( 'NONE',  ( 29.07187500061451502, -6.054752690667223547, -1.112240025338166033E-15 ) ) ;
#61160 = ORIENTED_EDGE ( 'NONE', *, *, #10710, .F. ) ;
#61161 = CARTESIAN_POINT ( 'NONE',  ( 26.91562500061451146, 3.027376345333613106, -5.243569643749998122 ) ) ;
#61162 = CARTESIAN_POINT ( 'NONE',  ( 24.90937500061451715, 0.000000000000000000, 5.243569643749999010 ) ) ;
#61163 = CARTESIAN_POINT ( 'NONE',  ( -4.243569643749999898, 18.90312500061459389, -30.00000000000000000 ) ) ;
#61164 = CARTESIAN_POINT ( 'NONE',  ( 13.04999999999999893, -4.330127018922190985, -2.500000000000001332 ) ) ;
#61165 = CARTESIAN_POINT ( 'NONE',  ( 10.52812500061451750, -4.541064518000419881, 2.621784821874995952 ) ) ;
#61166 = CARTESIAN_POINT ( 'NONE',  ( 4.000000000000000000, 17.39374999877096428, 30.00000000000000000 ) ) ;
#61167 = CARTESIAN_POINT ( 'NONE',  ( 4.428044609675158227, 2.322158679919935409, 4.428044609675073850 ) ) ;
#61168 = CARTESIAN_POINT ( 'NONE',  ( 28.41562500061451502, 3.027376345333611329, 5.243569643749999010 ) ) ;
#61169 = CARTESIAN_POINT ( 'NONE',  ( 16.91250000122903430, 4.330127018922192761, -2.499999999999997780 ) ) ;
#61170 = CARTESIAN_POINT ( 'NONE',  ( 22.55625000122903145, -4.330127018922190985, -2.500000000000001332 ) ) ;
#61171 = CARTESIAN_POINT ( 'NONE',  ( 15.45937500061451608, 0.000000000000000000, 4.756430356249998326 ) ) ;
#61172 = CARTESIAN_POINT ( 'NONE',  ( 4.228125000614517681, -4.541064518000419881, 2.621784821874995952 ) ) ;
#61173 = CARTESIAN_POINT ( 'NONE',  ( 22.84687500061451715, -3.027376345333610441, -5.243569643749999898 ) ) ;
#61174 = CARTESIAN_POINT ( 'NONE',  ( 4.243569643749999898, 14.19687500061451857, 32.45002607614398471 ) ) ;
#61175 = CARTESIAN_POINT ( 'NONE',  ( 21.04687500061451644, -3.027376345333610441, -5.243569643749999898 ) ) ;
#61176 = CARTESIAN_POINT ( 'NONE',  ( 29.78437500061451715, 4.541064518000418104, 2.621784821874999949 ) ) ;
#61177 = CARTESIAN_POINT ( 'NONE',  ( 4.243569643749999010, 17.87187500061451928, 27.54997392385601174 ) ) ;
#61178 = CARTESIAN_POINT ( 'NONE',  ( 10.30312500061451431, 4.541064518000418104, -2.621784821874998173 ) ) ;
#61180 =( BOUNDED_CURVE ( )  B_SPLINE_CURVE ( 2, ( #69223, #905, #17503, #18584, #40417, #7513, #52584 ),
 .UNSPECIFIED., .F., .F. ) 
 B_SPLINE_CURVE_WITH_KNOTS ( ( 3, 2, 2, 3 ),
 ( 0.9300000000000001599, 0.9333333333333334592, 0.9366666666666668695, 0.9400000000000001688 ),
 .UNSPECIFIED. ) 
 CURVE ( )  GEOMETRIC_REPRESENTATION_ITEM ( )  RATIONAL_B_SPLINE_CURVE ( ( 0.9999999999999955591, 0.8660254037844431485, 1.000000000000000000, 0.8660254037844387076, 1.000000000000000000, 0.8660254037844298258, 1.000000000000008882 ) ) 
 REPRESENTATION_ITEM ( '' )  );
#61179 = DIRECTION ( 'NONE',  ( -1.000000000000000000, -0.000000000000000000, -0.000000000000000000 ) ) ;
#61181 = CARTESIAN_POINT ( 'NONE',  ( 7.359375000614516438, 0.000000000000000000, 5.243569643749999010 ) ) ;
#61182 = CARTESIAN_POINT ( 'NONE',  ( 7.612500001229035362, 0.000000000000000000, 4.999999999999998224 ) ) ;
#61183 = CARTESIAN_POINT ( 'NONE',  ( 7.640625000614517326, 6.054752690667223547, 3.707466751127219781E-16 ) ) ;
#61184 = CARTESIAN_POINT ( 'NONE',  ( 10.99687500061451750, -3.027376345333614438, 5.243569643749998122 ) ) ;
#61185 = CARTESIAN_POINT ( 'NONE',  ( 0.000000000000000000, 0.000000000000000000, -50.00000000000000000 ) ) ;
#61186 = CARTESIAN_POINT ( 'NONE',  ( 19.76250000122903216, 0.000000000000000000, 4.999999999999998224 ) ) ;
#61187 = CARTESIAN_POINT ( 'NONE',  ( 9.196875000614518569, -3.027376345333614438, 5.243569643749998122 ) ) ;
#61188 = CARTESIAN_POINT ( 'NONE',  ( 10.26562500061451644, 3.027376345333613106, -5.243569643749998122 ) ) ;
#61189 = CARTESIAN_POINT ( 'NONE',  ( 6.403125000614517504, 0.000000000000000000, 5.243569643749999010 ) ) ;
#61190 = EDGE_CURVE ( 'NONE', #22800, #24417, #38028, .T. ) ;
#61191 = CARTESIAN_POINT ( 'NONE',  ( 25.85625000122903216, 4.330127018922192761, -2.499999999999997780 ) ) ;
#61192 = CARTESIAN_POINT ( 'NONE',  ( 19.47187500061451360, 3.027376345333611329, 5.243569643749999010 ) ) ;
#61193 = CARTESIAN_POINT ( 'NONE',  ( 11.50312500061451892, -4.541064518000417216, -2.621784821875001281 ) ) ;
#61194 = CARTESIAN_POINT ( 'NONE',  ( 28.95937500061451431, 0.000000000000000000, 5.243569643749999010 ) ) ;
#61195 = CARTESIAN_POINT ( 'NONE',  ( 4.243569643749999010, 12.47187500061451715, -32.45002607614398471 ) ) ;
#61196 = CARTESIAN_POINT ( 'NONE',  ( 12.52500000122903145, 2.886751345948126879, 4.999999999999999112 ) ) ;
#61197 = CARTESIAN_POINT ( 'NONE',  ( 2.121784821874999061, 15.60312500061451857, -33.67503911421598417 ) ) ;
#61198 = CARTESIAN_POINT ( 'NONE',  ( 14.17500000122903536, 2.886751345948129099, -4.999999999999998224 ) ) ;
#61199 = CARTESIAN_POINT ( 'NONE',  ( 11.24062500061451608, 6.054752690667223547, 3.707466751127219781E-16 ) ) ;
#61200 = ORIENTED_EDGE ( 'NONE', *, *, #380, .T. ) ;
#61201 = CARTESIAN_POINT ( 'NONE',  ( 13.04999999999999893, -4.330127018922190985, -2.500000000000001332 ) ) ;
#61202 = CARTESIAN_POINT ( 'NONE',  ( 10.36875000122903323, -5.773502691896255534, -1.060575238724906372E-15 ) ) ;
#61203 = CARTESIAN_POINT ( 'NONE',  ( 21.85312500061451502, -4.541064518000417216, -2.621784821875001281 ) ) ;
#61204 = CARTESIAN_POINT ( 'NONE',  ( 7.734375000614517326, 4.541064518000418104, 2.621784821874999949 ) ) ;
#61205 = CARTESIAN_POINT ( 'NONE',  ( 10.98750000122903536, 6.123233995736764310E-16, -4.999999999999998224 ) ) ;
#61206 = CARTESIAN_POINT ( 'NONE',  ( 17.51250000122903216, 0.000000000000000000, 4.999999999999998224 ) ) ;
#61207 = CARTESIAN_POINT ( 'NONE',  ( 14.91562500061451679, 3.027376345333611329, 5.243569643749999010 ) ) ;
#61208 = CARTESIAN_POINT ( 'NONE',  ( 18.29062500061451502, -3.027376345333610441, -5.243569643749999898 ) ) ;
#61209 = CARTESIAN_POINT ( 'NONE',  ( 26.13750000122903216, -4.330127018922194537, 2.499999999999995559 ) ) ;
#61210 = CARTESIAN_POINT ( 'NONE',  ( 27.22500000122903430, 2.886751345948129099, -4.999999999999998224 ) ) ;
#61211 = CARTESIAN_POINT ( 'NONE',  ( 23.21250000000000213, 2.886751345948126879, 4.999999999999999112 ) ) ;
#61212 = CARTESIAN_POINT ( 'NONE',  ( -7.967954043666661671E-16, 13.87812499938548250, 34.33755215474603517 ) ) ;
#61213 = CARTESIAN_POINT ( 'NONE',  ( 26.59687500061451360, 6.054752690667223547, 3.707466751127219781E-16 ) ) ;
#61214 = DIRECTION ( 'NONE',  ( -0.000000000000000000, -1.000000000000000000, -0.000000000000000000 ) ) ;
#61215 = CARTESIAN_POINT ( 'NONE',  ( 12.26250000122903394, -4.330127018922190985, -2.500000000000001332 ) ) ;
#61216 = CARTESIAN_POINT ( 'NONE',  ( 28.54687500061451644, -3.027376345333614438, 5.243569643749998122 ) ) ;
#61217 = CARTESIAN_POINT ( 'NONE',  ( -3.999999999999999112, 20.00000000000000000, -30.00000000000000000 ) ) ;
#61218 = CARTESIAN_POINT ( 'NONE',  ( 4.584375000614516971, 4.541064518000418104, 2.621784821874999949 ) ) ;
#61219 = B_SPLINE_CURVE_WITH_KNOTS ( 'NONE', 1,
 ( #45759, #63814 ),
 .UNSPECIFIED., .F., .F.,
 ( 2, 2 ),
 ( 0.000000000000000000, 1.000000000000000000 ),
 .UNSPECIFIED. ) ;
#61220 = CARTESIAN_POINT ( 'NONE',  ( 22.79062500061451502, -3.027376345333610441, -5.243569643749999898 ) ) ;
#61221 = CARTESIAN_POINT ( 'NONE',  ( -1.878215178125001827, 14.40312499938548463, 33.25316411605952283 ) ) ;
#61222 = CARTESIAN_POINT ( 'NONE',  ( 3.999999999999998668, 19.81250000000000000, -32.30940107675850470 ) ) ;
#61223 = CARTESIAN_POINT ( 'NONE',  ( 9.721875000614517148, -6.054752690667223547, -1.112240025338166033E-15 ) ) ;
#61224 = CARTESIAN_POINT ( 'NONE',  ( 3.647618174410700131, -3.419850926247963940, 3.721781544883157711 ) ) ;
#61225 = CARTESIAN_POINT ( 'NONE',  ( 29.61562500061451431, 3.027376345333613106, -5.243569643749998122 ) ) ;
#61226 = CARTESIAN_POINT ( 'NONE',  ( 5.259375000614518569, -4.541064518000417216, -2.621784821875001281 ) ) ;
#61227 = CARTESIAN_POINT ( 'NONE',  ( 27.68437500061451573, -4.541064518000419881, 2.621784821874995952 ) ) ;
#61228 = CARTESIAN_POINT ( 'NONE',  ( 4.243569643749999898, 11.02812500061459566, 30.00000000000000000 ) ) ;
#61229 = CARTESIAN_POINT ( 'NONE',  ( 20.66250000000000142, -5.773502691896255534, -1.060575238724906372E-15 ) ) ;
#61230 = ORIENTED_EDGE ( 'NONE', *, *, #16557, .F. ) ;
#61231 = CARTESIAN_POINT ( 'NONE',  ( 27.93750000000000000, -2.886751345948125991, -5.000000000000000000 ) ) ;
#61232 = CARTESIAN_POINT ( 'NONE',  ( 27.83437500061451786, 6.421520780324663323E-16, -5.243569643749999010 ) ) ;
#61233 = EDGE_CURVE ( 'NONE', #23988, #5357, #48499, .T. ) ;
#61234 = ORIENTED_EDGE ( 'NONE', *, *, #47659, .T. ) ;
#61235 = CARTESIAN_POINT ( 'NONE',  ( 16.75312500061451715, 0.000000000000000000, 5.243569643749999010 ) ) ;
#61236 = CARTESIAN_POINT ( 'NONE',  ( 9.065625000614517148, 3.027376345333611329, 5.243569643749999010 ) ) ;
#61237 = CARTESIAN_POINT ( 'NONE',  ( 21.64687500061451431, 0.000000000000000000, 4.756430356249998326 ) ) ;
#61238 = CARTESIAN_POINT ( 'NONE',  ( 7.284375000614518036, 4.541064518000418104, 2.621784821874999949 ) ) ;
#61239 = CARTESIAN_POINT ( 'NONE',  ( 17.43750000122903288, 4.330127018922191873, 2.499999999999999556 ) ) ;
#61240 = CARTESIAN_POINT ( 'NONE',  ( 23.81250000122903288, 0.000000000000000000, 4.999999999999998224 ) ) ;
#61241 = CARTESIAN_POINT ( 'NONE',  ( 7.096875000614517148, -3.027376345333610441, -5.243569643749999898 ) ) ;
#61242 = CARTESIAN_POINT ( 'NONE',  ( 12.04687500061451821, -3.027376345333610441, -5.243569643749999898 ) ) ;
#61243 = CARTESIAN_POINT ( 'NONE',  ( 24.15937500061451715, -4.541064518000417216, -2.621784821875001281 ) ) ;
#61244 = CARTESIAN_POINT ( 'NONE',  ( -3.999999999999999112, 16.40000000000000213, 30.00000000000000000 ) ) ;
#61245 = ORIENTED_EDGE ( 'NONE', *, *, #34819, .F. ) ;
#61246 = CARTESIAN_POINT ( 'NONE',  ( 9.899999999999998579, -4.330127018922190985, -2.500000000000001332 ) ) ;
#61247 = CARTESIAN_POINT ( 'NONE',  ( 16.84687500061451715, -3.027376345333614438, 5.243569643749998122 ) ) ;
#61248 = CARTESIAN_POINT ( 'NONE',  ( 9.309375000614517504, -4.541064518000417216, -2.621784821875001281 ) ) ;
#61249 = CARTESIAN_POINT ( 'NONE',  ( 3.756430356250000546, 15.82812499938548179, 27.83122392262697886 ) ) ;
#61250 = CARTESIAN_POINT ( 'NONE',  ( 20.54999999999999716, 0.000000000000000000, 4.999999999999998224 ) ) ;
#61251 = CARTESIAN_POINT ( 'NONE',  ( 4.000000000000000000, 16.58750000000000213, 27.69059892324149530 ) ) ;
#61252 = CARTESIAN_POINT ( 'NONE',  ( 4.243569643749999898, 10.59687500061451715, -27.54997392385601529 ) ) ;
#61253 = CARTESIAN_POINT ( 'NONE',  ( 22.69687500061451857, -2.746126346562646425, 4.756430356249996549 ) ) ;
#61254 = CARTESIAN_POINT ( 'NONE',  ( 11.65312500061451573, 4.541064518000418104, -2.621784821874998173 ) ) ;
#61255 = CARTESIAN_POINT ( 'NONE',  ( 27.94687500061451502, 6.054752690667223547, 3.707466751127219781E-16 ) ) ;
#61256 = CARTESIAN_POINT ( 'NONE',  ( -3.999999999999999112, 19.66250000122903430, 30.00000000000000000 ) ) ;
#61257 = CARTESIAN_POINT ( 'NONE',  ( 27.79687500061451999, -3.027376345333610441, -5.243569643749999898 ) ) ;
#61258 = CARTESIAN_POINT ( 'NONE',  ( 10.12500000000000178, 4.330127018922191873, 2.499999999999999556 ) ) ;
#61259 = CARTESIAN_POINT ( 'NONE',  ( 4.000000000000000000, 15.35000000122903252, 32.30940107675849049 ) ) ;
#61260 = CARTESIAN_POINT ( 'NONE',  ( 10.31250000122903288, 0.000000000000000000, 4.999999999999998224 ) ) ;
#61261 = CARTESIAN_POINT ( 'NONE',  ( 20.55937500061451573, -4.541064518000417216, -2.621784821875001281 ) ) ;
#61262 = CARTESIAN_POINT ( 'NONE',  ( 15.34687500061451537, 6.054752690667223547, 3.707466751127219781E-16 ) ) ;
#61263 = CARTESIAN_POINT ( 'NONE',  ( -5.000000000000004441, 6.123233995736764310E-16, -4.999999999999998224 ) ) ;
#61264 = ORIENTED_EDGE ( 'NONE', *, *, #41845, .T. ) ;
#61265 = CARTESIAN_POINT ( 'NONE',  ( 15.66562500061451857, 3.027376345333613106, -5.243569643749998122 ) ) ;
#61266 = CARTESIAN_POINT ( 'NONE',  ( 27.52500000122903145, -5.773502691896255534, -1.060575238724906372E-15 ) ) ;
#61267 = CARTESIAN_POINT ( 'NONE',  ( 15.98437500061451821, -4.541064518000419881, 2.621784821874995952 ) ) ;
#61268 = CARTESIAN_POINT ( 'NONE',  ( 3.215625000614518836, 3.027376345333611329, 5.243569643749999010 ) ) ;
#61269 = CARTESIAN_POINT ( 'NONE',  ( 16.64062500061451289, 6.054752690667223547, 3.707466751127219781E-16 ) ) ;
#61270 = EDGE_CURVE ( 'NONE', #24148, #9351, #42335, .T. ) ;
#61271 = DIRECTION ( 'NONE',  ( 0.000000000000000000, 0.000000000000000000, -1.000000000000000000 ) ) ;
#61272 = CARTESIAN_POINT ( 'NONE',  ( 25.69687500061451502, 6.054752690667223547, 3.707466751127219781E-16 ) ) ;
#61273 = CARTESIAN_POINT ( 'NONE',  ( 4.243569643749999898, 12.82812500061451821, 30.00000000000000000 ) ) ;
#61274 = CARTESIAN_POINT ( 'NONE',  ( 16.32187500061451502, 3.027376345333611329, 5.243569643749999010 ) ) ;
#61275 = CARTESIAN_POINT ( 'NONE',  ( 13.87500000122903465, 2.886751345948126879, 4.999999999999999112 ) ) ;
#61276 = CARTESIAN_POINT ( 'NONE',  ( 9.309375000614517504, -4.119189519843965641, -2.378215178125001383 ) ) ;
#61277 = CARTESIAN_POINT ( 'NONE',  ( 2.121784821875001281, 18.20937500061451786, -26.32496088578401938 ) ) ;
#61278 = CARTESIAN_POINT ( 'NONE',  ( 21.53437500061451715, 6.421520780324663323E-16, -5.243569643749999010 ) ) ;
#61279 = CARTESIAN_POINT ( 'NONE',  ( 22.16250000122903074, -4.330127018922190985, -2.500000000000001332 ) ) ;
#61280 = CARTESIAN_POINT ( 'NONE',  ( 16.17187500061451644, 3.027376345333613106, -5.243569643749998122 ) ) ;
#61281 = CARTESIAN_POINT ( 'NONE',  ( -3.000416591977282496E-16, 11.64687500061451786, 25.09994784771203058 ) ) ;
#61282 = CARTESIAN_POINT ( 'NONE',  ( 17.01562500061451644, 3.027376345333613106, -5.243569643749998122 ) ) ;
#61283 = VERTEX_POINT ( 'NONE', #3062 ) ;
#61284 = VERTEX_POINT ( 'NONE', #1083 ) ;
#61285 = CARTESIAN_POINT ( 'NONE',  ( 20.96250000000000213, 2.886751345948126879, 4.999999999999999112 ) ) ;
#61286 = DIRECTION ( 'NONE',  ( -1.000000000000000000, -0.000000000000000000, -0.000000000000000000 ) ) ;
#61287 = CARTESIAN_POINT ( 'NONE',  ( 24.29062500061451502, 6.054752690667223547, 3.707466751127219781E-16 ) ) ;
#61288 = CARTESIAN_POINT ( 'NONE',  ( 4.678125000614516971, -4.541064518000419881, 2.621784821874995952 ) ) ;
#61289 = CARTESIAN_POINT ( 'NONE',  ( 16.50000000122903288, 5.773502691896255534, 3.535250795749688894E-16 ) ) ;
#61290 = EDGE_CURVE ( 'NONE', #66075, #60322, #45594, .T. ) ;
#61291 = CARTESIAN_POINT ( 'NONE',  ( 21.81562500061451004, -6.054752690667223547, -1.112240025338166033E-15 ) ) ;
#61292 = CARTESIAN_POINT ( 'NONE',  ( 19.79999999999999716, -4.330127018922190985, -2.500000000000001332 ) ) ;
#61293 = CARTESIAN_POINT ( 'NONE',  ( 25.75312500061451715, 0.000000000000000000, 5.243569643749999010 ) ) ;
#61294 = CARTESIAN_POINT ( 'NONE',  ( 4.790625000614518569, -3.027376345333610441, -5.243569643749999898 ) ) ;
#61295 = ORIENTED_EDGE ( 'NONE', *, *, #51760, .F. ) ;
#61296 = CARTESIAN_POINT ( 'NONE',  ( 3.928125000614516527, 6.421520780324663323E-16, -5.243569643749999010 ) ) ;
#61297 = CARTESIAN_POINT ( 'NONE',  ( 10.39687500061451786, 5.492252693125287522, 3.363034840372157021E-16 ) ) ;
#61298 = DIRECTION ( 'NONE',  ( -1.000000000000000000, -0.000000000000000000, -0.000000000000000000 ) ) ;
#61299 = CARTESIAN_POINT ( 'NONE',  ( 3.999999999999998668, 10.47500000122903430, -32.30940107675850470 ) ) ;
#61300 = CARTESIAN_POINT ( 'NONE',  ( -4.243569643749999898, 17.60937500061451999, -30.00000000000000000 ) ) ;
#61301 = CARTESIAN_POINT ( 'NONE',  ( 7.612500000000000711, -5.773502691896255534, -1.060575238724906372E-15 ) ) ;
#61302 = CARTESIAN_POINT ( 'NONE',  ( 8.896875000614517859, -3.027376345333610441, -5.243569643749999898 ) ) ;
#61303 = CARTESIAN_POINT ( 'NONE',  ( 7.350000001229033408, -2.886751345948125991, -5.000000000000000000 ) ) ;
#61304 = CARTESIAN_POINT ( 'NONE',  ( 13.17187500061451999, 3.027376345333611329, 5.243569643749999010 ) ) ;
#61305 = CARTESIAN_POINT ( 'NONE',  ( 3.496875000614518836, -3.027376345333610441, -5.243569643749999898 ) ) ;
#61306 = FACE_OUTER_BOUND ( 'NONE', #64119, .T. ) ;
#61307 = AXIS2_PLACEMENT_3D ( 'NONE', #41500, #32152, #32518 ) ;
#61308 = CARTESIAN_POINT ( 'NONE',  ( 9.999999999999992895, -5.857864376269048101, -9.999999999999992895 ) ) ;
#61309 = CARTESIAN_POINT ( 'NONE',  ( 9.684375000614517504, -4.541064518000419881, 2.621784821874995952 ) ) ;
#61310 = CARTESIAN_POINT ( 'NONE',  ( 26.73750000122903003, 6.123233995736764310E-16, -4.999999999999998224 ) ) ;
#61311 = CARTESIAN_POINT ( 'NONE',  ( 19.26562500061451644, 3.027376345333613106, -5.243569643749998122 ) ) ;
#61312 = CARTESIAN_POINT ( 'NONE',  ( 2.121784821875001281, 19.05312500061459602, 33.67503911421598417 ) ) ;
#61313 = CARTESIAN_POINT ( 'NONE',  ( 23.70937500061451786, -4.541064518000417216, -2.621784821875001281 ) ) ;
#61314 = CARTESIAN_POINT ( 'NONE',  ( 29.58749999999999858, -2.886751345948150860, 4.999999999999960920 ) ) ;
#61315 = CARTESIAN_POINT ( 'NONE',  ( 3.140625000614516882, 6.054752690667223547, 3.707466751127219781E-16 ) ) ;
#61316 = CARTESIAN_POINT ( 'NONE',  ( 21.27187500061451431, -4.119189519843968306, 2.378215178124996054 ) ) ;
#61317 = CARTESIAN_POINT ( 'NONE',  ( 25.56562500061452070, 3.027376345333613106, -5.243569643749998122 ) ) ;
#61318 = CARTESIAN_POINT ( 'NONE',  ( 14.46562500061451750, 3.027376345333611329, 5.243569643749999010 ) ) ;
#61319 = CARTESIAN_POINT ( 'NONE',  ( 15.35625000122903216, -4.330127018922190985, -2.500000000000001332 ) ) ;
#61320 = CARTESIAN_POINT ( 'NONE',  ( 13.39687500061451608, -3.027376345333610441, -5.243569643749999898 ) ) ;
#61321 = CARTESIAN_POINT ( 'NONE',  ( 24.97500000122903430, 2.886751345948129099, -4.999999999999998224 ) ) ;
#61322 = CARTESIAN_POINT ( 'NONE',  ( 3.571875000614517237, 3.027376345333613106, -5.243569643749998122 ) ) ;
#61323 = CARTESIAN_POINT ( 'NONE',  ( 13.84687500061451537, -3.027376345333610441, -5.243569643749999898 ) ) ;
#61324 = CARTESIAN_POINT ( 'NONE',  ( 15.00000000000000000, 4.330127018922192761, -2.499999999999997780 ) ) ;
#61325 = CYLINDRICAL_SURFACE ( 'NONE', #70195, 4.999999999999998224 ) ;
#61326 = CARTESIAN_POINT ( 'NONE',  ( -5.810221930991193690E-16, 12.23750000000000071, -34.00000000000000000 ) ) ;
#61327 = CARTESIAN_POINT ( 'NONE',  ( 25.77187500061451075, 3.027376345333611329, 5.243569643749999010 ) ) ;
#61328 = CARTESIAN_POINT ( 'NONE',  ( 15.53437500061451715, -4.541064518000419881, 2.621784821874995952 ) ) ;
#61329 = CARTESIAN_POINT ( 'NONE',  ( 1.878215178125000495, 15.52812499938548285, 26.74683588394047007 ) ) ;
#61330 = CARTESIAN_POINT ( 'NONE',  ( 27.03750000000000142, -2.886751345948125991, -5.000000000000000000 ) ) ;
#61331 = CARTESIAN_POINT ( 'NONE',  ( 3.225000001229033408, -5.773502691896255534, -1.060575238724906372E-15 ) ) ;
#61332 = CARTESIAN_POINT ( 'NONE',  ( 4.762499999999999289, 2.886751345948126879, 4.999999999999999112 ) ) ;
#61333 = CARTESIAN_POINT ( 'NONE',  ( 7.284375000614517148, -2.746126346562646425, 4.756430356249996549 ) ) ;
#61334 = CARTESIAN_POINT ( 'NONE',  ( 18.89062500061451644, 6.054752690667223547, 3.707466751127219781E-16 ) ) ;
#61335 = CARTESIAN_POINT ( 'NONE',  ( 8.812500000000000000, 2.886751345948126879, 4.999999999999999112 ) ) ;
#61336 = ADVANCED_FACE ( 'NONE', ( #62392 ), #46136, .F. ) ;
#61337 = CARTESIAN_POINT ( 'NONE',  ( -0.7157356635157281488, 9.902086024390941432, 25.94083351194041143 ) ) ;
#61338 = CARTESIAN_POINT ( 'NONE',  ( 18.11250000000000071, 2.886751345948129099, -4.999999999999998224 ) ) ;
#61339 = CARTESIAN_POINT ( 'NONE',  ( 45.00000000000000000, 0.000000000000000000, 4.999999999999998224 ) ) ;
#61340 = CARTESIAN_POINT ( 'NONE',  ( 20.81250000122903643, -4.330127018922190985, -2.500000000000001332 ) ) ;
#61341 = CARTESIAN_POINT ( 'NONE',  ( 15.00000000000000000, 4.330127018922192761, -2.499999999999997780 ) ) ;
#61342 = CARTESIAN_POINT ( 'NONE',  ( 27.30937500061451573, -4.541064518000417216, -2.621784821875001281 ) ) ;
#61343 = ORIENTED_EDGE ( 'NONE', *, *, #65260, .F. ) ;
#61344 = CARTESIAN_POINT ( 'NONE',  ( 17.61562500061451786, 3.027376345333611329, 5.243569643749999010 ) ) ;
#61345 = CARTESIAN_POINT ( 'NONE',  ( 23.80312500061451786, 4.541064518000418104, -2.621784821874998173 ) ) ;
#61346 = CARTESIAN_POINT ( 'NONE',  ( 23.37187500061451573, 3.027376345333613106, -5.243569643749998122 ) ) ;
#61347 = CARTESIAN_POINT ( 'NONE',  ( 6.637500000000001066, -2.886751345948129988, 4.999999999999997335 ) ) ;
#61348 = CARTESIAN_POINT ( 'NONE',  ( 8.840625000614515727, -3.027376345333610441, -5.243569643749999898 ) ) ;
#61349 = CARTESIAN_POINT ( 'NONE',  ( 25.11562500061451431, 3.027376345333613106, -5.243569643749998122 ) ) ;
#61350 = CARTESIAN_POINT ( 'NONE',  ( 14.10937500061451644, 0.000000000000000000, 5.243569643749999010 ) ) ;
#61351 = CARTESIAN_POINT ( 'NONE',  ( 19.58437500061451786, -4.541064518000419881, 2.621784821874995952 ) ) ;
#61352 = CARTESIAN_POINT ( 'NONE',  ( 1.626862140677534273E-15, 11.67500000122903181, -26.00000000000000355 ) ) ;
#61353 = CARTESIAN_POINT ( 'NONE',  ( 9.001249775931846008E-16, 10.07187500061451857, 34.90005215228797653 ) ) ;
#61354 = CARTESIAN_POINT ( 'NONE',  ( 21.03750000122903074, 4.330127018922191873, 2.499999999999999556 ) ) ;
#61355 = CARTESIAN_POINT ( 'NONE',  ( 18.15937500061451715, 0.000000000000000000, 4.756430356249998326 ) ) ;
#61356 = CARTESIAN_POINT ( 'NONE',  ( 11.27812500061451573, 4.541064518000418104, 2.621784821874999949 ) ) ;
#61357 = CARTESIAN_POINT ( 'NONE',  ( 7.696875000614516793, 6.054752690667223547, 3.707466751127219781E-16 ) ) ;
#61358 = CARTESIAN_POINT ( 'NONE',  ( 6.384375000614516793, 4.541064518000418104, 2.621784821874999949 ) ) ;
#61359 = ORIENTED_EDGE ( 'NONE', *, *, #16377, .F. ) ;
#61360 = CARTESIAN_POINT ( 'NONE',  ( 27.34687500061451360, -3.027376345333610441, -5.243569643749999898 ) ) ;
#61361 = CARTESIAN_POINT ( 'NONE',  ( 20.01562500061451644, -6.054752690667223547, -1.112240025338166033E-15 ) ) ;
#61362 = CARTESIAN_POINT ( 'NONE',  ( 3.515625000614516882, 3.027376345333613106, -5.243569643749998122 ) ) ;
#61363 = CARTESIAN_POINT ( 'NONE',  ( 27.89062500061451289, 6.054752690667223547, 3.707466751127219781E-16 ) ) ;
#61364 = CARTESIAN_POINT ( 'NONE',  ( 23.85937500061451644, 4.541064518000418104, -2.621784821874998173 ) ) ;
#61365 = CARTESIAN_POINT ( 'NONE',  ( 18.59062500061451573, -3.027376345333614438, 5.243569643749998122 ) ) ;
#61366 = CARTESIAN_POINT ( 'NONE',  ( -4.243569643749999898, 18.47187500061451715, 27.54997392385601529 ) ) ;
#61367 = CARTESIAN_POINT ( 'NONE',  ( 25.45312500061451644, -4.541064518000417216, -2.621784821875001281 ) ) ;
#61368 = CARTESIAN_POINT ( 'NONE',  ( 5.887500001229034829, -4.330127018922194537, 2.499999999999995559 ) ) ;
#61369 = ORIENTED_EDGE ( 'NONE', *, *, #39433, .T. ) ;
#61370 = CARTESIAN_POINT ( 'NONE',  ( 28.76249999999999929, -5.773502691896255534, -1.060575238724906372E-15 ) ) ;
#61371 = CARTESIAN_POINT ( 'NONE',  ( 4.000000000000000000, 16.13749999999999929, -27.69059892324149530 ) ) ;
#61372 = CARTESIAN_POINT ( 'NONE',  ( 3.756430356249998770, 18.11562499938547788, 32.16877607737302469 ) ) ;
#61373 = CARTESIAN_POINT ( 'NONE',  ( 3.834375000614519635, -4.541064518000419881, 2.621784821874995952 ) ) ;
#61374 = CARTESIAN_POINT ( 'NONE',  ( 13.11562500061451786, 3.027376345333611329, 5.243569643749999010 ) ) ;
#61375 = CARTESIAN_POINT ( 'NONE',  ( 6.609375000614519102, -4.541064518000417216, -2.621784821875001281 ) ) ;
#61376 = CARTESIAN_POINT ( 'NONE',  ( 24.30000000122903359, -2.886751345948129988, 4.999999999999997335 ) ) ;
#61377 =( BOUNDED_CURVE ( )  B_SPLINE_CURVE ( 2, ( #63586, #18867, #46971, #1186, #63223, #52869, #24422 ),
 .UNSPECIFIED., .F., .F. ) 
 B_SPLINE_CURVE_WITH_KNOTS ( ( 3, 2, 2, 3 ),
 ( 0.4700000000000001399, 0.4733333333333334392, 0.4766666666666666829, 0.4799999999999999267 ),
 .UNSPECIFIED. ) 
 CURVE ( )  GEOMETRIC_REPRESENTATION_ITEM ( )  RATIONAL_B_SPLINE_CURVE ( ( 0.9999999999999933387, 0.8660254037844453689, 1.000000000000000000, 0.8660254037844387076, 1.000000000000000000, 0.8660254037844409281, 0.9999999999999977796 ) ) 
 REPRESENTATION_ITEM ( '' )  );
#61378 = CARTESIAN_POINT ( 'NONE',  ( 15.87187500061451573, 3.027376345333611329, 5.243569643749999010 ) ) ;
#61379 = CARTESIAN_POINT ( 'NONE',  ( 3.009375000614516793, -4.541064518000417216, -2.621784821875001281 ) ) ;
#61380 = CARTESIAN_POINT ( 'NONE',  ( 29.77499999999999858, 6.123233995736764310E-16, -4.999999999999998224 ) ) ;
#61381 = CARTESIAN_POINT ( 'NONE',  ( 27.49687500061451217, 6.054752690667223547, 3.707466751127219781E-16 ) ) ;
#61382 = CARTESIAN_POINT ( 'NONE',  ( 3.253125000614518036, 0.000000000000000000, 5.243569643749999010 ) ) ;
#61383 = CARTESIAN_POINT ( 'NONE',  ( 12.14062500061451821, 6.054752690667223547, 3.707466751127219781E-16 ) ) ;
#61384 = ORIENTED_EDGE ( 'NONE', *, *, #32153, .F. ) ;
#61385 = CARTESIAN_POINT ( 'NONE',  ( 9.928125000614517859, 4.541064518000418104, 2.621784821874999949 ) ) ;
#61386 = CARTESIAN_POINT ( 'NONE',  ( 7.303125000614516082, 0.000000000000000000, 5.243569643749999010 ) ) ;
#61387 = CARTESIAN_POINT ( 'NONE',  ( 18.08437500061451431, 4.119189519843966529, 2.378215178124999607 ) ) ;
#61388 = CARTESIAN_POINT ( 'NONE',  ( 9.449999999999999289, -4.330127018922190985, -2.500000000000001332 ) ) ;
#61389 = EDGE_CURVE ( 'NONE', #15981, #38080, #15367, .T. ) ;
#61390 = CARTESIAN_POINT ( 'NONE',  ( 2.925000001229034918, 2.886751345948129099, -4.999999999999998224 ) ) ;
#61391 = CARTESIAN_POINT ( 'NONE',  ( 18.18750000000000000, 5.773502691896255534, 3.535250795749688894E-16 ) ) ;
#61392 =( BOUNDED_CURVE ( )  B_SPLINE_CURVE ( 2, ( #48664, #47936, #8768, #54568, #32032, #37936, #8401 ),
 .UNSPECIFIED., .F., .F. ) 
 B_SPLINE_CURVE_WITH_KNOTS ( ( 3, 2, 2, 3 ),
 ( 0.02499999999999994935, 0.02777777777777776236, 0.03055555555555557884, 0.03333333333333339532 ),
 .UNSPECIFIED. ) 
 CURVE ( )  GEOMETRIC_REPRESENTATION_ITEM ( )  RATIONAL_B_SPLINE_CURVE ( ( 1.000000000000002442, 0.8660254037844360431, 1.000000000000000000, 0.8660254037844387076, 1.000000000000000000, 0.8660254037844357100, 1.000000000000003109 ) ) 
 REPRESENTATION_ITEM ( '' )  );
#61393 = CARTESIAN_POINT ( 'NONE',  ( 16.09687500061452070, -3.027376345333610441, -5.243569643749999898 ) ) ;
#61394 = CARTESIAN_POINT ( 'NONE',  ( 12.82500000122903394, 2.886751345948129099, -4.999999999999998224 ) ) ;
#61395 = CARTESIAN_POINT ( 'NONE',  ( 20.17499999999999716, -4.330127018922194537, 2.499999999999995559 ) ) ;
#61396 = CARTESIAN_POINT ( 'NONE',  ( 9.001249775931846008E-16, 14.51562500061451466, -25.09994784771203058 ) ) ;
#61397 = CARTESIAN_POINT ( 'NONE',  ( -1.071796769724492115, 20.01740381056766438, 34.00000000000000000 ) ) ;
#61398 = CARTESIAN_POINT ( 'NONE',  ( 26.25937500061451502, -5.492252693125287522, -1.008910452111647106E-15 ) ) ;
#61399 = CARTESIAN_POINT ( 'NONE',  ( 26.50312500061451360, 4.541064518000418104, -2.621784821874998173 ) ) ;
#61400 = CARTESIAN_POINT ( 'NONE',  ( 1.999999999999998668, 19.84999999999999787, 26.53589838486224650 ) ) ;
#61401 = CARTESIAN_POINT ( 'NONE',  ( 17.39999999999999858, 0.000000000000000000, 4.999999999999998224 ) ) ;
#61402 = CARTESIAN_POINT ( 'NONE',  ( 25.87500000000000000, 4.330127018922191873, 2.499999999999999556 ) ) ;
#61403 = CARTESIAN_POINT ( 'NONE',  ( 9.665625000614515017, -6.054752690667223547, -1.112240025338166033E-15 ) ) ;
#61404 = CARTESIAN_POINT ( 'NONE',  ( 28.05937500061451217, -5.492252693125287522, -1.008910452111647106E-15 ) ) ;
#61405 =( BOUNDED_CURVE ( )  B_SPLINE_CURVE ( 2, ( #70719, #37099, #43017, #59624, #31933, #26391, #2761 ),
 .UNSPECIFIED., .F., .F. ) 
 B_SPLINE_CURVE_WITH_KNOTS ( ( 3, 2, 2, 3 ),
 ( 0.3250000000000000111, 0.3277777777777777790, 0.3305555555555556024, 0.3333333333333333703 ),
 .UNSPECIFIED. ) 
 CURVE ( )  GEOMETRIC_REPRESENTATION_ITEM ( )  RATIONAL_B_SPLINE_CURVE ( ( 1.000000000000000000, 0.8660254037844387076, 1.000000000000000000, 0.8660254037844387076, 1.000000000000000000, 0.8660254037844360431, 1.000000000000002665 ) ) 
 REPRESENTATION_ITEM ( '' )  );
#61406 = CARTESIAN_POINT ( 'NONE',  ( 22.24687500061451217, -3.027376345333614438, 5.243569643749998122 ) ) ;
#61407 = CARTESIAN_POINT ( 'NONE',  ( 13.05937500061451750, 2.746126346562643317, 4.756430356249998326 ) ) ;
#61408 = CARTESIAN_POINT ( 'NONE',  ( 4.640625000614518214, -3.027376345333614438, 5.243569643749998122 ) ) ;
#61409 = CARTESIAN_POINT ( 'NONE',  ( 11.22187500061451892, 3.027376345333613106, -5.243569643749998122 ) ) ;
#61410 = ORIENTED_EDGE ( 'NONE', *, *, #46133, .T. ) ;
#61411 = CARTESIAN_POINT ( 'NONE',  ( 21.42187500061451644, -6.054752690667223547, -1.112240025338166033E-15 ) ) ;
#61412 = CYLINDRICAL_SURFACE ( 'NONE', #20740, 4.999999999999998224 ) ;
#61413 = CARTESIAN_POINT ( 'NONE',  ( 29.66249999999999432, -5.773502691896255534, -1.060575238724906372E-15 ) ) ;
#61414 = EDGE_CURVE ( 'NONE', #43575, #61054, #14941, .T. ) ;
#61415 = CARTESIAN_POINT ( 'NONE',  ( 5.549999999999998934, 4.330127018922192761, -2.499999999999997780 ) ) ;
#61416 = CARTESIAN_POINT ( 'NONE',  ( 13.87500000122903465, 2.886751345948126879, 4.999999999999999112 ) ) ;
#61417 = CARTESIAN_POINT ( 'NONE',  ( 1.592000809091587073E-14, 15.38750000000000284, -34.00000000000000000 ) ) ;
#61418 = CARTESIAN_POINT ( 'NONE',  ( 18.75000000000000000, 0.000000000000000000, 4.999999999999998224 ) ) ;
#61419 = VERTEX_POINT ( 'NONE', #16955 ) ;
#61420 = CARTESIAN_POINT ( 'NONE',  ( 13.72500000000000142, 4.330127018922191873, 2.499999999999999556 ) ) ;
#61421 = CARTESIAN_POINT ( 'NONE',  ( 16.16250000000000142, -5.773502691896255534, -1.060575238724906372E-15 ) ) ;
#61422 = CARTESIAN_POINT ( 'NONE',  ( 13.95000000122903572, -2.886751345948129988, 4.999999999999997335 ) ) ;
#61423 = CARTESIAN_POINT ( 'NONE',  ( 12.25312500061451537, 0.000000000000000000, 5.243569643749999010 ) ) ;
#61424 = CARTESIAN_POINT ( 'NONE',  ( 9.937500000000001776, -2.886751345948125991, -5.000000000000000000 ) ) ;
#61425 = CARTESIAN_POINT ( 'NONE',  ( -3.999999999999999112, 15.61250000122903359, 30.00000000000000000 ) ) ;
#61426 = CARTESIAN_POINT ( 'NONE',  ( -4.243569643749999898, 14.45937500061451964, -30.00000000000000000 ) ) ;
#61427 = CARTESIAN_POINT ( 'NONE',  ( 27.37500000122903288, 2.886751345948126879, 4.999999999999999112 ) ) ;
#61428 = CARTESIAN_POINT ( 'NONE',  ( -1.878215178124999163, 15.04062499938548392, 26.74683588394047007 ) ) ;
#61429 = CARTESIAN_POINT ( 'NONE',  ( 9.337500000000000355, -2.886751345948129988, 4.999999999999997335 ) ) ;
#61430 = CYLINDRICAL_SURFACE ( 'NONE', #796, 4.000000000000000000 ) ;
#61431 = ORIENTED_EDGE ( 'NONE', *, *, #35197, .T. ) ;
#61432 = CARTESIAN_POINT ( 'NONE',  ( 24.59062500061451573, -3.027376345333610441, -5.243569643749999898 ) ) ;
#61433 = CARTESIAN_POINT ( 'NONE',  ( 3.612401643004526264, 3.457069727864729991, 3.855493425756290282 ) ) ;
#61434 = CARTESIAN_POINT ( 'NONE',  ( 29.67187500061451644, 3.027376345333613106, -5.243569643749998122 ) ) ;
#61435 = CARTESIAN_POINT ( 'NONE',  ( 21.23437500061451644, 4.541064518000418104, 2.621784821874999949 ) ) ;
#61436 = CARTESIAN_POINT ( 'NONE',  ( 15.89062500061451289, -3.027376345333614438, 5.243569643749998122 ) ) ;
#61437 = CARTESIAN_POINT ( 'NONE',  ( -4.243569643749999898, 10.76562500061459637, -32.45002607614398471 ) ) ;
#61438 = CARTESIAN_POINT ( 'NONE',  ( 7.003125000614518036, -4.541064518000417216, -2.621784821875001281 ) ) ;
#61439 = CARTESIAN_POINT ( 'NONE',  ( 28.72500000122903074, 2.886751345948126879, 4.999999999999999112 ) ) ;
#61440 = CARTESIAN_POINT ( 'NONE',  ( 23.63437500061451502, -4.119189519843968306, 2.378215178124996054 ) ) ;
#61441 = CARTESIAN_POINT ( 'NONE',  ( 17.99062500061451786, 6.054752690667223547, 3.707466751127219781E-16 ) ) ;
#61442 = CARTESIAN_POINT ( 'NONE',  ( 8.146875000614516082, 5.492252693125287522, 3.363034840372157021E-16 ) ) ;
#61443 = CARTESIAN_POINT ( 'NONE',  ( -3.756430356250001434, 19.20312499938548356, 32.16877607737301048 ) ) ;
#61444 = CARTESIAN_POINT ( 'NONE',  ( 15.90937500061451892, 0.000000000000000000, 5.243569643749999010 ) ) ;
#61445 = CARTESIAN_POINT ( 'NONE',  ( 14.63437500061451679, -4.541064518000419881, 2.621784821874995952 ) ) ;
#61446 = CARTESIAN_POINT ( 'NONE',  ( 22.13437500061451502, 4.541064518000418104, 2.621784821874999949 ) ) ;
#61447 = EDGE_LOOP ( 'NONE', ( #291, #13681, #1268, #72192 ) ) ;
#61448 = CARTESIAN_POINT ( 'NONE',  ( -2.121784821874999949, 11.68437500061451750, 26.32496088578401938 ) ) ;
#61449 = CARTESIAN_POINT ( 'NONE',  ( -3.999999999999997335, 14.75000000122903288, -27.69059892324149530 ) ) ;
#61450 = CARTESIAN_POINT ( 'NONE',  ( 27.66562500061451146, -6.054752690667223547, -1.112240025338166033E-15 ) ) ;
#61451 = CARTESIAN_POINT ( 'NONE',  ( 26.87812500061451360, 6.421520780324663323E-16, -5.243569643749999010 ) ) ;
#61452 = CARTESIAN_POINT ( 'NONE',  ( 4.000000000000000000, 19.40000000122903856, -27.69059892324149885 ) ) ;
#61453 = CARTESIAN_POINT ( 'NONE',  ( 3.999999999999998668, 16.66249999999999787, 27.69059892324149175 ) ) ;
#61454 = CARTESIAN_POINT ( 'NONE',  ( 5.596875000614516260, -3.027376345333614438, 5.243569643749998122 ) ) ;
#61455 = CARTESIAN_POINT ( 'NONE',  ( 12.78750000122903430, 6.123233995736764310E-16, -4.999999999999998224 ) ) ;
#61456 = CARTESIAN_POINT ( 'NONE',  ( 7.425000001229034474, 2.886751345948129099, -4.999999999999998224 ) ) ;
#61457 = CARTESIAN_POINT ( 'NONE',  ( 29.32500000122903216, -5.773502691896255534, -1.060575238724906372E-15 ) ) ;
#61458 = CARTESIAN_POINT ( 'NONE',  ( -1.999999999999999112, 18.89374999877096784, 26.53589838486224650 ) ) ;
#61459 = CARTESIAN_POINT ( 'NONE',  ( 18.13125000122903074, 6.123233995736764310E-16, -4.999999999999998224 ) ) ;
#61460 = CARTESIAN_POINT ( 'NONE',  ( 11.70937500061451608, 4.541064518000418104, -2.621784821874998173 ) ) ;
#61461 = DIRECTION ( 'NONE',  ( 0.000000000000000000, 0.000000000000000000, -1.000000000000000000 ) ) ;
#61462 = ORIENTED_EDGE ( 'NONE', *, *, #71351, .T. ) ;
#61463 = CARTESIAN_POINT ( 'NONE',  ( 20.46562500061451928, -6.054752690667223547, -1.112240025338166033E-15 ) ) ;
#61464 = CARTESIAN_POINT ( 'NONE',  ( 13.58437500061451786, 4.541064518000418104, 2.621784821874999949 ) ) ;
#61465 = CARTESIAN_POINT ( 'NONE',  ( 5.615625000614517859, -6.054752690667223547, -1.112240025338166033E-15 ) ) ;
#61466 = CARTESIAN_POINT ( 'NONE',  ( 22.69687500061451857, -3.027376345333614438, 5.243569643749998122 ) ) ;
#61467 = CARTESIAN_POINT ( 'NONE',  ( 10.95937500061451964, 0.000000000000000000, 5.243569643749999010 ) ) ;
#61468 = CARTESIAN_POINT ( 'NONE',  ( 4.490625000614516971, 6.054752690667223547, 3.707466751127219781E-16 ) ) ;
#61469 = CARTESIAN_POINT ( 'NONE',  ( 10.83750000122903501, -4.330127018922194537, 2.499999999999995559 ) ) ;
#61470 = CARTESIAN_POINT ( 'NONE',  ( 5.775000001229033231, 2.886751345948126879, 4.999999999999999112 ) ) ;
#61471 = CARTESIAN_POINT ( 'NONE',  ( 20.50312500061451715, -4.541064518000417216, -2.621784821875001281 ) ) ;
#61472 = CARTESIAN_POINT ( 'NONE',  ( 7.462500001229035007, 4.330127018922192761, -2.499999999999997780 ) ) ;
#61473 = CARTESIAN_POINT ( 'NONE',  ( 17.05312500061451786, 4.541064518000418104, -2.621784821874998173 ) ) ;
#61474 = CARTESIAN_POINT ( 'NONE',  ( 15.36562500061451608, 3.027376345333611329, 5.243569643749999010 ) ) ;
#61475 = CARTESIAN_POINT ( 'NONE',  ( 26.18437500061451573, 4.119189519843966529, 2.378215178124999607 ) ) ;
#61476 = CARTESIAN_POINT ( 'NONE',  ( 16.42500000000000071, 4.330127018922191873, 2.499999999999999556 ) ) ;
#61477 = CARTESIAN_POINT ( 'NONE',  ( 10.01250000122903394, -4.330127018922190985, -2.500000000000001332 ) ) ;
#61478 = CARTESIAN_POINT ( 'NONE',  ( 6.065625000614516260, -6.054752690667223547, -1.112240025338166033E-15 ) ) ;
#61479 = ADVANCED_FACE ( 'NONE', ( #6617 ), #18037, .F. ) ;
#61480 = CARTESIAN_POINT ( 'NONE',  ( 20.10000000122903074, 5.773502691896255534, 3.535250795749688894E-16 ) ) ;
#61481 = CARTESIAN_POINT ( 'NONE',  ( 27.89999999999999858, -4.330127018922190985, -2.500000000000001332 ) ) ;
#61482 = CARTESIAN_POINT ( 'NONE',  ( 4.243569643749999898, 12.39687500061451608, -27.54997392385601529 ) ) ;
#61483 = CARTESIAN_POINT ( 'NONE',  ( 21.33749999999999858, 5.773502691896255534, 3.535250795749688401E-16 ) ) ;
#61484 = CARTESIAN_POINT ( 'NONE',  ( 4.012500001229033053, 0.000000000000000000, 4.999999999999998224 ) ) ;
#61485 = CARTESIAN_POINT ( 'NONE',  ( 3.946875000614517681, -3.027376345333610441, -5.243569643749999898 ) ) ;
#61486 = CARTESIAN_POINT ( 'NONE',  ( 19.80937500061451573, 4.541064518000418104, -2.621784821874998173 ) ) ;
#61487 = CARTESIAN_POINT ( 'NONE',  ( 8.775000000000002132, 4.330127018922191873, 2.499999999999999556 ) ) ;
#61488 = CARTESIAN_POINT ( 'NONE',  ( 15.44062500061451537, -3.027376345333614438, 5.243569643749998122 ) ) ;
#61489 = CARTESIAN_POINT ( 'NONE',  ( 12.88125000122903430, 4.330127018922191873, 2.499999999999999556 ) ) ;
#61490 = CARTESIAN_POINT ( 'NONE',  ( -1.999999999999997113, 15.57500000000000284, -26.53589838486224295 ) ) ;
#61491 = DIRECTION ( 'NONE',  ( -0.000000000000000000, -1.000000000000000000, -0.000000000000000000 ) ) ;
#61492 = CARTESIAN_POINT ( 'NONE',  ( 29.25937500061451502, 4.541064518000418104, -2.621784821874998173 ) ) ;
#61493 = CARTESIAN_POINT ( 'NONE',  ( 20.59687500061451715, 4.119189519843966529, -2.378215178124998275 ) ) ;
#61494 = CARTESIAN_POINT ( 'NONE',  ( 14.12812500061451715, -4.541064518000419881, 2.621784821874995952 ) ) ;
#61495 = CARTESIAN_POINT ( 'NONE',  ( 11.03437500061451715, -4.541064518000419881, 2.621784821874995952 ) ) ;
#61496 = VERTEX_POINT ( 'NONE', #22857 ) ;
#61497 = CARTESIAN_POINT ( 'NONE',  ( 28.86562500061451786, 3.027376345333611329, 5.243569643749999010 ) ) ;
#61498 = CARTESIAN_POINT ( 'NONE',  ( 22.19062500061451715, -3.027376345333614438, 5.243569643749998122 ) ) ;
#61499 = DIRECTION ( 'NONE',  ( -1.000000000000000000, -0.000000000000000000, -0.000000000000000000 ) ) ;
#61500 = CARTESIAN_POINT ( 'NONE',  ( 11.62500000000000000, -4.330127018922194537, 2.499999999999995559 ) ) ;
#61501 = CARTESIAN_POINT ( 'NONE',  ( 21.93750000122903288, 4.330127018922191873, 2.499999999999999556 ) ) ;
#61502 = CARTESIAN_POINT ( 'NONE',  ( 17.27812500061451217, -4.541064518000419881, 2.621784821874995952 ) ) ;
#61503 = CARTESIAN_POINT ( 'NONE',  ( 12.60937500061451289, 2.746126346562643317, 4.756430356249998326 ) ) ;
#61504 = ORIENTED_EDGE ( 'NONE', *, *, #22002, .F. ) ;
#61505 = CARTESIAN_POINT ( 'NONE',  ( 19.34999999999999787, -4.330127018922190985, -2.500000000000001332 ) ) ;
#61506 = CARTESIAN_POINT ( 'NONE',  ( 22.24687500061451217, -3.027376345333614438, 5.243569643749998122 ) ) ;
#61507 = CARTESIAN_POINT ( 'NONE',  ( 27.77812500061451573, 6.421520780324663323E-16, -5.243569643749999010 ) ) ;
#61508 = EDGE_CURVE ( 'NONE', #46924, #4424, #24845, .T. ) ;
#61509 = ORIENTED_EDGE ( 'NONE', *, *, #72508, .F. ) ;
#61510 = CARTESIAN_POINT ( 'NONE',  ( 7.453125000614516438, -4.541064518000417216, -2.621784821875001281 ) ) ;
#61511 = CARTESIAN_POINT ( 'NONE',  ( 3.300686927427837425, 3.755761153797071206, 3.532840975251721805 ) ) ;
#61512 = CARTESIAN_POINT ( 'NONE',  ( 17.58749999999999858, -2.886751345948125991, -5.000000000000000000 ) ) ;
#61513 = CARTESIAN_POINT ( 'NONE',  ( 25.50000000000000000, 0.000000000000000000, 4.999999999999998224 ) ) ;
#61514 = CARTESIAN_POINT ( 'NONE',  ( 5.924999999999999822, 6.123233995736764310E-16, -4.999999999999998224 ) ) ;
#61515 = CARTESIAN_POINT ( 'NONE',  ( 3.609375000614516882, 4.541064518000418104, -2.621784821874998173 ) ) ;
#61516 = CARTESIAN_POINT ( 'NONE',  ( 29.67187500061451644, 3.027376345333613106, -5.243569643749998122 ) ) ;
#61517 = ORIENTED_EDGE ( 'NONE', *, *, #41396, .F. ) ;
#61518 = CARTESIAN_POINT ( 'NONE',  ( 23.09062500061451573, -3.027376345333614438, 5.243569643749998122 ) ) ;
#61519 = CARTESIAN_POINT ( 'NONE',  ( 24.34687500061451715, 6.054752690667223547, 3.707466751127219781E-16 ) ) ;
#61520 = CARTESIAN_POINT ( 'NONE',  ( 4.243569643749999898, 19.12812500061459531, -30.00000000000000000 ) ) ;
#61521 = CARTESIAN_POINT ( 'NONE',  ( 14.69999999999999929, 0.000000000000000000, 4.999999999999998224 ) ) ;
#61522 = CARTESIAN_POINT ( 'NONE',  ( 7.753125000614518036, 0.000000000000000000, 5.243569643749999010 ) ) ;
#61523 = CARTESIAN_POINT ( 'NONE',  ( 1.071796769724500997, 17.30134618820330417, 33.99999999999999289 ) ) ;
#61524 = CARTESIAN_POINT ( 'NONE',  ( 16.94999999999999929, 0.000000000000000000, 4.999999999999998224 ) ) ;
#61525 = CARTESIAN_POINT ( 'NONE',  ( 25.34062500061451573, -3.027376345333614438, 5.243569643749998122 ) ) ;
#61526 = CARTESIAN_POINT ( 'NONE',  ( -2.000000000000000000, 18.12500000000000355, 26.53589838486224650 ) ) ;
#61527 = CARTESIAN_POINT ( 'NONE',  ( 14.89687500061451786, 5.492252693125287522, 3.363034840372157021E-16 ) ) ;
#61528 = CARTESIAN_POINT ( 'NONE',  ( 2.953125000614516438, -4.541064518000417216, -2.621784821875001281 ) ) ;
#61529 = CARTESIAN_POINT ( 'NONE',  ( 20.14687500061451786, -3.027376345333610441, -5.243569643749999898 ) ) ;
#61530 = CARTESIAN_POINT ( 'NONE',  ( 9.001249775931846008E-16, 13.67187500061451999, 34.90005215228797653 ) ) ;
#61531 = CARTESIAN_POINT ( 'NONE',  ( 22.62187500061451573, 3.027376345333611329, 5.243569643749999010 ) ) ;
#61532 = CARTESIAN_POINT ( 'NONE',  ( 28.95937500061451431, 0.000000000000000000, 5.243569643749999010 ) ) ;
#61533 = CARTESIAN_POINT ( 'NONE',  ( -4.243569643749998122, 18.54687500061451644, 32.45002607614398471 ) ) ;
#61534 = CARTESIAN_POINT ( 'NONE',  ( 10.45312500061451644, 0.000000000000000000, 5.243569643749999010 ) ) ;
#61535 = DIRECTION ( 'NONE',  ( -0.000000000000000000, -0.000000000000000000, -1.000000000000000000 ) ) ;
#61536 = CARTESIAN_POINT ( 'NONE',  ( 6.159375000614517148, -4.541064518000417216, -2.621784821875001281 ) ) ;
#61537 = CARTESIAN_POINT ( 'NONE',  ( 12.90000000000000213, 0.000000000000000000, 4.999999999999998224 ) ) ;
#61538 = CARTESIAN_POINT ( 'NONE',  ( 7.228125000614517681, 4.541064518000418104, 2.621784821874999949 ) ) ;
#61539 = CARTESIAN_POINT ( 'NONE',  ( 11.55937500061451928, -4.541064518000417216, -2.621784821875001281 ) ) ;
#61540 = CARTESIAN_POINT ( 'NONE',  ( 19.08750000122903145, 6.123233995736764310E-16, -4.999999999999998224 ) ) ;
#61541 = CARTESIAN_POINT ( 'NONE',  ( 7.471875000614519813, -6.054752690667223547, -1.112240025338166033E-15 ) ) ;
#61542 = CARTESIAN_POINT ( 'NONE',  ( 9.478125000614515017, 4.541064518000418104, 2.621784821874999949 ) ) ;
#61543 = CARTESIAN_POINT ( 'NONE',  ( 45.00000000000000000, 6.363961030679004871, 6.363961030678849440 ) ) ;
#61544 = CARTESIAN_POINT ( 'NONE',  ( 24.84375000122903288, -2.886751345948125991, -5.000000000000000000 ) ) ;
#61545 = CARTESIAN_POINT ( 'NONE',  ( 18.64687500061451786, -3.027376345333614438, 5.243569643749998122 ) ) ;
#61546 = CARTESIAN_POINT ( 'NONE',  ( 1.999999999999998668, 13.21250000122903501, 26.53589838486224650 ) ) ;
#61547 = CARTESIAN_POINT ( 'NONE',  ( 28.11562500061451431, -6.054752690667223547, -1.112240025338166033E-15 ) ) ;
#61548 = CARTESIAN_POINT ( 'NONE',  ( 11.31562500061451892, 3.027376345333611329, 5.243569643749999010 ) ) ;
#61549 = CARTESIAN_POINT ( 'NONE',  ( 28.77187500061451431, 3.027376345333612662, -5.243569643749998122 ) ) ;
#61550 = CARTESIAN_POINT ( 'NONE',  ( -3.000416591977282496E-16, 12.99687500061451750, -34.90005215228797653 ) ) ;
#61551 = CARTESIAN_POINT ( 'NONE',  ( 13.80000000122903181, 5.773502691896255534, 3.535250795749688894E-16 ) ) ;
#61552 = CARTESIAN_POINT ( 'NONE',  ( 26.91562500061451146, 3.027376345333613106, -5.243569643749998122 ) ) ;
#61553 = CARTESIAN_POINT ( 'NONE',  ( -4.243569643749997233, 15.79062500061451857, -27.54997392385601174 ) ) ;
#61554 = CARTESIAN_POINT ( 'NONE',  ( 15.52500000122903323, 2.886751345948129099, -4.999999999999998224 ) ) ;
#61555 = CARTESIAN_POINT ( 'NONE',  ( 12.86250000000000071, 2.886751345948126879, 4.999999999999999112 ) ) ;
#61556 = DIRECTION ( 'NONE',  ( -1.000000000000000000, -0.000000000000000000, -0.000000000000000000 ) ) ;
#61557 = CARTESIAN_POINT ( 'NONE',  ( 23.69062500061451004, -3.027376345333610441, -5.243569643749999898 ) ) ;
#61558 = CARTESIAN_POINT ( 'NONE',  ( 7.134375000614516793, 6.421520780324663323E-16, -5.243569643749999010 ) ) ;
#61559 = CARTESIAN_POINT ( 'NONE',  ( 9.787500001229036073, 4.330127018922191873, 2.499999999999999556 ) ) ;
#61560 = CARTESIAN_POINT ( 'NONE',  ( 18.82500000122903216, 2.886751345948126879, 4.999999999999999112 ) ) ;
#61561 = CARTESIAN_POINT ( 'NONE',  ( 15.92812500061451608, -4.541064518000419881, 2.621784821874995952 ) ) ;
#61562 = CARTESIAN_POINT ( 'NONE',  ( 17.57812500061451644, 4.541064518000418104, 2.621784821874999949 ) ) ;
#61563 = CARTESIAN_POINT ( 'NONE',  ( 26.47500000122903074, 2.886751345948126879, 4.999999999999999112 ) ) ;
#61564 = CARTESIAN_POINT ( 'NONE',  ( 27.97500000122903074, -5.773502691896255534, -1.060575238724906372E-15 ) ) ;
#61565 = CARTESIAN_POINT ( 'NONE',  ( 22.72499999999999787, 4.330127018922191873, 2.499999999999999556 ) ) ;
#61566 = CARTESIAN_POINT ( 'NONE',  ( 25.28437500061451715, 4.541064518000418104, 2.621784821874999949 ) ) ;
#61567 = CARTESIAN_POINT ( 'NONE',  ( 25.68750000122903288, -4.330127018922194537, 2.499999999999995559 ) ) ;
#61568 = CARTESIAN_POINT ( 'NONE',  ( 12.90000000122903145, 5.773502691896255534, 3.535250795749688894E-16 ) ) ;
#61569 = CARTESIAN_POINT ( 'NONE',  ( 27.08437500061451786, 4.541064518000418104, 2.621784821874999949 ) ) ;
#61570 = B_SPLINE_CURVE_WITH_KNOTS ( 'NONE', 3,
 ( #67271, #10737, #27011, #21083, #11099, #49181, #56171, #43634, #33270, #43271, #66157, #15534, #38078, #60600, #10009, #32544, #15903, #55808, #5565, #50630, #55082, #4838, #49543, #38450, #50276, #20712, #72065, #60976, #21445, #27372, #70059, #35347, #5919, #45451, #64144, #30541, #30175, #22893, #50988, #52706, #67984, #2112, #46810, #24986, #13531, #58232 ),
 .UNSPECIFIED., .F., .F.,
 ( 4, 2, 2, 2, 2, 2, 2, 2, 2, 2, 2, 2, 2, 2, 2, 2, 2, 2, 2, 2, 2, 2, 4 ),
 ( 0.01924954336552996831, 0.02045024950336954070, 0.02105060257228932863, 0.02165095564120911656, 0.02225130871012890449, 0.02285166177904869589, 0.02405236791688826481, 0.02525307405472783373, 0.02645378019256739918, 0.02705413326148718711, 0.02765448633040697157, 0.02825483939932675603, 0.02885519246824654049, 0.03005589860608610941, 0.03125660474392567834, 0.03245731088176524726, 0.03365801701960481618, 0.03485872315744438510, 0.03545907622636416956, 0.03605942929528395402, 0.03726013543312352294, 0.03786048850204330740, 0.03846084157096309186 ),
 .UNSPECIFIED. ) ;
#61571 = LINE ( 'NONE', #68852, #36123 ) ;
#61572 = CARTESIAN_POINT ( 'NONE',  ( 3.946875000614517681, -3.027376345333610441, -5.243569643749999898 ) ) ;
#61573 = CARTESIAN_POINT ( 'NONE',  ( 23.27812500061451573, 6.421520780324663323E-16, -5.243569643749999010 ) ) ;
#61574 = CARTESIAN_POINT ( 'NONE',  ( 1.878215178124997609, 13.57812499938548356, 33.25316411605952993 ) ) ;
#61575 = CARTESIAN_POINT ( 'NONE',  ( 26.23125000122903216, 6.123233995736764310E-16, -4.999999999999998224 ) ) ;
#61576 = CARTESIAN_POINT ( 'NONE',  ( 9.309375000614517504, -4.541064518000417216, -2.621784821875001281 ) ) ;
#61577 = CARTESIAN_POINT ( 'NONE',  ( 4.528125000614516615, 4.541064518000418104, 2.621784821874999949 ) ) ;
#61578 = CARTESIAN_POINT ( 'NONE',  ( 29.35312500061451502, 0.000000000000000000, 5.243569643749999010 ) ) ;
#61579 = CARTESIAN_POINT ( 'NONE',  ( 7.171875000614517326, 3.027376345333613106, -5.243569643749998122 ) ) ;
#61580 = CARTESIAN_POINT ( 'NONE',  ( 29.52187500061451431, -6.054752690667223547, -1.112240025338166033E-15 ) ) ;
#61581 = CARTESIAN_POINT ( 'NONE',  ( 30.00000000000000000, 0.000000000000000000, 0.000000000000000000 ) ) ;
#61582 = CARTESIAN_POINT ( 'NONE',  ( 19.98749999999999716, 5.773502691896255534, 3.535250795749688894E-16 ) ) ;
#61583 = ORIENTED_EDGE ( 'NONE', *, *, #15786, .T. ) ;
#61584 = CARTESIAN_POINT ( 'NONE',  ( 26.55000000000000071, -4.330127018922190985, -2.500000000000001332 ) ) ;
#61585 =( BOUNDED_CURVE ( )  B_SPLINE_CURVE ( 2, ( #34130, #17849, #11612, #5708, #23762, #1257, #56318 ),
 .UNSPECIFIED., .F., .F. ) 
 B_SPLINE_CURVE_WITH_KNOTS ( ( 3, 2, 2, 3 ),
 ( 0.04166666666666671293, 0.04444444444444448777, 0.04722222222222225568, 0.05000000000000003053 ),
 .UNSPECIFIED. ) 
 CURVE ( )  GEOMETRIC_REPRESENTATION_ITEM ( )  RATIONAL_B_SPLINE_CURVE ( ( 0.9999999999999976685, 0.8660254037844410391, 1.000000000000000000, 0.8660254037844387076, 1.000000000000000000, 0.8660254037844373753, 1.000000000000001332 ) ) 
 REPRESENTATION_ITEM ( '' )  );
#61586 = CARTESIAN_POINT ( 'NONE',  ( 27.87187500061451573, 3.027376345333613106, -5.243569643749998122 ) ) ;
#61587 = EDGE_CURVE ( 'NONE', #14259, #11117, #33949, .T. ) ;
#61588 = ORIENTED_EDGE ( 'NONE', *, *, #22231, .T. ) ;
#61589 = VECTOR ( 'NONE', #36794, 1000.000000000000000 ) ;
#61590 = CARTESIAN_POINT ( 'NONE',  ( 17.05312500061451786, 4.541064518000418104, -2.621784821874998173 ) ) ;
#61591 = CARTESIAN_POINT ( 'NONE',  ( 8.765625000614518214, -6.054752690667223547, -1.112240025338166033E-15 ) ) ;
#61592 = CARTESIAN_POINT ( 'NONE',  ( 21.53437500061451360, 5.492252693125287522, 3.363034840372157021E-16 ) ) ;
#61593 = CARTESIAN_POINT ( 'NONE',  ( 3.871875000614519280, -6.054752690667223547, -1.112240025338166033E-15 ) ) ;
#61594 = CARTESIAN_POINT ( 'NONE',  ( 18.48750000122903359, -4.330127018922194537, 2.499999999999995559 ) ) ;
#61595 = CARTESIAN_POINT ( 'NONE',  ( 24.22500000000000142, -4.330127018922194537, 2.499999999999995559 ) ) ;
#61596 = CARTESIAN_POINT ( 'NONE',  ( 3.242103837493086330E-14, 11.00000000122903288, 26.00000000000000711 ) ) ;
#61597 = CARTESIAN_POINT ( 'NONE',  ( 8.109375000614518214, 4.541064518000418104, -2.621784821874998173 ) ) ;
#61598 = CARTESIAN_POINT ( 'NONE',  ( 11.70937500061451608, 4.541064518000418104, -2.621784821874998173 ) ) ;
#61599 = CARTESIAN_POINT ( 'NONE',  ( 22.88437500061451857, 6.421520780324663323E-16, -5.243569643749999010 ) ) ;
#61600 = CARTESIAN_POINT ( 'NONE',  ( -1.487416814333745711E-14, 15.72500000122903430, -26.00000000000000000 ) ) ;
#61601 = ORIENTED_EDGE ( 'NONE', *, *, #38095, .T. ) ;
#61602 = CARTESIAN_POINT ( 'NONE',  ( 3.646875000614520079, 6.054752690667223547, 3.707466751127219781E-16 ) ) ;
#61603 = CARTESIAN_POINT ( 'NONE',  ( 11.70000000000000284, -4.330127018922190985, -2.500000000000001332 ) ) ;
#61604 = CARTESIAN_POINT ( 'NONE',  ( 7.846875000614518036, -3.027376345333614438, 5.243569643749998122 ) ) ;
#61605 = CARTESIAN_POINT ( 'NONE',  ( 3.756430356249998770, 14.40312499938548463, 32.16877607737302469 ) ) ;
#61606 = CARTESIAN_POINT ( 'NONE',  ( 21.93750000000000000, -2.886751345948129988, 4.999999999999997335 ) ) ;
#61607 = CARTESIAN_POINT ( 'NONE',  ( 16.00312500061451715, -4.541064518000417216, -2.621784821875001281 ) ) ;
#61608 = CARTESIAN_POINT ( 'NONE',  ( 3.999999999999998668, 17.41250000000000142, 32.30940107675850470 ) ) ;
#61609 = CARTESIAN_POINT ( 'NONE',  ( 4.311958327294343363, 2.531208285321026263, 4.311958327294242999 ) ) ;
#61610 = CARTESIAN_POINT ( 'NONE',  ( 23.48437500061451644, 4.119189519843966529, 2.378215178124999607 ) ) ;
#61611 = CARTESIAN_POINT ( 'NONE',  ( 10.82812500061451644, 4.541064518000418104, 2.621784821874999949 ) ) ;
#61612 = CARTESIAN_POINT ( 'NONE',  ( 29.18437500061451573, 6.421520780324663323E-16, -5.243569643749999010 ) ) ;
#61613 = CARTESIAN_POINT ( 'NONE',  ( 29.40937500061451715, 0.000000000000000000, 5.243569643749999010 ) ) ;
#61614 = CARTESIAN_POINT ( 'NONE',  ( 10.76250000000000107, -5.773502691896255534, -1.060575238724906372E-15 ) ) ;
#61615 = CARTESIAN_POINT ( 'NONE',  ( -1.999999999999997113, 14.78750000122903252, 33.46410161513775705 ) ) ;
#61616 = CARTESIAN_POINT ( 'NONE',  ( 9.900000001229033231, -2.886751345948129988, 4.999999999999997335 ) ) ;
#61617 = CARTESIAN_POINT ( 'NONE',  ( 20.37187500061451573, 3.027376345333611329, 5.243569643749999010 ) ) ;
#61618 = CARTESIAN_POINT ( 'NONE',  ( 15.30937500061451750, 4.541064518000418104, -2.621784821874998173 ) ) ;
#61619 = ORIENTED_EDGE ( 'NONE', *, *, #66024, .F. ) ;
#61620 = CARTESIAN_POINT ( 'NONE',  ( 14.61562500061451608, -6.054752690667223547, -1.112240025338166033E-15 ) ) ;
#61621 = CARTESIAN_POINT ( 'NONE',  ( 26.62500000122903288, -5.773502691896255534, -1.060575238724906372E-15 ) ) ;
#61622 = CARTESIAN_POINT ( 'NONE',  ( 14.63437500061451679, -4.541064518000419881, 2.621784821874995952 ) ) ;
#61623 = CARTESIAN_POINT ( 'NONE',  ( 5.989600911063007516, 8.007829439449656306, -29.59314995572118434 ) ) ;
#61624 = CARTESIAN_POINT ( 'NONE',  ( 16.07812500061451289, 6.421520780324663323E-16, -5.243569643749999010 ) ) ;
#61625 = CARTESIAN_POINT ( 'NONE',  ( -3.137519842735245283E-14, 14.37500000122903288, -26.00000000000000711 ) ) ;
#61626 = CARTESIAN_POINT ( 'NONE',  ( 27.45937500061451786, 4.541064518000418104, -2.621784821874998173 ) ) ;
#61627 = CARTESIAN_POINT ( 'NONE',  ( 2.121784821875001281, 10.50312500061451715, 33.67503911421598417 ) ) ;
#61628 = CARTESIAN_POINT ( 'NONE',  ( 16.09687500061452070, -3.027376345333610441, -5.243569643749999898 ) ) ;
#61629 = CARTESIAN_POINT ( 'NONE',  ( 14.88750000122903394, -4.330127018922194537, 2.499999999999995559 ) ) ;
#61630 = FACE_OUTER_BOUND ( 'NONE', #18438, .T. ) ;
#61631 = CARTESIAN_POINT ( 'NONE',  ( 2.121784821874999061, 18.80937500061451928, -33.67503911421598417 ) ) ;
#61632 = CARTESIAN_POINT ( 'NONE',  ( 19.39687500061451786, 6.054752690667223547, 3.707466751127219781E-16 ) ) ;
#61633 = CARTESIAN_POINT ( 'NONE',  ( 18.90000000122902790, -2.886751345948129988, 4.999999999999997335 ) ) ;
#61634 = CARTESIAN_POINT ( 'NONE',  ( 17.25937500061451502, 0.000000000000000000, 5.243569643749999010 ) ) ;
#61635 = CARTESIAN_POINT ( 'NONE',  ( 2.121784821875001281, 13.25937500061451857, 33.67503911421598417 ) ) ;
#61636 = CARTESIAN_POINT ( 'NONE',  ( 16.94062500061451715, -3.027376345333610441, -5.243569643749999898 ) ) ;
#61637 = ORIENTED_EDGE ( 'NONE', *, *, #53941, .T. ) ;
#61638 = ORIENTED_EDGE ( 'NONE', *, *, #31768, .F. ) ;
#61639 = CARTESIAN_POINT ( 'NONE',  ( 19.94999999999999929, 4.330127018922192761, -2.499999999999997780 ) ) ;
#61640 = DIRECTION ( 'NONE',  ( -1.000000000000000000, -0.000000000000000000, -0.000000000000000000 ) ) ;
#61641 = CARTESIAN_POINT ( 'NONE',  ( 23.35312500061451857, 4.541064518000418104, -2.621784821874998173 ) ) ;
#61642 = CARTESIAN_POINT ( 'NONE',  ( 3.215625000614518836, 3.027376345333611329, 5.243569643749999010 ) ) ;
#61643 = CARTESIAN_POINT ( 'NONE',  ( 17.36250000122903359, 4.330127018922192761, -2.499999999999997780 ) ) ;
#61644 = CARTESIAN_POINT ( 'NONE',  ( 22.37812500061451360, 6.421520780324663323E-16, -5.243569643749999010 ) ) ;
#61645 = CARTESIAN_POINT ( 'NONE',  ( 25.97812500061451502, 6.421520780324663323E-16, -5.243569643749999010 ) ) ;
#61646 = CARTESIAN_POINT ( 'NONE',  ( 5.240625000614516971, -3.027376345333610441, -5.243569643749999898 ) ) ;
#61647 = ORIENTED_EDGE ( 'NONE', *, *, #27131, .F. ) ;
#61648 = EDGE_CURVE ( 'NONE', #19531, #30832, #62034, .T. ) ;
#61649 = AXIS2_PLACEMENT_3D ( 'NONE', #17155, #39347, #28257 ) ;
#61650 = CARTESIAN_POINT ( 'NONE',  ( -1.071796769724492115, 20.41115380933863221, 34.00000000000000000 ) ) ;
#61651 = CARTESIAN_POINT ( 'NONE',  ( 3.215625000614518836, 3.027376345333611329, 5.243569643749999010 ) ) ;
#61652 = EDGE_CURVE ( 'NONE', #18641, #36195, #10203, .T. ) ;
#61653 = CARTESIAN_POINT ( 'NONE',  ( 12.15937500061451892, 4.119189519843966529, -2.378215178124998275 ) ) ;
#61654 = DIRECTION ( 'NONE',  ( 1.000000000000000000, -0.000000000000000000, -0.000000000000000000 ) ) ;
#61655 = CARTESIAN_POINT ( 'NONE',  ( -3.999999999999999112, 12.46250000122903323, -30.00000000000000000 ) ) ;
#61656 = CARTESIAN_POINT ( 'NONE',  ( -4.243569643749999898, 18.95937500061451431, -30.00000000000000000 ) ) ;
#61657 = CARTESIAN_POINT ( 'NONE',  ( 9.074999999999999289, 6.123233995736764310E-16, -4.999999999999998224 ) ) ;
#61658 = ADVANCED_FACE ( 'NONE', ( #44698 ), #68238, .T. ) ;
#61659 = CARTESIAN_POINT ( 'NONE',  ( 3.562500001229033764, 0.000000000000000000, 4.999999999999998224 ) ) ;
#61660 = CARTESIAN_POINT ( 'NONE',  ( 11.93437500061451573, -4.541064518000419881, 2.621784821874995952 ) ) ;
#61661 = CARTESIAN_POINT ( 'NONE',  ( 1.592000809091587073E-14, 16.85000000122903785, -34.00000000000000000 ) ) ;
#61662 = CARTESIAN_POINT ( 'NONE',  ( 3.646875000614520079, 6.054752690667223547, 3.707466751127219781E-16 ) ) ;
#61663 = DIRECTION ( 'NONE',  ( -1.000000000000000000, -0.000000000000000000, -0.000000000000000000 ) ) ;
#61664 = FACE_OUTER_BOUND ( 'NONE', #65579, .T. ) ;
#61665 = EDGE_CURVE ( 'NONE', #72600, #68862, #72519, .T. ) ;
#61666 = CARTESIAN_POINT ( 'NONE',  ( 9.984375000614518214, 4.541064518000418104, 2.621784821874999949 ) ) ;
#61667 = CARTESIAN_POINT ( 'NONE',  ( 3.562500000000000444, -5.773502691896255534, -1.060575238724906372E-15 ) ) ;
#61668 = CARTESIAN_POINT ( 'NONE',  ( 19.52812500061451573, -4.541064518000419881, 2.621784821874995952 ) ) ;
#61669 = LINE ( 'NONE', #38795, #60474 ) ;
#61670 = CARTESIAN_POINT ( 'NONE',  ( -4.243569643749998122, 18.04062500061459673, 32.45002607614398471 ) ) ;
#61671 = CARTESIAN_POINT ( 'NONE',  ( 23.55937500061451573, 0.000000000000000000, 5.243569643749999010 ) ) ;
#61672 = CARTESIAN_POINT ( 'NONE',  ( 1.626862140677534273E-15, 15.27500000122903501, -26.00000000000000355 ) ) ;
#61673 = CARTESIAN_POINT ( 'NONE',  ( 29.13750000122903216, 4.330127018922191873, 2.499999999999999556 ) ) ;
#61674 = CARTESIAN_POINT ( 'NONE',  ( 20.14687500061451786, 4.119189519843966529, -2.378215178124998275 ) ) ;
#61675 = CARTESIAN_POINT ( 'NONE',  ( 24.02812500061451573, -4.541064518000419881, 2.621784821874995952 ) ) ;
#61676 = CARTESIAN_POINT ( 'NONE',  ( 14.50312500061451537, 0.000000000000000000, 5.243569643749999010 ) ) ;
#61677 = CARTESIAN_POINT ( 'NONE',  ( 13.66875000122903216, 2.886751345948129099, -4.999999999999998224 ) ) ;
#61678 = CARTESIAN_POINT ( 'NONE',  ( 12.94687500061451857, -3.027376345333610441, -5.243569643749999898 ) ) ;
#61679 = CARTESIAN_POINT ( 'NONE',  ( 28.87499999999999645, 6.123233995736764310E-16, -4.999999999999998224 ) ) ;
#61680 = CARTESIAN_POINT ( 'NONE',  ( 23.88750000122903216, -4.330127018922194537, 2.499999999999995559 ) ) ;
#61681 = CARTESIAN_POINT ( 'NONE',  ( 4.246875000614519280, -3.027376345333614438, 5.243569643749998122 ) ) ;
#61682 = CARTESIAN_POINT ( 'NONE',  ( 14.82187500061451679, 3.027376345333613106, -5.243569643749998122 ) ) ;
#61683 = CARTESIAN_POINT ( 'NONE',  ( 21.15000000000000213, -4.330127018922190985, -2.500000000000001332 ) ) ;
#61684 = CARTESIAN_POINT ( 'NONE',  ( -1.999999999999997113, 11.52500000000000036, 33.46410161513775705 ) ) ;
#61685 = FACE_OUTER_BOUND ( 'NONE', #36642, .T. ) ;
#61686 = CARTESIAN_POINT ( 'NONE',  ( 24.23437500061451644, 6.421520780324663323E-16, -5.243569643749999010 ) ) ;
#61687 = CARTESIAN_POINT ( 'NONE',  ( 14.03437500061451715, 4.541064518000418104, 2.621784821874999949 ) ) ;
#61688 = CARTESIAN_POINT ( 'NONE',  ( -1.878215178125001827, 16.20312499938548356, 33.25316411605952283 ) ) ;
#61689 = CARTESIAN_POINT ( 'NONE',  ( 27.97500000000000142, 6.123233995736764310E-16, -4.999999999999998224 ) ) ;
#61690 = CARTESIAN_POINT ( 'NONE',  ( 3.562500001229033764, 0.000000000000000000, 4.999999999999998224 ) ) ;
#61691 = CARTESIAN_POINT ( 'NONE',  ( 6.600000000000001421, 0.000000000000000000, 4.999999999999998224 ) ) ;
#61692 = CARTESIAN_POINT ( 'NONE',  ( 28.99687500061451573, -2.746126346562646425, 4.756430356249996549 ) ) ;
#61693 = CARTESIAN_POINT ( 'NONE',  ( 19.11562500061451431, -6.054752690667223547, -1.112240025338166033E-15 ) ) ;
#61694 = CARTESIAN_POINT ( 'NONE',  ( 8.512499999999999289, -5.773502691896255534, -1.060575238724906372E-15 ) ) ;
#61695 = CARTESIAN_POINT ( 'NONE',  ( -3.999999999999999112, 14.15000000000000036, 30.00000000000000000 ) ) ;
#61696 = CARTESIAN_POINT ( 'NONE',  ( 16.64999999999999858, -4.330127018922190985, -2.500000000000001332 ) ) ;
#61697 = CARTESIAN_POINT ( 'NONE',  ( -2.121784821874996840, 12.67812500061451786, 33.67503911421598417 ) ) ;
#61698 = CARTESIAN_POINT ( 'NONE',  ( 3.999999999999998668, 18.31250000000000000, 32.30940107675850470 ) ) ;
#61699 = CARTESIAN_POINT ( 'NONE',  ( 19.95000000122903572, -2.886751345948125991, -5.000000000000000000 ) ) ;
#61700 = CARTESIAN_POINT ( 'NONE',  ( 45.00000000000000000, 0.000000000000000000, 0.000000000000000000 ) ) ;
#61701 = CARTESIAN_POINT ( 'NONE',  ( 27.12187500061451573, 3.027376345333611329, 5.243569643749999010 ) ) ;
#61702 = ORIENTED_EDGE ( 'NONE', *, *, #4530, .F. ) ;
#61703 = CARTESIAN_POINT ( 'NONE',  ( 15.92812500061451608, -4.541064518000419881, 2.621784821874995952 ) ) ;
#61704 = CARTESIAN_POINT ( 'NONE',  ( 22.00312500061451360, 4.541064518000418104, -2.621784821874998173 ) ) ;
#61705 = CARTESIAN_POINT ( 'NONE',  ( 22.13437500061451502, 4.541064518000418104, 2.621784821874999949 ) ) ;
#61706 = CARTESIAN_POINT ( 'NONE',  ( 6.600000000000001421, 0.000000000000000000, 4.999999999999998224 ) ) ;
#61707 = CARTESIAN_POINT ( 'NONE',  ( 10.11562500061451608, -6.054752690667223547, -1.112240025338166033E-15 ) ) ;
#61708 = CARTESIAN_POINT ( 'NONE',  ( 24.89062500061451644, -3.027376345333614438, 5.243569643749998122 ) ) ;
#61709 = CARTESIAN_POINT ( 'NONE',  ( 15.12187500061451750, -6.054752690667223547, -1.112240025338166033E-15 ) ) ;
#61710 = CARTESIAN_POINT ( 'NONE',  ( 18.42187500061451644, 3.027376345333613106, -5.243569643749998122 ) ) ;
#61711 = CARTESIAN_POINT ( 'NONE',  ( 19.27500000000000213, -4.330127018922194537, 2.499999999999995559 ) ) ;
#61712 = CARTESIAN_POINT ( 'NONE',  ( 4.243569643749999010, 17.81562500061451715, 27.54997392385601174 ) ) ;
#61713 = CARTESIAN_POINT ( 'NONE',  ( 21.15000000122903145, -2.886751345948129988, 4.999999999999997335 ) ) ;
#61714 = CARTESIAN_POINT ( 'NONE',  ( 16.20937500061451786, 4.119189519843966529, -2.378215178124998275 ) ) ;
#61715 = CARTESIAN_POINT ( 'NONE',  ( 12.32812500061451821, -4.541064518000419881, 2.621784821874995952 ) ) ;
#61716 = CARTESIAN_POINT ( 'NONE',  ( 5.521875000614517859, 3.027376345333611329, 5.243569643749999010 ) ) ;
#61717 = CARTESIAN_POINT ( 'NONE',  ( 4.321875000614517681, -6.054752690667223547, -1.112240025338166033E-15 ) ) ;
#61718 = ORIENTED_EDGE ( 'NONE', *, *, #41944, .F. ) ;
#61719 = CARTESIAN_POINT ( 'NONE',  ( 27.08437500061451786, 4.541064518000418104, 2.621784821874999949 ) ) ;
#61720 = CARTESIAN_POINT ( 'NONE',  ( 18.21562500061451573, -6.054752690667223547, -1.112240025338166033E-15 ) ) ;
#61721 = CARTESIAN_POINT ( 'NONE',  ( 27.90000000122903145, -2.886751345948129988, 4.999999999999997335 ) ) ;
#61722 = CARTESIAN_POINT ( 'NONE',  ( 27.10312500061451502, 0.000000000000000000, 5.243569643749999010 ) ) ;
#61723 = CARTESIAN_POINT ( 'NONE',  ( 25.24687500061451573, 6.054752690667223547, 3.707466751127219781E-16 ) ) ;
#61724 = CARTESIAN_POINT ( 'NONE',  ( 20.31562500061451715, 3.027376345333611329, 5.243569643749999010 ) ) ;
#61725 = CARTESIAN_POINT ( 'NONE',  ( 2.121784821874999061, 18.35937500061451644, 26.32496088578401583 ) ) ;
#61726 = CARTESIAN_POINT ( 'NONE',  ( 25.11562500061451431, 3.027376345333613106, -5.243569643749998122 ) ) ;
#61727 = CARTESIAN_POINT ( 'NONE',  ( 4.500000001229034652, -2.886751345948129988, 4.999999999999997335 ) ) ;
#61728 = ORIENTED_EDGE ( 'NONE', *, *, #69660, .F. ) ;
#61729 = CARTESIAN_POINT ( 'NONE',  ( 26.88749999999999574, -2.886751345948129988, 4.999999999999997335 ) ) ;
#61730 = CARTESIAN_POINT ( 'NONE',  ( -1.999999999999997113, 14.67500000000000071, -26.53589838486224295 ) ) ;
#61731 = CARTESIAN_POINT ( 'NONE',  ( 1.878215178125000495, 16.42812499938548143, 26.74683588394047007 ) ) ;
#61732 = CARTESIAN_POINT ( 'NONE',  ( 4.771875000614516971, -6.054752690667223547, -1.112240025338166033E-15 ) ) ;
#61733 = CARTESIAN_POINT ( 'NONE',  ( 13.79062500061451502, -3.027376345333610441, -5.243569643749999898 ) ) ;
#61734 = CARTESIAN_POINT ( 'NONE',  ( 6.721875000614518925, 3.027376345333613106, -5.243569643749998122 ) ) ;
#61735 = CARTESIAN_POINT ( 'NONE',  ( 24.78750000122903074, -4.330127018922194537, 2.499999999999995559 ) ) ;
#61736 = CARTESIAN_POINT ( 'NONE',  ( 15.12187500061451928, -6.054752690667223547, -1.112240025338166033E-15 ) ) ;
#61737 = CARTESIAN_POINT ( 'NONE',  ( 3.421875000614516882, -6.054752690667223547, -1.112240025338166033E-15 ) ) ;
#61738 = CARTESIAN_POINT ( 'NONE',  ( 27.93750000000000000, -2.886751345948125991, -5.000000000000000000 ) ) ;
#61739 = CARTESIAN_POINT ( 'NONE',  ( 26.33437500061451431, -4.541064518000419881, 2.621784821874995952 ) ) ;
#61740 = CARTESIAN_POINT ( 'NONE',  ( 3.140625000614516882, 6.054752690667223547, 3.707466751127219781E-16 ) ) ;
#61741 = CARTESIAN_POINT ( 'NONE',  ( 13.90312500061451750, 4.541064518000418104, -2.621784821874998173 ) ) ;
#61742 = VERTEX_POINT ( 'NONE', #38968 ) ;
#61743 = CARTESIAN_POINT ( 'NONE',  ( 9.215625000614515727, -6.054752690667223547, -1.112240025338166033E-15 ) ) ;
#61744 = CARTESIAN_POINT ( 'NONE',  ( 6.365625000614518747, 3.027376345333611329, 5.243569643749999010 ) ) ;
#61745 = CARTESIAN_POINT ( 'NONE',  ( 19.43437500061451928, 4.119189519843966529, 2.378215178124999607 ) ) ;
#61746 = CARTESIAN_POINT ( 'NONE',  ( -0.7368805616696194605, 9.859898480082234684, 25.82089837893477480 ) ) ;
#61747 = CARTESIAN_POINT ( 'NONE',  ( 15.03749999999999964, 5.773502691896255534, 3.535250795749688894E-16 ) ) ;
#61748 =( BOUNDED_CURVE ( )  B_SPLINE_CURVE ( 2, ( #19724, #42275, #48185, #30462, #64798, #2388, #53726, #53353, #2751 ),
 .UNSPECIFIED., .F., .F. ) 
 B_SPLINE_CURVE_WITH_KNOTS ( ( 3, 2, 2, 2, 3 ),
 ( 0.2916666666666666852, 0.2962962962962962798, 0.3055555555555555802, 0.3148148148148148251, 0.3194444444444444753 ),
 .UNSPECIFIED. ) 
 CURVE ( )  GEOMETRIC_REPRESENTATION_ITEM ( )  RATIONAL_B_SPLINE_CURVE ( ( 0.9330127018922194093, 0.9330127018922197424, 1.000000000000000000, 0.8660254037844387076, 1.000000000000000000, 0.8660254037844387076, 1.000000000000000000, 0.9330127018922189652, 0.9330127018922194093 ) ) 
 REPRESENTATION_ITEM ( '' )  );
#61749 = EDGE_CURVE ( 'NONE', #29431, #25241, #32415, .T. ) ;
#61750 = CARTESIAN_POINT ( 'NONE',  ( 14.97187500061451892, 3.027376345333611329, 5.243569643749999010 ) ) ;
#61751 = CARTESIAN_POINT ( 'NONE',  ( 12.56250000122903465, 0.000000000000000000, 4.999999999999998224 ) ) ;
#61752 = CARTESIAN_POINT ( 'NONE',  ( 19.01249999999999929, 2.886751345948129099, -4.999999999999998224 ) ) ;
#61753 = CARTESIAN_POINT ( 'NONE',  ( 21.83437500061451786, -4.541064518000419881, 2.621784821874995952 ) ) ;
#61754 = CARTESIAN_POINT ( 'NONE',  ( 4.243569643749999898, 13.27812500061451750, -30.00000000000000000 ) ) ;
#61755 = CARTESIAN_POINT ( 'NONE',  ( 3.065815551951259543, -3.949781639713015657, 3.065815551951216467 ) ) ;
#61756 = CARTESIAN_POINT ( 'NONE',  ( 24.90937500061451360, -5.492252693125287522, -1.008910452111647106E-15 ) ) ;
#61757 = FACE_OUTER_BOUND ( 'NONE', #64025, .T. ) ;
#61758 = CARTESIAN_POINT ( 'NONE',  ( 25.75312500061451715, 0.000000000000000000, 5.243569643749999010 ) ) ;
#61759 = PRESENTATION_STYLE_ASSIGNMENT (( #57661 ) ) ;
#61760 = DIRECTION ( 'NONE',  ( 1.000000000000000000, -0.000000000000000000, -0.000000000000000000 ) ) ;
#61761 = CARTESIAN_POINT ( 'NONE',  ( 25.53750000000000142, -2.886751345948129988, 4.999999999999997335 ) ) ;
#61762 = CARTESIAN_POINT ( 'NONE',  ( 8.803125000614517859, -4.541064518000417216, -2.621784821875001281 ) ) ;
#61763 = CARTESIAN_POINT ( 'NONE',  ( 26.29687500061451644, -4.119189519843965641, -2.378215178125001383 ) ) ;
#61764 = CARTESIAN_POINT ( 'NONE',  ( 20.52187500061451786, -6.054752690667223547, -1.112240025338166033E-15 ) ) ;
#61765 = CARTESIAN_POINT ( 'NONE',  ( 13.69687500061451679, -4.119189519843965641, -2.378215178125001383 ) ) ;
#61766 = CARTESIAN_POINT ( 'NONE',  ( 5.653125000614517504, -4.541064518000417216, -2.621784821875001281 ) ) ;
#61767 = CARTESIAN_POINT ( 'NONE',  ( 10.39687500061451786, 6.054752690667223547, 3.707466751127219781E-16 ) ) ;
#61768 = ORIENTED_EDGE ( 'NONE', *, *, #53711, .T. ) ;
#61769 = CARTESIAN_POINT ( 'NONE',  ( 20.59687500061451360, -3.027376345333610441, -5.243569643749999898 ) ) ;
#61770 = CARTESIAN_POINT ( 'NONE',  ( 0.000000000000000000, 20.00000000000000000, 30.00000000000000000 ) ) ;
#61771 = CARTESIAN_POINT ( 'NONE',  ( 29.43750000000000000, 5.773502691896255534, 3.535250795749688894E-16 ) ) ;
#61773 = ADVANCED_FACE ( 'NONE', ( #11250 ), #56316, .F. ) ;
#61772 = CARTESIAN_POINT ( 'NONE',  ( 6.075000000000000178, 4.330127018922191873, 2.499999999999999556 ) ) ;
#61774 = CARTESIAN_POINT ( 'NONE',  ( 15.56250000122903465, 4.330127018922192761, -2.499999999999997780 ) ) ;
#61775 = CARTESIAN_POINT ( 'NONE',  ( 0.000000000000000000, 27.50000000000000000, 30.00000000000000000 ) ) ;
#61776 = EDGE_LOOP ( 'NONE', ( #36781, #35105, #64546, #38106 ) ) ;
#61777 = CARTESIAN_POINT ( 'NONE',  ( 12.33750000000000036, 5.773502691896255534, 3.535250795749688894E-16 ) ) ;
#61778 = CARTESIAN_POINT ( 'NONE',  ( 25.94062500061451715, -3.027376345333610441, -5.243569643749999898 ) ) ;
#61779 = CARTESIAN_POINT ( 'NONE',  ( 17.36249999999999716, 2.886751345948126879, 4.999999999999999112 ) ) ;
#61780 = CARTESIAN_POINT ( 'NONE',  ( 11.62500000122903465, 2.886751345948126879, 4.999999999999999112 ) ) ;
#61781 = CARTESIAN_POINT ( 'NONE',  ( 9.853125000614516793, 4.541064518000418104, -2.621784821874998173 ) ) ;
#61782 = CARTESIAN_POINT ( 'NONE',  ( 7.912499999999999645, 2.886751345948126879, 4.999999999999999112 ) ) ;
#61783 = DIRECTION ( 'NONE',  ( 0.000000000000000000, 0.000000000000000000, 1.000000000000000000 ) ) ;
#61784 = CARTESIAN_POINT ( 'NONE',  ( -2.121784821874996840, 15.43437500061451928, -26.32496088578401583 ) ) ;
#61785 = CARTESIAN_POINT ( 'NONE',  ( 27.60000000122903430, -2.886751345948125991, -5.000000000000000000 ) ) ;
#61786 = CARTESIAN_POINT ( 'NONE',  ( 3.756430356250000546, 14.47812499938548747, 27.83122392262697886 ) ) ;
#61787 = CARTESIAN_POINT ( 'NONE',  ( 7.387500000000001066, 5.773502691896255534, 3.535250795749688894E-16 ) ) ;
#61788 = CARTESIAN_POINT ( 'NONE',  ( -5.810221930991193690E-16, 12.68750000000000000, 26.00000000000000355 ) ) ;
#61789 = VERTEX_POINT ( 'NONE', #45232 ) ;
#61790 = CARTESIAN_POINT ( 'NONE',  ( 24.51562500061451289, -6.054752690667223547, -1.112240025338166033E-15 ) ) ;
#61791 = CARTESIAN_POINT ( 'NONE',  ( 29.80312500061451431, 0.000000000000000000, 5.243569643749999010 ) ) ;
#61792 = CARTESIAN_POINT ( 'NONE',  ( 28.77187500061451431, 3.027376345333613106, -5.243569643749998122 ) ) ;
#61793 = CARTESIAN_POINT ( 'NONE',  ( 19.84687500061451360, 6.054752690667223547, 3.707466751127219781E-16 ) ) ;
#61794 = CARTESIAN_POINT ( 'NONE',  ( 17.69062500061451715, -3.027376345333614438, 5.243569643749998122 ) ) ;
#61795 = ADVANCED_FACE ( 'NONE', ( #67764 ), #6064, .F. ) ;
#61796 = CARTESIAN_POINT ( 'NONE',  ( 4.243569643749999898, 11.44062500061459353, -27.54997392385601529 ) ) ;
#61797 = CARTESIAN_POINT ( 'NONE',  ( 6.253125000614517148, 4.541064518000418104, -2.621784821874998173 ) ) ;
#61798 =( BOUNDED_SURFACE ( )  B_SPLINE_SURFACE ( 1, 2, ( 
 ( #6719, #44808, #33699, #62142, #56246, #22254, #67341, #39259, #16701, #61413, #824, #5637, #29252, #72500, #33342, #61771, #57315, #51423, #22609, #11536, #6352, #16340, #28522, #28174, #23332, #11175, #22966, #44446, #38895, #27813, #50347, #45882, #34056, #45527, #21888, #68414, #72871, #10807, #50701, #55880, #56596, #17776, #103, #68057, #45161, #67692, #5992, #40335, #12251, #39985, #62497, #11895, #62857, #34420, #56948, #34782, #28883, #41070, #7438, #52144, #52867, #63584, #35866, #35150, #13327, #8529, #46603, #1547, #7802, #2266, #30339, #58389, #47684, #18136, #1184, #24781, #57673, #69146, #52505, #69505, #12616, #29608, #7079, #47325, #35509, #63942, #18865, #24420, #36241, #12971, #30694, #42150, #64677, #69858, #41426, #24057, #1916, #18505, #58755, #25143, #58028, #46969, #46240, #8165, #23692, #29964, #19225, #41779, #53225, #64308, #13698, #51784, #59122, #2622, #70220, #19594, #14062, #36601, #68780, #40703, #63221, #19963, #33516, #14795, #61962, #31058, #65040, #20328, #16887, #10996, #54338, #71322, #38062, #25518, #60218, #37338, #56066, #48431, #32164, #2990, #70588, #59488, #25891, #5458, #70956, #59861, #42882, #20697, #65405, #9265, #53972, #48063, #73055, #48793, #61595, #27998, #50527, #31800, #43255, #49166, #4101, #31432, #3732, #22437, #54697, #26257, #3370, #44985, #42516, #67522, #36966, #26629, #53595, #14431, #8900, #65776, #15158, #37695, #9630, #71697, #21069, #39441, #43620, #66142, #15520, #22793, #68969, #29795, #45346, #62688, #18326, #45712, #69332, #33883, #18690, #62328, #285, #28348, #56428, #46795, #67880, #17252, #39812, #5817, #17609, #12444, #57135, #35334, #1373, #68605, #11724, #50885, #34240, #56774, #6179, #28708, #40169, #51247, #1014, #23883, #650, #41254, #63043, #12084, #68246, #11365, #23158, #34605, #6544, #23520, #7266, #29078, #51613, #1733, #46070, #17966, #40899, #46430, #63412, #40527, #29437, #52331, #34975, #57504, #24247, #6906, #51974, #12798, #57857, #30158, #69687, #8718, #3187, #53423, #13890, #9088, #35696, #65227, #2097, #36430, #59307, #2813, #24608, #13154, #64129, #58216, #25714, #31250, #7621, #20151, #19791, #14616, #70775, #53792, #48252, #31625, #19052, #52691, #54159, #37155, #41610, #42705, #58583, #47515, #36063, #13515, #47155, #7990, #30526, #26077, #53053, #2447, #24970, #70044, #19417, #64865, #58944, #59681, #3555, #47887, #41977, #64498, #8352, #30881, #25341, #70415, #42342, #14253, #36792, #48616, #71141, #20514, #63766, #43808, #26818, #50448, #37524, #5375, #26446, #32720, #38997, #71516, #37888, #33436, #60407, #55257, #72610, #33079, #21992, #49352, #61155, #61512, #48986, #16083, #10910, #60045, #15347, #71882, #27547, #9456, #20891, #10550, #55617, #4653, #66333, #55981, #14986, #44550, #54520, #15711, #38631, #27182, #3923, #65598, #43445, #31986, #5013, #50079, #65967, #67081, #72244, #16440, #27913, #72973, #43072, #9816, #32348, #54886, #4293, #21255, #38249, #60778, #10185, #49716, #21621, #44179, #66709, #40441, #68520, #22711, #11644, #1285, #45984, #28627, #45264, #23795, #61877, #46346, #28272, #17881, #44907, #11284, #56348, #17170, #16806, #67796, #39730, #68164, #62957, #68880, #35250, #33805, #23438, #5738, #6820, #40810, #50803, #568, #29354, #56696, #7181, #67444, #29709, #51165, #62247, #18237, #206, #63326, #34159, #12352, #39362, #6096, #23074, #45631, #17527, #40089, #62603, #11999, #34887, #12714, #57771, #34522, #57416, #57052, #51887, #52247, #6458, #28993, #22355, #51530, #930, #8631, #46711, #7536, #47069, #64776, #31160, #7902, #36344, #31535, #9003, #69604, #35973, #19329, #58493, #24525, #18965, #41525, #64044, #63681, #3095, #30440, #1650, #24158, #35610, #13423, #59590, #53702, #24883, #41884, #25624, #69246, #30799, #52969, #48161, #2365, #2730, #18607, #41172, #30069, #47428, #70686, #69959, #64412, #13805, #58859, #8269, #53332, #25245, #13071, #42617, #47794, #20061, #65141, #14532, #52608, #2014, #37066, #70324, #19700, #58130, #42253, #14167, #36701, #59223, #10822, #15622, #27462, #9730, #27097, #26731, #43358, #3471, #21906, #66993, #3836, #21168, #37440, #44462, #42981, #49629, #16355, #38910, #65881, #32264, #54437, #55171, #15262, #38164, #59961, #60687, #54075, #48896, #26357, #10102, #4567, #32631, #72156, #49993, #20432, #25991, #71426, #72517, #20803, #60320, #37800, #43721, #54796, #4203, #49266, #48530, #61429, #71799, #10463, #61066, #71057, #9368, #31900, #4927, #21535, #44090, #65512, #32993, #66244, #14899, #66617, #15993, #38542, #55533, #62159, #6368, #6007, #22626, #55895, #1202, #46258, #56263, #474, #16720, #23707, #22270, #28900, #68797, #18153, #45177, #11556, #33718, #34436, #67708, #17442, #39275, #68073, #63237, #28189, #5654, #62513, #56964, #11911, #39999, #29269, #72889, #5284, #51439, #61787, #50718, #34072, #51077, #67357, #11191, #121, #841, #17080, #45544, #22982, #28542, #17793, #39641, #12268, #40720, #33357, #23350, #45899, #56612, #68430, #40353, #62872, #34798, #57331, #6735, #27830, #51799, #50362, #44822, #58046, #2640, #42167, #18879, #47341, #42530, #19977, #7454, #46985, #30354, #69521, #35525, #29981, #52522, #1931, #1564, #14077, #41442, #12631, #35166, #46619, #24436, #70604, #64693, #35881, #52883, #19610, #7095, #41795, #63960, #36617, #13344, #13716, #57690, #52161, #41087, #25159, #53242, #29624, #59138, #64323, #8547, #31074, #47700, #70237, #53614, #18522, #24074, #3005, #25534, #63599, #48076, #58406, #7819, #2281, #24798, #69875, #30709, #58772, #12989, #19240, #69163, #36257, #8181, #65421, #44002, #31447, #66524, #70971, #60601, #14447, #53988, #25907, #59876, #59503, #14810, #37354, #37712, #10010, #15904, #4839, #3386, #66159, #48447, #49544, #10377, #32545, #27012 ),
 ( #42897, #36981, #8916, #9281, #31815, #20346, #20713, #54354, #54714, #55083, #3748, #21813, #43635, #65793, #48809, #72429, #26272, #27373, #71339, #4117, #60978, #43272, #15174, #55446, #60233, #26645, #21446, #4483, #38451, #9647, #72066, #32909, #32181, #38079, #49905, #49182, #71712, #21084, #65056, #15535, #50277, #62430, #56879, #33990, #67625, #62790, #16271, #45812, #55810, #16991, #39916, #56527, #5197, #66903, #44738, #38827, #17359, #67272, #33628, #23262, #67985, #50632, #16631, #68348, #10738, #17709, #72801, #11828, #61342, #33271, #27738, #39186, #22184, #61701, #11100, #39549, #34346, #40269, #57240, #56172, #45453, #5566, #28813, #12183, #6283, #51351, #28103, #36, #29182, #22542, #51715, #45090, #62073, #11467, #5920, #6653, #28454, #50989, #387, #22894, #753, #34710, #1117, #44377, #13627, #7732, #1481, #46172, #18071, #69076, #18436, #29540, #52439, #41002, #13261, #36170, #68711, #53526, #2200, #24352, #7369, #30993, #40632, #59053, #7009, #35799, #19528, #52076, #63517, #13994, #12904, #58321, #53159, #58688, #2557, #29900, #41712, #42086, #23987, #69792, #64608, #63151, #35437, #1845, #8099, #12546, #46534, #64238, #30627, #30266, #46900, #36533, #35080, #25075, #57606, #69439, #19158, #52799, #57961, #18796, #41360, #63870, #47618, #70150, #24715, #8458, #47258, #23626, #9922, #66072, #15450, #43917, #8827, #64973, #66443, #26930, #31363, #37995, #70887, #59789, #48361, #54268, #65706, #20998, #25824, #48725, #43550, #4401, #15819, #42451, #4031, #14364, #60517, #21363, #32461, #54995, #36899, #59419, #60889, #25451, #10294, #53904, #3297, #19898, #47995, #38363, #20260, #42812, #65335, #70523, #9195, #26556, #71248, #49455, #71989, #60151, #14725, #37267, #31730, #3662, #26185, #20627, #43186, #15092, #37628, #32825, #9561, #2921, #54625, #32094, #49096, #71625, #49823, #17630, #38741, #45008, #51269, #10655, #50191, #45733, #72716, #67544, #11745, #45366, #34262, #39100, #305, #672, #61261, #28370, #23179, #72347, #27652, #61617, #39835, #21728, #33185, #22815, #67902, #16907, #5482, #68268, #27289, #56795, #66817, #28021, #50907, #39462, #16190, #4756, #55724, #44288, #17273, #62349, #5118, #6201, #11385, #28728, #40190, #62711, #12105, #55363, #22099, #44657, #67187, #16548, #11019, #33540, #56091, #50549, #73077, #22458, #61984, #33904, #56448, #5838, #23906, #14547, #58242, #40924, #34999, #37083, #1036, #59607, #40550, #31176, #57157, #23543, #68629, #29460, #29100, #57529, #13181, #18351, #46821, #1758, #7291, #20077, #68992, #9021, #26007, #48546, #35720, #24272, #6929, #57881, #63067, #53719, #17991, #25640, #29820, #51635, #42633, #6569, #12470, #51996, #48178, #65157, #63437, #69358, #65529, #42998, #1397, #12823, #52355, #35357, #46454, #18716, #41280, #63791, #46093, #31552, #8647, #34628, #3111, #70702, #54091, #20448, #3489, #71073, #55187, #21922, #9385, #44106, #21185, #38925, #32280, #16010, #59976, #54453, #43374, #9746, #61444, #54814, #43736, #4220, #4582, #26748, #71814, #37817, #31917, #55909, #32646, #44478, #67009, #10838, #20819, #65898, #33373, #49645, #66632, #72903, #16370, #15278, #3852, #60337, #44837, #72172, #5301, #66260, #61081, #60703, #49281, #37457, #27847, #50378, #15638, #27112, #71444, #22285, #26374, #10479, #14915, #48913, #38179, #10116, #21551, #38558, #33008, #55547, #4943, #27477, #50009, #72534, #67724, #23364, #68444, #45912, #857, #63251, #33734, #16735, #17806, #50734, #11573, #68090, #11926, #28205, #45192, #136, #39290, #29637, #22642, #17097, #56280, #61804, #490, #40367, #40015, #18166, #57343, #51454, #39657, #11207, #5669, #62176, #34088, #56629, #22999, #6023, #56979, #6749, #28558, #24086, #62885, #17457, #51093, #1577, #45559, #52175, #62529, #6383, #12643, #34451, #28916, #57703, #12280, #34813, #23721, #29282, #46271, #51812, #1215, #35179, #68810, #40735, #7108, #67372, #18892, #30369, #31089, #13001, #52534, #64707, #59153, #36273, #69889, #65072, #18536, #48094, #58058, #19254, #42182, #58787, #7467, #69175, #46998, #41100, #8561, #14091, #63610, #3020, #2656, #70618, #53628, #36631, #25551, #14463, #1943, #35538, #36996, #19992, #24449, #42545, #41454, #52898, #63972, #24811, #8197, #59519, #19626, #69533, #35896, #8932, #70253, #2296, #13355, #31462, #29993, #54005, #58420, #3401, #7832, #47357, #41809, #64339, #13731, #30726, #53258, #25174, #46633, #47715, #38842, #65436, #27028, #37369, #10392, #44393, #66539, #60993, #59892, #9297, #10754, #48462, #33285, #3763, #14827, #42913, #20729, #16287, #43288, #15550, #55462, #15919, #4854, #9663, #44017, #21828, #31830, #72080, #66918, #20362, #71355, #32196, #32924, #54368, #26287, #38467, #27388, #38093, #49196, #61357, #70986, #49920, #48824, #71729, #21463, #60616, #65808, #15190, #37728, #60248, #72444, #55824, #54729, #25922, #55099, #4132, #26662, #21099, #43650, #66174, #10025, #32561, #4499, #49559, #11115, #17722, #51, #62088, #50647, #56541, #67999, #23275, #51365, #5581, #67640, #57253, #28826, #11481, #28118, #6667, #44753, #29195, #33644, #767, #27753, #67287, #39202, #22556, #72816, #45104, #17006, #51003, #45825, #51729, #18084, #16646, #6297, #61716, #62803, #23639, #68361, #40282, #56188, #39563, #63164, #50293, #12559, #34004, #5934, #22199, #28468, #40645, #401, #22909, #45467, #17372, #39929, #12196, #62443, #1130, #34723, #11841, #34360, #56892, #46185, #68724, #35094, #5212, #69451, #57974, #7744, #13640, #7022, #8472, #47271, #41372, #24365, #59067, #52089, #14009, #69089, #30280, #19542, #41015, #36548, #69805, #52813, #35450, #63882, #63530, #64252, #18450, #36184, #13273, #29553, #30640, #1494, #12917, #7381, #58702, #53172, #46912, #2213, #57619, #24000, #18808, #35811, #24728, #58333 ) ),
 .UNSPECIFIED., .F., .F., .F. ) 
 B_SPLINE_SURFACE_WITH_KNOTS ( ( 2, 2 ),
 ( 3, 2, 2, 2, 2, 2, 2, 2, 2, 2, 2, 2, 2, 2, 2, 2, 2, 2, 2, 2, 2, 2, 2, 2, 2, 2, 2, 2, 2, 2, 2, 2, 2, 2, 2, 2, 2, 2, 2, 2, 2, 2, 2, 2, 2, 2, 2, 2, 2, 2, 2, 2, 2, 2, 2, 2, 2, 2, 2, 2, 2, 2, 2, 2, 2, 2, 2, 2, 2, 2, 2, 2, 2, 2, 2, 2, 2, 2, 2, 2, 2, 2, 2, 2, 2, 2, 2, 2, 2, 2, 2, 2, 2, 2, 2, 2, 2, 2, 2, 2, 2, 2, 2, 2, 2, 2, 2, 2, 2, 2, 2, 2, 2, 2, 2, 2, 2, 2, 2, 2, 2, 2, 2, 2, 2, 2, 2, 2, 2, 2, 2, 2, 2, 2, 2, 2, 2, 2, 2, 2, 2, 2, 2, 2, 2, 2, 2, 2, 2, 2, 2, 2, 2, 2, 2, 2, 2, 2, 2, 2, 2, 2, 2, 2, 2, 2, 2, 2, 2, 2, 2, 2, 2, 2, 2, 2, 2, 2, 2, 2, 2, 2, 2, 2, 2, 2, 2, 2, 2, 2, 2, 2, 2, 2, 2, 2, 2, 2, 2, 2, 2, 2, 2, 2, 2, 2, 2, 2, 2, 2, 2, 2, 2, 2, 2, 2, 2, 2, 2, 2, 2, 2, 2, 2, 2, 2, 2, 2, 2, 2, 2, 2, 2, 2, 2, 2, 2, 2, 2, 2, 2, 2, 2, 2, 2, 2, 2, 2, 2, 2, 2, 2, 2, 2, 2, 2, 2, 2, 2, 2, 2, 2, 2, 2, 2, 2, 2, 2, 2, 2, 2, 2, 2, 2, 2, 2, 2, 2, 2, 2, 2, 2, 2, 2, 2, 2, 2, 2, 2, 2, 2, 2, 2, 2, 2, 2, 2, 2, 2, 2, 2, 2, 2, 2, 2, 2, 2, 2, 2, 2, 2, 2, 2, 2, 2, 2, 2, 2, 2, 2, 2, 2, 2, 2, 2, 2, 2, 2, 2, 2, 2, 2, 2, 2, 2, 2, 2, 2, 2, 2, 2, 2, 2, 2, 2, 2, 2, 2, 2, 2, 2, 2, 2, 2, 2, 2, 2, 2, 2, 2, 3 ),
 ( 0.000000000000000000, 1.000000000000000000 ),
 ( 0.000000000000000000, 0.002777777777777777884, 0.005555555555555555768, 0.008333333333333333218, 0.01111111111111111154, 0.01388888888888888812, 0.01666666666666666644, 0.01944444444444444475, 0.02222222222222222307, 0.02500000000000000139, 0.02777777777777777624, 0.03055555555555555455, 0.03333333333333333287, 0.03611111111111110772, 0.03888888888888888951, 0.04166666666666666435, 0.04444444444444444614, 0.04722222222222222099, 0.05000000000000000278, 0.05277777777777777762, 0.05555555555555555247, 0.05833333333333333426, 0.06111111111111110911, 0.06388888888888888395, 0.06666666666666666574, 0.06944444444444444753, 0.07222222222222221544, 0.07499999999999999722, 0.07777777777777777901, 0.08055555555555556080, 0.08333333333333332871, 0.08611111111111111049, 0.08888888888888889228, 0.09166666666666666019, 0.09444444444444444198, 0.09722222222222222376, 0.1000000000000000056, 0.1027777777777777735, 0.1055555555555555552, 0.1083333333333333370, 0.1111111111111111049, 0.1138888888888888867, 0.1166666666666666685, 0.1194444444444444503, 0.1222222222222222182, 0.1250000000000000000, 0.1277777777777777679, 0.1305555555555555636, 0.1333333333333333315, 0.1361111111111110994, 0.1388888888888888951, 0.1416666666666666630, 0.1444444444444444309, 0.1472222222222222265, 0.1499999999999999944, 0.1527777777777777901, 0.1555555555555555580, 0.1583333333333333259, 0.1611111111111111216, 0.1638888888888888895, 0.1666666666666666574, 0.1694444444444444531, 0.1722222222222222210, 0.1749999999999999889, 0.1777777777777777846, 0.1805555555555555525, 0.1833333333333333204, 0.1861111111111111160, 0.1888888888888888840, 0.1916666666666666796, 0.1944444444444444475, 0.1972222222222222154, 0.2000000000000000111, 0.2027777777777777790, 0.2055555555555555469, 0.2083333333333333426, 0.2111111111111111105, 0.2138888888888888784, 0.2166666666666666741, 0.2194444444444444420, 0.2222222222222222099, 0.2250000000000000056, 0.2277777777777777735, 0.2305555555555555691, 0.2333333333333333370, 0.2361111111111111049, 0.2388888888888889006, 0.2416666666666666685, 0.2444444444444444364, 0.2472222222222222321, 0.2500000000000000000, 0.2527777777777777679, 0.2555555555555555358, 0.2583333333333333592, 0.2611111111111111271, 0.2638888888888888951, 0.2666666666666666630, 0.2694444444444444309, 0.2722222222222221988, 0.2750000000000000222, 0.2777777777777777901, 0.2805555555555555580, 0.2833333333333333259, 0.2861111111111110938, 0.2888888888888888618, 0.2916666666666666852, 0.2944444444444444531, 0.2972222222222222210, 0.2999999999999999889, 0.3027777777777777568, 0.3055555555555555802, 0.3083333333333333481, 0.3111111111111111160, 0.3138888888888888840, 0.3166666666666666519, 0.3194444444444444198, 0.3222222222222222432, 0.3250000000000000111, 0.3277777777777777790, 0.3305555555555555469, 0.3333333333333333148, 0.3361111111111111382, 0.3388888888888889062, 0.3416666666666666741, 0.3444444444444444420, 0.3472222222222222099, 0.3499999999999999778, 0.3527777777777778012, 0.3555555555555555691, 0.3583333333333333370, 0.3611111111111111049, 0.3638888888888888729, 0.3666666666666666408, 0.3694444444444444642, 0.3722222222222222321, 0.3750000000000000000, 0.3777777777777777679, 0.3805555555555555358, 0.3833333333333333592, 0.3861111111111111271, 0.3888888888888888951, 0.3916666666666666630, 0.3944444444444444309, 0.3972222222222221988, 0.4000000000000000222, 0.4027777777777777901, 0.4055555555555555580, 0.4083333333333333259, 0.4111111111111110938, 0.4138888888888888618, 0.4166666666666666852, 0.4194444444444444531, 0.4222222222222222210, 0.4249999999999999889, 0.4277777777777777568, 0.4305555555555555802, 0.4333333333333333481, 0.4361111111111111160, 0.4388888888888888840, 0.4416666666666666519, 0.4444444444444444198, 0.4472222222222222432, 0.4500000000000000111, 0.4527777777777777790, 0.4555555555555555469, 0.4583333333333333148, 0.4611111111111111382, 0.4638888888888889062, 0.4666666666666666741, 0.4694444444444444420, 0.4722222222222222099, 0.4749999999999999778, 0.4777777777777778012, 0.4805555555555555691, 0.4833333333333333370, 0.4861111111111111049, 0.4888888888888888729, 0.4916666666666666408, 0.4944444444444444642, 0.4972222222222222321, 0.5000000000000000000, 0.5027777777777777679, 0.5055555555555555358, 0.5083333333333333037, 0.5111111111111110716, 0.5138888888888888395, 0.5166666666666667185, 0.5194444444444444864, 0.5222222222222222543, 0.5250000000000000222, 0.5277777777777777901, 0.5305555555555555580, 0.5333333333333333259, 0.5361111111111110938, 0.5388888888888888618, 0.5416666666666666297, 0.5444444444444443976, 0.5472222222222222765, 0.5500000000000000444, 0.5527777777777778123, 0.5555555555555555802, 0.5583333333333333481, 0.5611111111111111160, 0.5638888888888888840, 0.5666666666666666519, 0.5694444444444444198, 0.5722222222222221877, 0.5749999999999999556, 0.5777777777777777235, 0.5805555555555556024, 0.5833333333333333703, 0.5861111111111111382, 0.5888888888888889062, 0.5916666666666666741, 0.5944444444444444420, 0.5972222222222222099, 0.5999999999999999778, 0.6027777777777777457, 0.6055555555555555136, 0.6083333333333332815, 0.6111111111111111605, 0.6138888888888889284, 0.6166666666666666963, 0.6194444444444444642, 0.6222222222222222321, 0.6250000000000000000, 0.6277777777777777679, 0.6305555555555555358, 0.6333333333333333037, 0.6361111111111110716, 0.6388888888888888395, 0.6416666666666667185, 0.6444444444444444864, 0.6472222222222222543, 0.6500000000000000222, 0.6527777777777777901, 0.6555555555555555580, 0.6583333333333333259, 0.6611111111111110938, 0.6638888888888888618, 0.6666666666666666297, 0.6694444444444443976, 0.6722222222222222765, 0.6750000000000000444, 0.6777777777777778123, 0.6805555555555555802, 0.6833333333333333481, 0.6861111111111111160, 0.6888888888888888840, 0.6916666666666666519, 0.6944444444444444198, 0.6972222222222221877, 0.6999999999999999556, 0.7027777777777777235, 0.7055555555555556024, 0.7083333333333333703, 0.7111111111111111382, 0.7138888888888889062, 0.7166666666666666741, 0.7194444444444444420, 0.7222222222222222099, 0.7249999999999999778, 0.7277777777777777457, 0.7305555555555555136, 0.7333333333333332815, 0.7361111111111111605, 0.7388888888888889284, 0.7416666666666666963, 0.7444444444444444642, 0.7472222222222222321, 0.7500000000000000000, 0.7527777777777777679, 0.7555555555555555358, 0.7583333333333333037, 0.7611111111111110716, 0.7638888888888888395, 0.7666666666666667185, 0.7694444444444444864, 0.7722222222222222543, 0.7750000000000000222, 0.7777777777777777901, 0.7805555555555555580, 0.7833333333333333259, 0.7861111111111110938, 0.7888888888888888618, 0.7916666666666666297, 0.7944444444444443976, 0.7972222222222222765, 0.8000000000000000444, 0.8027777777777778123, 0.8055555555555555802, 0.8083333333333333481, 0.8111111111111111160, 0.8138888888888888840, 0.8166666666666666519, 0.8194444444444444198, 0.8222222222222221877, 0.8249999999999999556, 0.8277777777777777235, 0.8305555555555556024, 0.8333333333333333703, 0.8361111111111111382, 0.8388888888888889062, 0.8416666666666666741, 0.8444444444444444420, 0.8472222222222222099, 0.8499999999999999778, 0.8527777777777777457, 0.8555555555555555136, 0.8583333333333332815, 0.8611111111111111605, 0.8638888888888889284, 0.8666666666666666963, 0.8694444444444444642, 0.8722222222222222321, 0.8750000000000000000, 0.8777777777777777679, 0.8805555555555555358, 0.8833333333333333037, 0.8861111111111110716, 0.8888888888888888395, 0.8916666666666667185, 0.8944444444444444864, 0.8972222222222222543, 0.9000000000000000222, 0.9027777777777777901, 0.9055555555555555580, 0.9083333333333333259, 0.9111111111111110938, 0.9138888888888888618, 0.9166666666666666297, 0.9194444444444443976, 0.9222222222222222765, 0.9250000000000000444, 0.9277777777777778123, 0.9305555555555555802, 0.9333333333333333481, 0.9361111111111111160, 0.9388888888888888840, 0.9416666666666666519, 0.9444444444444444198, 0.9472222222222221877, 0.9499999999999999556, 0.9527777777777777235, 0.9555555555555556024, 0.9583333333333333703, 0.9611111111111111382, 0.9638888888888889062, 0.9666666666666666741, 0.9694444444444444420, 0.9722222222222222099, 0.9749999999999999778, 0.9777777777777777457, 0.9805555555555555136, 0.9833333333333332815, 0.9861111111111111605, 0.9888888888888889284, 0.9916666666666666963, 0.9944444444444444642, 0.9972222222222222321, 1.000000000000000000 ),
 .UNSPECIFIED. ) 
 GEOMETRIC_REPRESENTATION_ITEM ( )  RATIONAL_B_SPLINE_SURFACE ( (
 ( 1.000000000000000000, 0.8660254037844387076, 1.000000000000000000, 0.8660254037844387076, 1.000000000000000000, 0.8660254037844387076, 1.000000000000000000, 0.8660254037844387076, 1.000000000000000000, 0.8660254037844387076, 1.000000000000000000, 0.8660254037844387076, 1.000000000000000000, 0.8660254037844387076, 1.000000000000000000, 0.8660254037844387076, 1.000000000000000000, 0.8660254037844387076, 1.000000000000000000, 0.8660254037844387076, 1.000000000000000000, 0.8660254037844387076, 1.000000000000000000, 0.8660254037844387076, 1.000000000000000000, 0.8660254037844387076, 1.000000000000000000, 0.8660254037844387076, 1.000000000000000000, 0.8660254037844387076, 1.000000000000000000, 0.8660254037844387076, 1.000000000000000000, 0.8660254037844387076, 1.000000000000000000, 0.8660254037844387076, 1.000000000000000000, 0.8660254037844387076, 1.000000000000000000, 0.8660254037844387076, 1.000000000000000000, 0.8660254037844387076, 1.000000000000000000, 0.8660254037844387076, 1.000000000000000000, 0.8660254037844387076, 1.000000000000000000, 0.8660254037844387076, 1.000000000000000000, 0.8660254037844387076, 1.000000000000000000, 0.8660254037844387076, 1.000000000000000000, 0.8660254037844387076, 1.000000000000000000, 0.8660254037844387076, 1.000000000000000000, 0.8660254037844387076, 1.000000000000000000, 0.8660254037844387076, 1.000000000000000000, 0.8660254037844387076, 1.000000000000000000, 0.8660254037844387076, 1.000000000000000000, 0.8660254037844387076, 1.000000000000000000, 0.8660254037844387076, 1.000000000000000000, 0.8660254037844387076, 1.000000000000000000, 0.8660254037844387076, 1.000000000000000000, 0.8660254037844387076, 1.000000000000000000, 0.8660254037844387076, 1.000000000000000000, 0.8660254037844387076, 1.000000000000000000, 0.8660254037844387076, 1.000000000000000000, 0.8660254037844387076, 1.000000000000000000, 0.8660254037844387076, 1.000000000000000000, 0.8660254037844387076, 1.000000000000000000, 0.8660254037844387076, 1.000000000000000000, 0.8660254037844387076, 1.000000000000000000, 0.8660254037844387076, 1.000000000000000000, 0.8660254037844387076, 1.000000000000000000, 0.8660254037844387076, 1.000000000000000000, 0.8660254037844387076, 1.000000000000000000, 0.8660254037844387076, 1.000000000000000000, 0.8660254037844387076, 1.000000000000000000, 0.8660254037844387076, 1.000000000000000000, 0.8660254037844387076, 1.000000000000000000, 0.8660254037844387076, 1.000000000000000000, 0.8660254037844387076, 1.000000000000000000, 0.8660254037844387076, 1.000000000000000000, 0.8660254037844387076, 1.000000000000000000, 0.8660254037844387076, 1.000000000000000000, 0.8660254037844387076, 1.000000000000000000, 0.8660254037844387076, 1.000000000000000000, 0.8660254037844387076, 1.000000000000000000, 0.8660254037844387076, 1.000000000000000000, 0.8660254037844387076, 1.000000000000000000, 0.8660254037844387076, 1.000000000000000000, 0.8660254037844387076, 1.000000000000000000, 0.8660254037844387076, 1.000000000000000000, 0.8660254037844387076, 1.000000000000000000, 0.8660254037844387076, 1.000000000000000000, 0.8660254037844387076, 1.000000000000000000, 0.8660254037844387076, 1.000000000000000000, 0.8660254037844387076, 1.000000000000000000, 0.8660254037844387076, 1.000000000000000000, 0.8660254037844387076, 1.000000000000000000, 0.8660254037844387076, 1.000000000000000000, 0.8660254037844387076, 1.000000000000000000, 0.8660254037844387076, 1.000000000000000000, 0.8660254037844387076, 1.000000000000000000, 0.8660254037844387076, 1.000000000000000000, 0.8660254037844387076, 1.000000000000000000, 0.8660254037844387076, 1.000000000000000000, 0.8660254037844387076, 1.000000000000000000, 0.8660254037844387076, 1.000000000000000000, 0.8660254037844387076, 1.000000000000000000, 0.8660254037844387076, 1.000000000000000000, 0.8660254037844387076, 1.000000000000000000, 0.8660254037844387076, 1.000000000000000000, 0.8660254037844387076, 1.000000000000000000, 0.8660254037844387076, 1.000000000000000000, 0.8660254037844387076, 1.000000000000000000, 0.8660254037844387076, 1.000000000000000000, 0.8660254037844387076, 1.000000000000000000, 0.8660254037844387076, 1.000000000000000000, 0.8660254037844387076, 1.000000000000000000, 0.8660254037844387076, 1.000000000000000000, 0.8660254037844387076, 1.000000000000000000, 0.8660254037844387076, 1.000000000000000000, 0.8660254037844387076, 1.000000000000000000, 0.8660254037844387076, 1.000000000000000000, 0.8660254037844387076, 1.000000000000000000, 0.8660254037844387076, 1.000000000000000000, 0.8660254037844387076, 1.000000000000000000, 0.8660254037844387076, 1.000000000000000000, 0.8660254037844387076, 1.000000000000000000, 0.8660254037844387076, 1.000000000000000000, 0.8660254037844387076, 1.000000000000000000, 0.8660254037844387076, 1.000000000000000000, 0.8660254037844387076, 1.000000000000000000, 0.8660254037844387076, 1.000000000000000000, 0.8660254037844387076, 1.000000000000000000, 0.8660254037844387076, 1.000000000000000000, 0.8660254037844387076, 1.000000000000000000, 0.8660254037844387076, 1.000000000000000000, 0.8660254037844387076, 1.000000000000000000, 0.8660254037844387076, 1.000000000000000000, 0.8660254037844387076, 1.000000000000000000, 0.8660254037844387076, 1.000000000000000000, 0.8660254037844387076, 1.000000000000000000, 0.8660254037844387076, 1.000000000000000000, 0.8660254037844387076, 1.000000000000000000, 0.8660254037844387076, 1.000000000000000000, 0.8660254037844387076, 1.000000000000000000, 0.8660254037844387076, 1.000000000000000000, 0.8660254037844387076, 1.000000000000000000, 0.8660254037844387076, 1.000000000000000000, 0.8660254037844387076, 1.000000000000000000, 0.8660254037844387076, 1.000000000000000000, 0.8660254037844387076, 1.000000000000000000, 0.8660254037844387076, 1.000000000000000000, 0.8660254037844387076, 1.000000000000000000, 0.8660254037844387076, 1.000000000000000000, 0.8660254037844387076, 1.000000000000000000, 0.8660254037844387076, 1.000000000000000000, 0.8660254037844387076, 1.000000000000000000, 0.8660254037844387076, 1.000000000000000000, 0.8660254037844387076, 1.000000000000000000, 0.8660254037844387076, 1.000000000000000000, 0.8660254037844387076, 1.000000000000000000, 0.8660254037844387076, 1.000000000000000000, 0.8660254037844387076, 1.000000000000000000, 0.8660254037844387076, 1.000000000000000000, 0.8660254037844387076, 1.000000000000000000, 0.8660254037844387076, 1.000000000000000000, 0.8660254037844387076, 1.000000000000000000, 0.8660254037844387076, 1.000000000000000000, 0.8660254037844387076, 1.000000000000000000, 0.8660254037844387076, 1.000000000000000000, 0.8660254037844387076, 1.000000000000000000, 0.8660254037844387076, 1.000000000000000000, 0.8660254037844387076, 1.000000000000000000, 0.8660254037844387076, 1.000000000000000000, 0.8660254037844387076, 1.000000000000000000, 0.8660254037844387076, 1.000000000000000000, 0.8660254037844387076, 1.000000000000000000, 0.8660254037844387076, 1.000000000000000000, 0.8660254037844387076, 1.000000000000000000, 0.8660254037844387076, 1.000000000000000000, 0.8660254037844387076, 1.000000000000000000, 0.8660254037844387076, 1.000000000000000000, 0.8660254037844387076, 1.000000000000000000, 0.8660254037844387076, 1.000000000000000000, 0.8660254037844387076, 1.000000000000000000, 0.8660254037844387076, 1.000000000000000000, 0.8660254037844387076, 1.000000000000000000, 0.8660254037844387076, 1.000000000000000000, 0.8660254037844387076, 1.000000000000000000, 0.8660254037844387076, 1.000000000000000000, 0.8660254037844387076, 1.000000000000000000, 0.8660254037844387076, 1.000000000000000000, 0.8660254037844387076, 1.000000000000000000, 0.8660254037844387076, 1.000000000000000000, 0.8660254037844387076, 1.000000000000000000, 0.8660254037844387076, 1.000000000000000000, 0.8660254037844387076, 1.000000000000000000, 0.8660254037844387076, 1.000000000000000000, 0.8660254037844387076, 1.000000000000000000, 0.8660254037844387076, 1.000000000000000000, 0.8660254037844387076, 1.000000000000000000, 0.8660254037844387076, 1.000000000000000000, 0.8660254037844387076, 1.000000000000000000, 0.8660254037844387076, 1.000000000000000000, 0.8660254037844387076, 1.000000000000000000, 0.8660254037844387076, 1.000000000000000000, 0.8660254037844387076, 1.000000000000000000, 0.8660254037844387076, 1.000000000000000000, 0.8660254037844387076, 1.000000000000000000, 0.8660254037844387076, 1.000000000000000000, 0.8660254037844387076, 1.000000000000000000, 0.8660254037844387076, 1.000000000000000000, 0.8660254037844387076, 1.000000000000000000, 0.8660254037844387076, 1.000000000000000000, 0.8660254037844387076, 1.000000000000000000, 0.8660254037844387076, 1.000000000000000000, 0.8660254037844387076, 1.000000000000000000, 0.8660254037844387076, 1.000000000000000000, 0.8660254037844387076, 1.000000000000000000, 0.8660254037844387076, 1.000000000000000000, 0.8660254037844387076, 1.000000000000000000, 0.8660254037844387076, 1.000000000000000000, 0.8660254037844387076, 1.000000000000000000, 0.8660254037844387076, 1.000000000000000000, 0.8660254037844387076, 1.000000000000000000, 0.8660254037844387076, 1.000000000000000000, 0.8660254037844387076, 1.000000000000000000, 0.8660254037844387076, 1.000000000000000000, 0.8660254037844387076, 1.000000000000000000, 0.8660254037844387076, 1.000000000000000000, 0.8660254037844387076, 1.000000000000000000, 0.8660254037844387076, 1.000000000000000000, 0.8660254037844387076, 1.000000000000000000, 0.8660254037844387076, 1.000000000000000000, 0.8660254037844387076, 1.000000000000000000, 0.8660254037844387076, 1.000000000000000000, 0.8660254037844387076, 1.000000000000000000, 0.8660254037844387076, 1.000000000000000000, 0.8660254037844387076, 1.000000000000000000, 0.8660254037844387076, 1.000000000000000000, 0.8660254037844387076, 1.000000000000000000, 0.8660254037844387076, 1.000000000000000000, 0.8660254037844387076, 1.000000000000000000, 0.8660254037844387076, 1.000000000000000000, 0.8660254037844387076, 1.000000000000000000, 0.8660254037844387076, 1.000000000000000000, 0.8660254037844387076, 1.000000000000000000, 0.8660254037844387076, 1.000000000000000000, 0.8660254037844387076, 1.000000000000000000, 0.8660254037844387076, 1.000000000000000000, 0.8660254037844387076, 1.000000000000000000, 0.8660254037844387076, 1.000000000000000000, 0.8660254037844387076, 1.000000000000000000, 0.8660254037844387076, 1.000000000000000000, 0.8660254037844387076, 1.000000000000000000, 0.8660254037844387076, 1.000000000000000000, 0.8660254037844387076, 1.000000000000000000, 0.8660254037844387076, 1.000000000000000000, 0.8660254037844387076, 1.000000000000000000, 0.8660254037844387076, 1.000000000000000000, 0.8660254037844387076, 1.000000000000000000, 0.8660254037844387076, 1.000000000000000000, 0.8660254037844387076, 1.000000000000000000, 0.8660254037844387076, 1.000000000000000000, 0.8660254037844387076, 1.000000000000000000, 0.8660254037844387076, 1.000000000000000000, 0.8660254037844387076, 1.000000000000000000, 0.8660254037844387076, 1.000000000000000000, 0.8660254037844387076, 1.000000000000000000, 0.8660254037844387076, 1.000000000000000000, 0.8660254037844387076, 1.000000000000000000, 0.8660254037844387076, 1.000000000000000000, 0.8660254037844387076, 1.000000000000000000, 0.8660254037844387076, 1.000000000000000000, 0.8660254037844387076, 1.000000000000000000, 0.8660254037844387076, 1.000000000000000000, 0.8660254037844387076, 1.000000000000000000, 0.8660254037844387076, 1.000000000000000000, 0.8660254037844387076, 1.000000000000000000, 0.8660254037844387076, 1.000000000000000000, 0.8660254037844387076, 1.000000000000000000, 0.8660254037844387076, 1.000000000000000000, 0.8660254037844387076, 1.000000000000000000, 0.8660254037844387076, 1.000000000000000000, 0.8660254037844387076, 1.000000000000000000, 0.8660254037844387076, 1.000000000000000000, 0.8660254037844387076, 1.000000000000000000, 0.8660254037844387076, 1.000000000000000000, 0.8660254037844387076, 1.000000000000000000, 0.8660254037844387076, 1.000000000000000000, 0.8660254037844387076, 1.000000000000000000, 0.8660254037844387076, 1.000000000000000000, 0.8660254037844387076, 1.000000000000000000, 0.8660254037844387076, 1.000000000000000000, 0.8660254037844387076, 1.000000000000000000, 0.8660254037844387076, 1.000000000000000000, 0.8660254037844387076, 1.000000000000000000, 0.8660254037844387076, 1.000000000000000000, 0.8660254037844387076, 1.000000000000000000, 0.8660254037844387076, 1.000000000000000000, 0.8660254037844387076, 1.000000000000000000, 0.8660254037844387076, 1.000000000000000000, 0.8660254037844387076, 1.000000000000000000, 0.8660254037844387076, 1.000000000000000000, 0.8660254037844387076, 1.000000000000000000, 0.8660254037844387076, 1.000000000000000000, 0.8660254037844387076, 1.000000000000000000, 0.8660254037844387076, 1.000000000000000000, 0.8660254037844387076, 1.000000000000000000, 0.8660254037844387076, 1.000000000000000000, 0.8660254037844387076, 1.000000000000000000, 0.8660254037844387076, 1.000000000000000000, 0.8660254037844387076, 1.000000000000000000, 0.8660254037844387076, 1.000000000000000000, 0.8660254037844387076, 1.000000000000000000, 0.8660254037844387076, 1.000000000000000000, 0.8660254037844387076, 1.000000000000000000, 0.8660254037844387076, 1.000000000000000000, 0.8660254037844387076, 1.000000000000000000, 0.8660254037844387076, 1.000000000000000000, 0.8660254037844387076, 1.000000000000000000, 0.8660254037844387076, 1.000000000000000000, 0.8660254037844387076, 1.000000000000000000, 0.8660254037844387076, 1.000000000000000000, 0.8660254037844387076, 1.000000000000000000, 0.8660254037844387076, 1.000000000000000000, 0.8660254037844387076, 1.000000000000000000, 0.8660254037844387076, 1.000000000000000000, 0.8660254037844387076, 1.000000000000000000, 0.8660254037844387076, 1.000000000000000000, 0.8660254037844387076, 1.000000000000000000, 0.8660254037844387076, 1.000000000000000000, 0.8660254037844387076, 1.000000000000000000, 0.8660254037844387076, 1.000000000000000000, 0.8660254037844387076, 1.000000000000000000, 0.8660254037844387076, 1.000000000000000000, 0.8660254037844387076, 1.000000000000000000, 0.8660254037844387076, 1.000000000000000000, 0.8660254037844387076, 1.000000000000000000, 0.8660254037844387076, 1.000000000000000000, 0.8660254037844387076, 1.000000000000000000, 0.8660254037844387076, 1.000000000000000000, 0.8660254037844387076, 1.000000000000000000, 0.8660254037844387076, 1.000000000000000000, 0.8660254037844387076, 1.000000000000000000, 0.8660254037844387076, 1.000000000000000000, 0.8660254037844387076, 1.000000000000000000, 0.8660254037844387076, 1.000000000000000000, 0.8660254037844387076, 1.000000000000000000, 0.8660254037844387076, 1.000000000000000000, 0.8660254037844387076, 1.000000000000000000, 0.8660254037844387076, 1.000000000000000000, 0.8660254037844387076, 1.000000000000000000, 0.8660254037844387076, 1.000000000000000000, 0.8660254037844387076, 1.000000000000000000, 0.8660254037844387076, 1.000000000000000000, 0.8660254037844387076, 1.000000000000000000, 0.8660254037844387076, 1.000000000000000000, 0.8660254037844387076, 1.000000000000000000, 0.8660254037844387076, 1.000000000000000000, 0.8660254037844387076, 1.000000000000000000, 0.8660254037844387076, 1.000000000000000000, 0.8660254037844387076, 1.000000000000000000, 0.8660254037844387076, 1.000000000000000000, 0.8660254037844387076, 1.000000000000000000, 0.8660254037844387076, 1.000000000000000000, 0.8660254037844387076, 1.000000000000000000, 0.8660254037844387076, 1.000000000000000000, 0.8660254037844387076, 1.000000000000000000, 0.8660254037844387076, 1.000000000000000000, 0.8660254037844387076, 1.000000000000000000, 0.8660254037844387076, 1.000000000000000000, 0.8660254037844387076, 1.000000000000000000, 0.8660254037844387076, 1.000000000000000000, 0.8660254037844387076, 1.000000000000000000, 0.8660254037844387076, 1.000000000000000000, 0.8660254037844387076, 1.000000000000000000, 0.8660254037844387076, 1.000000000000000000, 0.8660254037844387076, 1.000000000000000000, 0.8660254037844387076, 1.000000000000000000, 0.8660254037844387076, 1.000000000000000000, 0.8660254037844387076, 1.000000000000000000, 0.8660254037844387076, 1.000000000000000000, 0.8660254037844387076, 1.000000000000000000),
 ( 1.000000000000000000, 0.8660254037844387076, 1.000000000000000000, 0.8660254037844387076, 1.000000000000000000, 0.8660254037844387076, 1.000000000000000000, 0.8660254037844387076, 1.000000000000000000, 0.8660254037844387076, 1.000000000000000000, 0.8660254037844387076, 1.000000000000000000, 0.8660254037844387076, 1.000000000000000000, 0.8660254037844387076, 1.000000000000000000, 0.8660254037844387076, 1.000000000000000000, 0.8660254037844387076, 1.000000000000000000, 0.8660254037844387076, 1.000000000000000000, 0.8660254037844387076, 1.000000000000000000, 0.8660254037844387076, 1.000000000000000000, 0.8660254037844387076, 1.000000000000000000, 0.8660254037844387076, 1.000000000000000000, 0.8660254037844387076, 1.000000000000000000, 0.8660254037844387076, 1.000000000000000000, 0.8660254037844387076, 1.000000000000000000, 0.8660254037844387076, 1.000000000000000000, 0.8660254037844387076, 1.000000000000000000, 0.8660254037844387076, 1.000000000000000000, 0.8660254037844387076, 1.000000000000000000, 0.8660254037844387076, 1.000000000000000000, 0.8660254037844387076, 1.000000000000000000, 0.8660254037844387076, 1.000000000000000000, 0.8660254037844387076, 1.000000000000000000, 0.8660254037844387076, 1.000000000000000000, 0.8660254037844387076, 1.000000000000000000, 0.8660254037844387076, 1.000000000000000000, 0.8660254037844387076, 1.000000000000000000, 0.8660254037844387076, 1.000000000000000000, 0.8660254037844387076, 1.000000000000000000, 0.8660254037844387076, 1.000000000000000000, 0.8660254037844387076, 1.000000000000000000, 0.8660254037844387076, 1.000000000000000000, 0.8660254037844387076, 1.000000000000000000, 0.8660254037844387076, 1.000000000000000000, 0.8660254037844387076, 1.000000000000000000, 0.8660254037844387076, 1.000000000000000000, 0.8660254037844387076, 1.000000000000000000, 0.8660254037844387076, 1.000000000000000000, 0.8660254037844387076, 1.000000000000000000, 0.8660254037844387076, 1.000000000000000000, 0.8660254037844387076, 1.000000000000000000, 0.8660254037844387076, 1.000000000000000000, 0.8660254037844387076, 1.000000000000000000, 0.8660254037844387076, 1.000000000000000000, 0.8660254037844387076, 1.000000000000000000, 0.8660254037844387076, 1.000000000000000000, 0.8660254037844387076, 1.000000000000000000, 0.8660254037844387076, 1.000000000000000000, 0.8660254037844387076, 1.000000000000000000, 0.8660254037844387076, 1.000000000000000000, 0.8660254037844387076, 1.000000000000000000, 0.8660254037844387076, 1.000000000000000000, 0.8660254037844387076, 1.000000000000000000, 0.8660254037844387076, 1.000000000000000000, 0.8660254037844387076, 1.000000000000000000, 0.8660254037844387076, 1.000000000000000000, 0.8660254037844387076, 1.000000000000000000, 0.8660254037844387076, 1.000000000000000000, 0.8660254037844387076, 1.000000000000000000, 0.8660254037844387076, 1.000000000000000000, 0.8660254037844387076, 1.000000000000000000, 0.8660254037844387076, 1.000000000000000000, 0.8660254037844387076, 1.000000000000000000, 0.8660254037844387076, 1.000000000000000000, 0.8660254037844387076, 1.000000000000000000, 0.8660254037844387076, 1.000000000000000000, 0.8660254037844387076, 1.000000000000000000, 0.8660254037844387076, 1.000000000000000000, 0.8660254037844387076, 1.000000000000000000, 0.8660254037844387076, 1.000000000000000000, 0.8660254037844387076, 1.000000000000000000, 0.8660254037844387076, 1.000000000000000000, 0.8660254037844387076, 1.000000000000000000, 0.8660254037844387076, 1.000000000000000000, 0.8660254037844387076, 1.000000000000000000, 0.8660254037844387076, 1.000000000000000000, 0.8660254037844387076, 1.000000000000000000, 0.8660254037844387076, 1.000000000000000000, 0.8660254037844387076, 1.000000000000000000, 0.8660254037844387076, 1.000000000000000000, 0.8660254037844387076, 1.000000000000000000, 0.8660254037844387076, 1.000000000000000000, 0.8660254037844387076, 1.000000000000000000, 0.8660254037844387076, 1.000000000000000000, 0.8660254037844387076, 1.000000000000000000, 0.8660254037844387076, 1.000000000000000000, 0.8660254037844387076, 1.000000000000000000, 0.8660254037844387076, 1.000000000000000000, 0.8660254037844387076, 1.000000000000000000, 0.8660254037844387076, 1.000000000000000000, 0.8660254037844387076, 1.000000000000000000, 0.8660254037844387076, 1.000000000000000000, 0.8660254037844387076, 1.000000000000000000, 0.8660254037844387076, 1.000000000000000000, 0.8660254037844387076, 1.000000000000000000, 0.8660254037844387076, 1.000000000000000000, 0.8660254037844387076, 1.000000000000000000, 0.8660254037844387076, 1.000000000000000000, 0.8660254037844387076, 1.000000000000000000, 0.8660254037844387076, 1.000000000000000000, 0.8660254037844387076, 1.000000000000000000, 0.8660254037844387076, 1.000000000000000000, 0.8660254037844387076, 1.000000000000000000, 0.8660254037844387076, 1.000000000000000000, 0.8660254037844387076, 1.000000000000000000, 0.8660254037844387076, 1.000000000000000000, 0.8660254037844387076, 1.000000000000000000, 0.8660254037844387076, 1.000000000000000000, 0.8660254037844387076, 1.000000000000000000, 0.8660254037844387076, 1.000000000000000000, 0.8660254037844387076, 1.000000000000000000, 0.8660254037844387076, 1.000000000000000000, 0.8660254037844387076, 1.000000000000000000, 0.8660254037844387076, 1.000000000000000000, 0.8660254037844387076, 1.000000000000000000, 0.8660254037844387076, 1.000000000000000000, 0.8660254037844387076, 1.000000000000000000, 0.8660254037844387076, 1.000000000000000000, 0.8660254037844387076, 1.000000000000000000, 0.8660254037844387076, 1.000000000000000000, 0.8660254037844387076, 1.000000000000000000, 0.8660254037844387076, 1.000000000000000000, 0.8660254037844387076, 1.000000000000000000, 0.8660254037844387076, 1.000000000000000000, 0.8660254037844387076, 1.000000000000000000, 0.8660254037844387076, 1.000000000000000000, 0.8660254037844387076, 1.000000000000000000, 0.8660254037844387076, 1.000000000000000000, 0.8660254037844387076, 1.000000000000000000, 0.8660254037844387076, 1.000000000000000000, 0.8660254037844387076, 1.000000000000000000, 0.8660254037844387076, 1.000000000000000000, 0.8660254037844387076, 1.000000000000000000, 0.8660254037844387076, 1.000000000000000000, 0.8660254037844387076, 1.000000000000000000, 0.8660254037844387076, 1.000000000000000000, 0.8660254037844387076, 1.000000000000000000, 0.8660254037844387076, 1.000000000000000000, 0.8660254037844387076, 1.000000000000000000, 0.8660254037844387076, 1.000000000000000000, 0.8660254037844387076, 1.000000000000000000, 0.8660254037844387076, 1.000000000000000000, 0.8660254037844387076, 1.000000000000000000, 0.8660254037844387076, 1.000000000000000000, 0.8660254037844387076, 1.000000000000000000, 0.8660254037844387076, 1.000000000000000000, 0.8660254037844387076, 1.000000000000000000, 0.8660254037844387076, 1.000000000000000000, 0.8660254037844387076, 1.000000000000000000, 0.8660254037844387076, 1.000000000000000000, 0.8660254037844387076, 1.000000000000000000, 0.8660254037844387076, 1.000000000000000000, 0.8660254037844387076, 1.000000000000000000, 0.8660254037844387076, 1.000000000000000000, 0.8660254037844387076, 1.000000000000000000, 0.8660254037844387076, 1.000000000000000000, 0.8660254037844387076, 1.000000000000000000, 0.8660254037844387076, 1.000000000000000000, 0.8660254037844387076, 1.000000000000000000, 0.8660254037844387076, 1.000000000000000000, 0.8660254037844387076, 1.000000000000000000, 0.8660254037844387076, 1.000000000000000000, 0.8660254037844387076, 1.000000000000000000, 0.8660254037844387076, 1.000000000000000000, 0.8660254037844387076, 1.000000000000000000, 0.8660254037844387076, 1.000000000000000000, 0.8660254037844387076, 1.000000000000000000, 0.8660254037844387076, 1.000000000000000000, 0.8660254037844387076, 1.000000000000000000, 0.8660254037844387076, 1.000000000000000000, 0.8660254037844387076, 1.000000000000000000, 0.8660254037844387076, 1.000000000000000000, 0.8660254037844387076, 1.000000000000000000, 0.8660254037844387076, 1.000000000000000000, 0.8660254037844387076, 1.000000000000000000, 0.8660254037844387076, 1.000000000000000000, 0.8660254037844387076, 1.000000000000000000, 0.8660254037844387076, 1.000000000000000000, 0.8660254037844387076, 1.000000000000000000, 0.8660254037844387076, 1.000000000000000000, 0.8660254037844387076, 1.000000000000000000, 0.8660254037844387076, 1.000000000000000000, 0.8660254037844387076, 1.000000000000000000, 0.8660254037844387076, 1.000000000000000000, 0.8660254037844387076, 1.000000000000000000, 0.8660254037844387076, 1.000000000000000000, 0.8660254037844387076, 1.000000000000000000, 0.8660254037844387076, 1.000000000000000000, 0.8660254037844387076, 1.000000000000000000, 0.8660254037844387076, 1.000000000000000000, 0.8660254037844387076, 1.000000000000000000, 0.8660254037844387076, 1.000000000000000000, 0.8660254037844387076, 1.000000000000000000, 0.8660254037844387076, 1.000000000000000000, 0.8660254037844387076, 1.000000000000000000, 0.8660254037844387076, 1.000000000000000000, 0.8660254037844387076, 1.000000000000000000, 0.8660254037844387076, 1.000000000000000000, 0.8660254037844387076, 1.000000000000000000, 0.8660254037844387076, 1.000000000000000000, 0.8660254037844387076, 1.000000000000000000, 0.8660254037844387076, 1.000000000000000000, 0.8660254037844387076, 1.000000000000000000, 0.8660254037844387076, 1.000000000000000000, 0.8660254037844387076, 1.000000000000000000, 0.8660254037844387076, 1.000000000000000000, 0.8660254037844387076, 1.000000000000000000, 0.8660254037844387076, 1.000000000000000000, 0.8660254037844387076, 1.000000000000000000, 0.8660254037844387076, 1.000000000000000000, 0.8660254037844387076, 1.000000000000000000, 0.8660254037844387076, 1.000000000000000000, 0.8660254037844387076, 1.000000000000000000, 0.8660254037844387076, 1.000000000000000000, 0.8660254037844387076, 1.000000000000000000, 0.8660254037844387076, 1.000000000000000000, 0.8660254037844387076, 1.000000000000000000, 0.8660254037844387076, 1.000000000000000000, 0.8660254037844387076, 1.000000000000000000, 0.8660254037844387076, 1.000000000000000000, 0.8660254037844387076, 1.000000000000000000, 0.8660254037844387076, 1.000000000000000000, 0.8660254037844387076, 1.000000000000000000, 0.8660254037844387076, 1.000000000000000000, 0.8660254037844387076, 1.000000000000000000, 0.8660254037844387076, 1.000000000000000000, 0.8660254037844387076, 1.000000000000000000, 0.8660254037844387076, 1.000000000000000000, 0.8660254037844387076, 1.000000000000000000, 0.8660254037844387076, 1.000000000000000000, 0.8660254037844387076, 1.000000000000000000, 0.8660254037844387076, 1.000000000000000000, 0.8660254037844387076, 1.000000000000000000, 0.8660254037844387076, 1.000000000000000000, 0.8660254037844387076, 1.000000000000000000, 0.8660254037844387076, 1.000000000000000000, 0.8660254037844387076, 1.000000000000000000, 0.8660254037844387076, 1.000000000000000000, 0.8660254037844387076, 1.000000000000000000, 0.8660254037844387076, 1.000000000000000000, 0.8660254037844387076, 1.000000000000000000, 0.8660254037844387076, 1.000000000000000000, 0.8660254037844387076, 1.000000000000000000, 0.8660254037844387076, 1.000000000000000000, 0.8660254037844387076, 1.000000000000000000, 0.8660254037844387076, 1.000000000000000000, 0.8660254037844387076, 1.000000000000000000, 0.8660254037844387076, 1.000000000000000000, 0.8660254037844387076, 1.000000000000000000, 0.8660254037844387076, 1.000000000000000000, 0.8660254037844387076, 1.000000000000000000, 0.8660254037844387076, 1.000000000000000000, 0.8660254037844387076, 1.000000000000000000, 0.8660254037844387076, 1.000000000000000000, 0.8660254037844387076, 1.000000000000000000, 0.8660254037844387076, 1.000000000000000000, 0.8660254037844387076, 1.000000000000000000, 0.8660254037844387076, 1.000000000000000000, 0.8660254037844387076, 1.000000000000000000, 0.8660254037844387076, 1.000000000000000000, 0.8660254037844387076, 1.000000000000000000, 0.8660254037844387076, 1.000000000000000000, 0.8660254037844387076, 1.000000000000000000, 0.8660254037844387076, 1.000000000000000000, 0.8660254037844387076, 1.000000000000000000, 0.8660254037844387076, 1.000000000000000000, 0.8660254037844387076, 1.000000000000000000, 0.8660254037844387076, 1.000000000000000000, 0.8660254037844387076, 1.000000000000000000, 0.8660254037844387076, 1.000000000000000000, 0.8660254037844387076, 1.000000000000000000, 0.8660254037844387076, 1.000000000000000000, 0.8660254037844387076, 1.000000000000000000, 0.8660254037844387076, 1.000000000000000000, 0.8660254037844387076, 1.000000000000000000, 0.8660254037844387076, 1.000000000000000000, 0.8660254037844387076, 1.000000000000000000, 0.8660254037844387076, 1.000000000000000000, 0.8660254037844387076, 1.000000000000000000, 0.8660254037844387076, 1.000000000000000000, 0.8660254037844387076, 1.000000000000000000, 0.8660254037844387076, 1.000000000000000000, 0.8660254037844387076, 1.000000000000000000, 0.8660254037844387076, 1.000000000000000000, 0.8660254037844387076, 1.000000000000000000, 0.8660254037844387076, 1.000000000000000000, 0.8660254037844387076, 1.000000000000000000, 0.8660254037844387076, 1.000000000000000000, 0.8660254037844387076, 1.000000000000000000, 0.8660254037844387076, 1.000000000000000000, 0.8660254037844387076, 1.000000000000000000, 0.8660254037844387076, 1.000000000000000000, 0.8660254037844387076, 1.000000000000000000, 0.8660254037844387076, 1.000000000000000000, 0.8660254037844387076, 1.000000000000000000, 0.8660254037844387076, 1.000000000000000000, 0.8660254037844387076, 1.000000000000000000, 0.8660254037844387076, 1.000000000000000000, 0.8660254037844387076, 1.000000000000000000, 0.8660254037844387076, 1.000000000000000000, 0.8660254037844387076, 1.000000000000000000, 0.8660254037844387076, 1.000000000000000000, 0.8660254037844387076, 1.000000000000000000, 0.8660254037844387076, 1.000000000000000000, 0.8660254037844387076, 1.000000000000000000, 0.8660254037844387076, 1.000000000000000000, 0.8660254037844387076, 1.000000000000000000, 0.8660254037844387076, 1.000000000000000000, 0.8660254037844387076, 1.000000000000000000, 0.8660254037844387076, 1.000000000000000000, 0.8660254037844387076, 1.000000000000000000, 0.8660254037844387076, 1.000000000000000000, 0.8660254037844387076, 1.000000000000000000, 0.8660254037844387076, 1.000000000000000000, 0.8660254037844387076, 1.000000000000000000, 0.8660254037844387076, 1.000000000000000000, 0.8660254037844387076, 1.000000000000000000, 0.8660254037844387076, 1.000000000000000000, 0.8660254037844387076, 1.000000000000000000, 0.8660254037844387076, 1.000000000000000000, 0.8660254037844387076, 1.000000000000000000, 0.8660254037844387076, 1.000000000000000000, 0.8660254037844387076, 1.000000000000000000, 0.8660254037844387076, 1.000000000000000000, 0.8660254037844387076, 1.000000000000000000, 0.8660254037844387076, 1.000000000000000000, 0.8660254037844387076, 1.000000000000000000, 0.8660254037844387076, 1.000000000000000000, 0.8660254037844387076, 1.000000000000000000, 0.8660254037844387076, 1.000000000000000000, 0.8660254037844387076, 1.000000000000000000, 0.8660254037844387076, 1.000000000000000000, 0.8660254037844387076, 1.000000000000000000, 0.8660254037844387076, 1.000000000000000000, 0.8660254037844387076, 1.000000000000000000, 0.8660254037844387076, 1.000000000000000000, 0.8660254037844387076, 1.000000000000000000, 0.8660254037844387076, 1.000000000000000000, 0.8660254037844387076, 1.000000000000000000, 0.8660254037844387076, 1.000000000000000000, 0.8660254037844387076, 1.000000000000000000, 0.8660254037844387076, 1.000000000000000000, 0.8660254037844387076, 1.000000000000000000, 0.8660254037844387076, 1.000000000000000000, 0.8660254037844387076, 1.000000000000000000, 0.8660254037844387076, 1.000000000000000000, 0.8660254037844387076, 1.000000000000000000, 0.8660254037844387076, 1.000000000000000000, 0.8660254037844387076, 1.000000000000000000, 0.8660254037844387076, 1.000000000000000000, 0.8660254037844387076, 1.000000000000000000, 0.8660254037844387076, 1.000000000000000000, 0.8660254037844387076, 1.000000000000000000, 0.8660254037844387076, 1.000000000000000000, 0.8660254037844387076, 1.000000000000000000, 0.8660254037844387076, 1.000000000000000000, 0.8660254037844387076, 1.000000000000000000) ) ) 
 REPRESENTATION_ITEM ( '' )  SURFACE ( )  );
#61799 = CARTESIAN_POINT ( 'NONE',  ( 27.90000000122903145, -2.886751345948129988, 4.999999999999997335 ) ) ;
#61800 = CARTESIAN_POINT ( 'NONE',  ( 24.42187500061451644, 2.746126346562643317, 4.756430356249998326 ) ) ;
#61801 = CARTESIAN_POINT ( 'NONE',  ( 18.92812500061451431, 4.541064518000418104, 2.621784821874999949 ) ) ;
#61802 = CARTESIAN_POINT ( 'NONE',  ( 1.626862140677534273E-15, 13.81250000000000000, 34.00000000000000000 ) ) ;
#61803 = CARTESIAN_POINT ( 'NONE',  ( 3.756430356250000546, 17.62812499938548427, 27.83122392262697886 ) ) ;
#61804 = CARTESIAN_POINT ( 'NONE',  ( 13.17187500061451999, 3.027376345333611329, 5.243569643749999010 ) ) ;
#61805 = CARTESIAN_POINT ( 'NONE',  ( 14.52187500061451608, 3.027376345333611329, 5.243569643749999010 ) ) ;
#61806 = CARTESIAN_POINT ( 'NONE',  ( 22.95937500061451431, 4.541064518000418104, -2.621784821874998173 ) ) ;
#61807 = ORIENTED_EDGE ( 'NONE', *, *, #15786, .F. ) ;
#61808 = CARTESIAN_POINT ( 'NONE',  ( 19.94999999999999929, 4.330127018922192761, -2.499999999999997780 ) ) ;
#61810 =( BOUNDED_CURVE ( )  B_SPLINE_CURVE ( 2, ( #72785, #62415, #56864, #33973, #62058, #62777, #5184, #68335, #27722 ),
 .UNSPECIFIED., .F., .F. ) 
 B_SPLINE_CURVE_WITH_KNOTS ( ( 3, 2, 2, 2, 3 ),
 ( 0.7282608695652174058, 0.7318840579710145233, 0.7391304347826086474, 0.7463768115942028825, 0.7500000000000000000 ),
 .UNSPECIFIED. ) 
 CURVE ( )  GEOMETRIC_REPRESENTATION_ITEM ( )  RATIONAL_B_SPLINE_CURVE ( ( 0.9330127018922194093, 0.9330127018922194093, 1.000000000000000000, 0.8660254037844387076, 1.000000000000000000, 0.8660254037844387076, 1.000000000000000000, 0.9330127018922194093, 0.9330127018922194093 ) ) 
 REPRESENTATION_ITEM ( '' )  );
#61809 = CARTESIAN_POINT ( 'NONE',  ( 25.97812500061451502, 6.421520780324663323E-16, -5.243569643749999010 ) ) ;
#61811 = CARTESIAN_POINT ( 'NONE',  ( 26.76562500061451644, -6.054752690667223547, -1.112240025338166033E-15 ) ) ;
#61812 = CYLINDRICAL_SURFACE ( 'NONE', #56839, 4.999999999999998224 ) ;
#61813 = CARTESIAN_POINT ( 'NONE',  ( -3.999999999999997335, 16.88749999999999929, 32.30940107675850470 ) ) ;
#61814 = CARTESIAN_POINT ( 'NONE',  ( 4.096875000614518925, 6.054752690667223547, 3.707466751127219781E-16 ) ) ;
#61815 = CARTESIAN_POINT ( 'NONE',  ( 11.88750000122903216, 6.123233995736764310E-16, -4.999999999999998224 ) ) ;
#61816 = CARTESIAN_POINT ( 'NONE',  ( 7.275000001229035007, -5.773502691896255534, -1.060575238724906372E-15 ) ) ;
#61817 = CARTESIAN_POINT ( 'NONE',  ( 3.028125000614518392, 6.421520780324663323E-16, -5.243569643749999010 ) ) ;
#61818 = CARTESIAN_POINT ( 'NONE',  ( -3.999999999999999556, 18.03124999877096712, 27.69059892324149175 ) ) ;
#61819 = CARTESIAN_POINT ( 'NONE',  ( 18.20625000122903003, 4.330127018922192761, -2.499999999999997780 ) ) ;
#61820 = CARTESIAN_POINT ( 'NONE',  ( 11.29687500061451644, 6.054752690667223547, 3.707466751127219781E-16 ) ) ;
#61821 = CARTESIAN_POINT ( 'NONE',  ( 3.999999999999999112, 14.82500000000000107, -30.00000000000000000 ) ) ;
#61822 = ORIENTED_EDGE ( 'NONE', *, *, #69469, .T. ) ;
#61823 = CARTESIAN_POINT ( 'NONE',  ( 19.04062500061451146, -3.027376345333614438, 5.243569643749998122 ) ) ;
#61824 = CARTESIAN_POINT ( 'NONE',  ( 14.22187500061451537, -6.054752690667223547, -1.112240025338166033E-15 ) ) ;
#61825 = CARTESIAN_POINT ( 'NONE',  ( 4.790625000614518569, -3.027376345333610441, -5.243569643749999898 ) ) ;
#61826 = CARTESIAN_POINT ( 'NONE',  ( 21.94687500061451502, -3.027376345333610441, -5.243569643749999898 ) ) ;
#61827 = CARTESIAN_POINT ( 'NONE',  ( 9.121875000614517504, 3.027376345333611329, 5.243569643749999010 ) ) ;
#61828 = CARTESIAN_POINT ( 'NONE',  ( 5.353125000614515905, 4.541064518000418104, -2.621784821874998173 ) ) ;
#61829 = CARTESIAN_POINT ( 'NONE',  ( -1.999999999999997113, 17.82499999999999929, 33.46410161513775705 ) ) ;
#61830 = CARTESIAN_POINT ( 'NONE',  ( 6.412500001229036073, -4.330127018922190985, -2.500000000000001332 ) ) ;
#61831 = CARTESIAN_POINT ( 'NONE',  ( 18.92812500061451431, 4.541064518000418104, 2.621784821874999949 ) ) ;
#61832 =( BOUNDED_CURVE ( )  B_SPLINE_CURVE ( 2, ( #42249, #35970, #7534, #14528, #70682, #59219, #7900, #41881, #64409 ),
 .UNSPECIFIED., .F., .F. ) 
 B_SPLINE_CURVE_WITH_KNOTS ( ( 3, 2, 2, 2, 3 ),
 ( 0.09782608695652174335, 0.1014492753623188470, 0.1086956521739130405, 0.1159420289855072478, 0.1195652173913043514 ),
 .UNSPECIFIED. ) 
 CURVE ( )  GEOMETRIC_REPRESENTATION_ITEM ( )  RATIONAL_B_SPLINE_CURVE ( ( 0.9330127018922194093, 0.9330127018922194093, 1.000000000000000000, 0.8660254037844387076, 1.000000000000000000, 0.8660254037844387076, 1.000000000000000000, 0.9330127018922194093, 0.9330127018922194093 ) ) 
 REPRESENTATION_ITEM ( '' )  );
#61833 = CARTESIAN_POINT ( 'NONE',  ( 8.475000001229034297, 2.886751345948126879, 4.999999999999999112 ) ) ;
#61834 = CARTESIAN_POINT ( 'NONE',  ( 17.20312500061451644, 0.000000000000000000, 5.243569643749999010 ) ) ;
#61835 = CARTESIAN_POINT ( 'NONE',  ( 14.72812500061451679, 6.421520780324663323E-16, -5.243569643749999010 ) ) ;
#61836 = CARTESIAN_POINT ( 'NONE',  ( 25.99687500061451928, -2.746126346562642428, -4.756430356249999214 ) ) ;
#61837 = CARTESIAN_POINT ( 'NONE',  ( 16.16250000000000142, -5.773502691896255534, -1.060575238724906372E-15 ) ) ;
#61838 = CARTESIAN_POINT ( 'NONE',  ( 9.450000001229033941, -2.886751345948129988, 4.999999999999997335 ) ) ;
#61839 = CARTESIAN_POINT ( 'NONE',  ( 5.465625000614517504, 3.027376345333611329, 5.243569643749999010 ) ) ;
#61840 = EDGE_CURVE ( 'NONE', #55166, #48472, #26534, .T. ) ;
#61841 = CARTESIAN_POINT ( 'NONE',  ( 21.52500000122903145, 2.886751345948126879, 4.999999999999999112 ) ) ;
#61842 = CARTESIAN_POINT ( 'NONE',  ( 26.77499999999999858, 4.330127018922191873, 2.499999999999999556 ) ) ;
#61843 = CARTESIAN_POINT ( 'NONE',  ( 4.243569643749999898, 10.63437500061451857, -30.00000000000000000 ) ) ;
#61844 = CARTESIAN_POINT ( 'NONE',  ( 4.575021196052274419, -2.017510855256722468, 4.733783051837803235 ) ) ;
#61845 = CARTESIAN_POINT ( 'NONE',  ( 23.92499999999999716, 6.123233995736764310E-16, -4.999999999999998224 ) ) ;
#61846 = CARTESIAN_POINT ( 'NONE',  ( 4.434375000614519280, 6.421520780324663323E-16, -5.243569643749999010 ) ) ;
#61847 = CARTESIAN_POINT ( 'NONE',  ( 21.87187500061451573, -6.054752690667223547, -1.112240025338166033E-15 ) ) ;
#61848 = DIRECTION ( 'NONE',  ( -0.000000000000000000, -0.000000000000000000, -1.000000000000000000 ) ) ;
#61849 = CARTESIAN_POINT ( 'NONE',  ( 17.27812500061451217, -4.541064518000419881, 2.621784821874995952 ) ) ;
#61850 = CARTESIAN_POINT ( 'NONE',  ( 12.69375000122903430, -2.886751345948125991, -5.000000000000000000 ) ) ;
#61851 = CARTESIAN_POINT ( 'NONE',  ( 26.73749999999999716, 5.773502691896255534, 3.535250795749688401E-16 ) ) ;
#61852 = CARTESIAN_POINT ( 'NONE',  ( 27.94687500061451502, 6.054752690667223547, 3.707466751127219781E-16 ) ) ;
#61853 = CARTESIAN_POINT ( 'NONE',  ( 19.95937500061451786, -5.492252693125287522, -1.008910452111647106E-15 ) ) ;
#61854 = AXIS2_PLACEMENT_3D ( 'NONE', #52393, #12862, #23942 ) ;
#61855 = CARTESIAN_POINT ( 'NONE',  ( 12.66562500061451502, 3.027376345333611329, 5.243569643749999010 ) ) ;
#61856 = CARTESIAN_POINT ( 'NONE',  ( 10.17187500061451999, -6.054752690667223547, -1.112240025338166033E-15 ) ) ;
#61857 = ORIENTED_EDGE ( 'NONE', *, *, #6767, .F. ) ;
#61858 = CARTESIAN_POINT ( 'NONE',  ( 2.817472997146174052, -4.130598735093008678, -2.817472997146206026 ) ) ;
#61859 = CARTESIAN_POINT ( 'NONE',  ( 23.05312500061451431, 0.000000000000000000, 5.243569643749999010 ) ) ;
#61860 = CYLINDRICAL_SURFACE ( 'NONE', #339, 4.999999999999998224 ) ;
#61861 = CARTESIAN_POINT ( 'NONE',  ( -5.810221930991193690E-16, 14.93750000000000000, 26.00000000000000355 ) ) ;
#61862 = VECTOR ( 'NONE', #32146, 1000.000000000000000 ) ;
#61863 = CARTESIAN_POINT ( 'NONE',  ( 13.04999999999999893, -4.330127018922190985, -2.500000000000001332 ) ) ;
#61864 = CARTESIAN_POINT ( 'NONE',  ( 20.85000000122903430, -2.886751345948125991, -5.000000000000000000 ) ) ;
#61865 = CARTESIAN_POINT ( 'NONE',  ( 16.45312500061451289, -4.541064518000417216, -2.621784821875001281 ) ) ;
#61866 = CARTESIAN_POINT ( 'NONE',  ( 12.23437500061451644, -2.746126346562646425, 4.756430356249996549 ) ) ;
#61867 = EDGE_LOOP ( 'NONE', ( #15612, #56765, #25707, #72239 ) ) ;
#61868 = CARTESIAN_POINT ( 'NONE',  ( 18.82500000000000284, -4.330127018922194537, 2.499999999999995559 ) ) ;
#61869 = CARTESIAN_POINT ( 'NONE',  ( 24.89999999999999858, 4.330127018922192761, -2.499999999999997780 ) ) ;
#61870 = CARTESIAN_POINT ( 'NONE',  ( 21.87187500061451573, -6.054752690667223547, -1.112240025338166033E-15 ) ) ;
#61871 = CARTESIAN_POINT ( 'NONE',  ( 24.55312500061451786, -4.541064518000417216, -2.621784821875001281 ) ) ;
#61873 = ORIENTED_EDGE ( 'NONE', *, *, #2515, .F. ) ;
#61872 = VECTOR ( 'NONE', #57770, 1000.000000000000000 ) ;
#61874 = CARTESIAN_POINT ( 'NONE',  ( 19.16250000000000142, 2.886751345948098901, 5.000000000000047073 ) ) ;
#61875 = CARTESIAN_POINT ( 'NONE',  ( 8.053125000614516082, 4.541064518000418104, -2.621784821874998173 ) ) ;
#61876 = CARTESIAN_POINT ( 'NONE',  ( 17.43750000122903288, 4.330127018922191873, 2.499999999999999556 ) ) ;
#61877 = CARTESIAN_POINT ( 'NONE',  ( 15.52500000000000036, 4.330127018922191873, 2.499999999999999556 ) ) ;
#61878 = CARTESIAN_POINT ( 'NONE',  ( 3.598985740823767987, -3.471053988920652422, -3.649034764177215173 ) ) ;
#61879 = CARTESIAN_POINT ( 'NONE',  ( 4.884375000614518569, 6.421520780324663323E-16, -5.243569643749999010 ) ) ;
#61880 = VECTOR ( 'NONE', #58739, 1000.000000000000000 ) ;
#61881 = CARTESIAN_POINT ( 'NONE',  ( 28.47187500061451715, 3.027376345333611329, 5.243569643749999010 ) ) ;
#61882 = ORIENTED_EDGE ( 'NONE', *, *, #45500, .T. ) ;
#61883 = CARTESIAN_POINT ( 'NONE',  ( 24.92812500061451431, -4.541064518000419881, 2.621784821874995952 ) ) ;
#61884 = CARTESIAN_POINT ( 'NONE',  ( 25.80937500061451928, 0.000000000000000000, 5.243569643749999010 ) ) ;
#61885 = EDGE_CURVE ( 'NONE', #23724, #70091, #27683, .T. ) ;
#61886 = CARTESIAN_POINT ( 'NONE',  ( 2.121784821875001281, 18.15312500061459389, -26.32496088578401938 ) ) ;
#61887 = CARTESIAN_POINT ( 'NONE',  ( 11.17500000000000071, -4.330127018922194537, 2.499999999999995559 ) ) ;
#61888 = CARTESIAN_POINT ( 'NONE',  ( 10.00312500061451715, 0.000000000000000000, 5.243569643749999010 ) ) ;
#61889 = CARTESIAN_POINT ( 'NONE',  ( 0.6945846161026939525, 20.50052346155192140, 33.93923243933046763 ) ) ;
#61890 = CARTESIAN_POINT ( 'NONE',  ( 1.510657702057710734E-15, 19.43750000000000000, -33.99999999999999289 ) ) ;
#61891 = CARTESIAN_POINT ( 'NONE',  ( 26.72812500061451502, -4.541064518000419881, 2.621784821874995952 ) ) ;
#61892 = CARTESIAN_POINT ( 'NONE',  ( 29.70937500061451431, 2.746126346562643317, 4.756430356249998326 ) ) ;
#61893 = CARTESIAN_POINT ( 'NONE',  ( 12.08437500061451608, 5.824947211148865298E-16, -4.756430356249998326 ) ) ;
#61894 = CARTESIAN_POINT ( 'NONE',  ( 3.178125000614515638, 4.541064518000418104, 2.621784821874999949 ) ) ;
#61895 = CARTESIAN_POINT ( 'NONE',  ( 19.35937500061451644, 4.541064518000418104, -2.621784821874998173 ) ) ;
#61896 = CARTESIAN_POINT ( 'NONE',  ( 2.121784821874999061, 15.65937500061451892, 26.32496088578401583 ) ) ;
#61897 = CARTESIAN_POINT ( 'NONE',  ( 20.93437500061451573, -4.541064518000419881, 2.621784821874995952 ) ) ;
#61898 = CARTESIAN_POINT ( 'NONE',  ( 28.99687500061451573, -3.027376345333614438, 5.243569643749998122 ) ) ;
#61899 = CARTESIAN_POINT ( 'NONE',  ( 4.243569643749999010, 18.77187500061451431, 27.54997392385601174 ) ) ;
#61900 = CARTESIAN_POINT ( 'NONE',  ( 10.86562500061451431, 3.027376345333611329, 5.243569643749999010 ) ) ;
#61901 = CARTESIAN_POINT ( 'NONE',  ( 2.700000001229035718, -2.886751345948129988, 4.999999999999997335 ) ) ;
#61902 = CARTESIAN_POINT ( 'NONE',  ( 5.971875000614516260, 3.027376345333611329, 5.243569643749999010 ) ) ;
#61903 = CARTESIAN_POINT ( 'NONE',  ( -1.071796769724488563, 16.15490381179669654, -26.00000000000000000 ) ) ;
#61904 = CARTESIAN_POINT ( 'NONE',  ( 6.628125000614517148, 6.421520780324663323E-16, -5.243569643749999010 ) ) ;
#61905 = CARTESIAN_POINT ( 'NONE',  ( 12.38437500061451857, -4.541064518000419881, 2.621784821874995952 ) ) ;
#61906 = SURFACE_STYLE_USAGE ( .BOTH. , #10941 ) ;
#61907 = CARTESIAN_POINT ( 'NONE',  ( 19.68750000122903288, 4.330127018922191873, 2.499999999999999556 ) ) ;
#61908 = CARTESIAN_POINT ( 'NONE',  ( 7.134375000614516793, 6.421520780324663323E-16, -5.243569643749999010 ) ) ;
#61909 = CARTESIAN_POINT ( 'NONE',  ( 9.253125000614517148, -4.541064518000417216, -2.621784821875001281 ) ) ;
#61910 = DIRECTION ( 'NONE',  ( 0.000000000000000000, 0.000000000000000000, 1.000000000000000000 ) ) ;
#61911 = CARTESIAN_POINT ( 'NONE',  ( 26.64375000122903003, -2.886751345948125991, -5.000000000000000000 ) ) ;
#61912 = CARTESIAN_POINT ( 'NONE',  ( 18.08437500061451431, 4.541064518000418104, 2.621784821874999949 ) ) ;
#61913 = CARTESIAN_POINT ( 'NONE',  ( 1.071796769724489895, 13.22990381179669939, 26.00000000000000355 ) ) ;
#61914 = CARTESIAN_POINT ( 'NONE',  ( 27.62812500061451360, -4.541064518000419881, 2.621784821874995952 ) ) ;
#61915 = CARTESIAN_POINT ( 'NONE',  ( 13.11562500061451786, 3.027376345333611329, 5.243569643749999010 ) ) ;
#61916 = LINE ( 'NONE', #22393, #64345 ) ;
#61917 = CARTESIAN_POINT ( 'NONE',  ( -4.243569643749998122, 11.79687500061451999, -27.54997392385601174 ) ) ;
#61918 = CARTESIAN_POINT ( 'NONE',  ( 13.05000000122903536, -2.886751345948129988, 4.999999999999997335 ) ) ;
#61919 = CARTESIAN_POINT ( 'NONE',  ( 28.45312500061451289, 0.000000000000000000, 5.243569643749999010 ) ) ;
#61920 = CARTESIAN_POINT ( 'NONE',  ( 9.001249775931846008E-16, 16.31562500061451715, -25.09994784771203058 ) ) ;
#61921 = CARTESIAN_POINT ( 'NONE',  ( 14.02500000122903323, -5.773502691896255534, -1.060575238724906372E-15 ) ) ;
#61922 = AXIS2_PLACEMENT_3D ( 'NONE', #55587, #56315, #62215 ) ;
#61923 = CARTESIAN_POINT ( 'NONE',  ( 12.90000000000000213, 0.000000000000000000, 4.999999999999998224 ) ) ;
#61924 = CARTESIAN_POINT ( 'NONE',  ( 4.311958327294343363, 2.531208285321026263, 4.311958327294242999 ) ) ;
#61925 = CARTESIAN_POINT ( 'NONE',  ( 21.89062500061451289, -3.027376345333610441, -5.243569643749999898 ) ) ;
#61926 = CARTESIAN_POINT ( 'NONE',  ( 8.446875000614518569, -3.027376345333610441, -5.243569643749999898 ) ) ;
#61927 = CARTESIAN_POINT ( 'NONE',  ( 8.512500001229033941, 0.000000000000000000, 4.999999999999998224 ) ) ;
#61928 = ADVANCED_FACE ( 'NONE', ( #23761 ), #8238, .T. ) ;
#61929 = CARTESIAN_POINT ( 'NONE',  ( 16.20000000122903216, -2.886751345948129988, 4.999999999999997335 ) ) ;
#61930 = CARTESIAN_POINT ( 'NONE',  ( 12.89062500061451821, -3.027376345333610441, -5.243569643749999898 ) ) ;
#61931 = CARTESIAN_POINT ( 'NONE',  ( 17.50312500061451715, 4.541064518000418104, -2.621784821874998173 ) ) ;
#61932 = ADVANCED_FACE ( 'NONE', ( #63291 ), #13041, .T. ) ;
#61933 = CIRCLE ( 'NONE', #5309, 9.999999999999998224 ) ;
#61934 = CARTESIAN_POINT ( 'NONE',  ( 28.23750000122903359, 4.330127018922191873, 2.499999999999999556 ) ) ;
#61935 = CARTESIAN_POINT ( 'NONE',  ( 23.09999999999999787, 4.330127018922192761, -2.499999999999997780 ) ) ;
#61936 = VECTOR ( 'NONE', #40152, 1000.000000000000000 ) ;
#61937 = CARTESIAN_POINT ( 'NONE',  ( 23.48437500061451644, 4.541064518000418104, 2.621784821874999949 ) ) ;
#61938 = DIRECTION ( 'NONE',  ( -1.000000000000000000, -0.000000000000000000, -0.000000000000000000 ) ) ;
#61939 = CARTESIAN_POINT ( 'NONE',  ( 9.750000001229032875, 5.773502691896255534, 3.535250795749688894E-16 ) ) ;
#61940 = CARTESIAN_POINT ( 'NONE',  ( 28.20937500061451786, -4.541064518000417216, -2.621784821875001281 ) ) ;
#61941 = CARTESIAN_POINT ( 'NONE',  ( 4.996875000614516615, 6.054752690667223547, 3.707466751127219781E-16 ) ) ;
#61942 = CARTESIAN_POINT ( 'NONE',  ( 24.25312500061451715, 4.541064518000418104, -2.621784821874998173 ) ) ;
#61943 = CARTESIAN_POINT ( 'NONE',  ( 3.756430356249998770, 14.51562499938548356, 32.16877607737301759 ) ) ;
#61944 = CARTESIAN_POINT ( 'NONE',  ( 9.384375000614518569, 6.421520780324663323E-16, -5.243569643749999010 ) ) ;
#61945 = DIRECTION ( 'NONE',  ( -1.000000000000000000, -0.000000000000000000, 0.000000000000000000 ) ) ;
#61946 = CARTESIAN_POINT ( 'NONE',  ( 29.12812500061451715, 6.421520780324663323E-16, -5.243569643749999010 ) ) ;
#61947 = CARTESIAN_POINT ( 'NONE',  ( 6.159375000614517148, -4.541064518000417216, -2.621784821875001281 ) ) ;
#61948 = CARTESIAN_POINT ( 'NONE',  ( 25.87500000000000000, 4.330127018922191873, 2.499999999999999556 ) ) ;
#61949 = CARTESIAN_POINT ( 'NONE',  ( 27.90937500061451715, 4.541064518000418104, -2.621784821874998173 ) ) ;
#61950 = CARTESIAN_POINT ( 'NONE',  ( 27.80625000122903145, 0.000000000000000000, 4.999999999999998224 ) ) ;
#61951 = CARTESIAN_POINT ( 'NONE',  ( 20.62499999999999645, -4.330127018922194537, 2.499999999999995559 ) ) ;
#61952 = ORIENTED_EDGE ( 'NONE', *, *, #26233, .F. ) ;
#61953 = CARTESIAN_POINT ( 'NONE',  ( 26.81250000000000000, 2.886751345948126879, 4.999999999999999112 ) ) ;
#61954 = CARTESIAN_POINT ( 'NONE',  ( 29.48437500061451644, -4.541064518000419881, 2.621784821874995952 ) ) ;
#61955 = VERTEX_POINT ( 'NONE', #64380 ) ;
#61956 = CARTESIAN_POINT ( 'NONE',  ( 15.29062500061451679, 6.054752690667223547, 3.707466751127219781E-16 ) ) ;
#61957 = CARTESIAN_POINT ( 'NONE',  ( 9.478125000614515017, 4.541064518000418104, 2.621784821874999949 ) ) ;
#61958 = CARTESIAN_POINT ( 'NONE',  ( 19.99687500061451217, -4.119189519843965641, -2.378215178125001383 ) ) ;
#61959 = CARTESIAN_POINT ( 'NONE',  ( 4.021875000614516082, 3.027376345333613106, -5.243569643749998122 ) ) ;
#61960 = CARTESIAN_POINT ( 'NONE',  ( 18.07500000122903216, -5.773502691896255534, -1.060575238724906372E-15 ) ) ;
#61961 = VECTOR ( 'NONE', #25648, 1000.000000000000000 ) ;
#61962 = CARTESIAN_POINT ( 'NONE',  ( 25.34999999999999787, 4.330127018922192761, -2.499999999999997780 ) ) ;
#61963 = CARTESIAN_POINT ( 'NONE',  ( 23.88750000122903216, -4.330127018922194537, 2.499999999999995559 ) ) ;
#61964 = CARTESIAN_POINT ( 'NONE',  ( 8.034375000614518925, 6.421520780324663323E-16, -5.243569643749999010 ) ) ;
#61965 = CARTESIAN_POINT ( 'NONE',  ( 12.08437500061451608, 6.421520780324663323E-16, -5.243569643749999010 ) ) ;
#61966 = CARTESIAN_POINT ( 'NONE',  ( 22.65937500061451715, 0.000000000000000000, 5.243569643749999010 ) ) ;
#61967 = DIRECTION ( 'NONE',  ( 0.000000000000000000, 0.000000000000000000, -1.000000000000000000 ) ) ;
#61968 = VERTEX_POINT ( 'NONE', #12684 ) ;
#61969 = CARTESIAN_POINT ( 'NONE',  ( 4.171875000614517326, 3.027376345333611329, 5.243569643749999010 ) ) ;
#61970 = CARTESIAN_POINT ( 'NONE',  ( 7.809375000614519280, 0.000000000000000000, 5.243569643749999010 ) ) ;
#61971 = CARTESIAN_POINT ( 'NONE',  ( 19.72499999999999787, -4.330127018922194537, 2.499999999999995559 ) ) ;
#61972 = CARTESIAN_POINT ( 'NONE',  ( 17.05312500061451786, 4.541064518000418104, -2.621784821874998173 ) ) ;
#61973 = CARTESIAN_POINT ( 'NONE',  ( 4.000000000000000000, 18.38749999999999929, 27.69059892324149530 ) ) ;
#61974 = DIRECTION ( 'NONE',  ( 0.000000000000000000, 0.000000000000000000, -1.000000000000000000 ) ) ;
#61975 = CARTESIAN_POINT ( 'NONE',  ( 21.49687500061451573, -2.746126346562642428, -4.756430356249999214 ) ) ;
#61976 = CARTESIAN_POINT ( 'NONE',  ( 9.103125000614515017, 0.000000000000000000, 5.243569643749999010 ) ) ;
#61977 = CARTESIAN_POINT ( 'NONE',  ( 27.27187500061451431, -6.054752690667223547, -1.112240025338166033E-15 ) ) ;
#61978 = CARTESIAN_POINT ( 'NONE',  ( 20.24999999999999645, -4.330127018922190985, -2.500000000000001332 ) ) ;
#61979 = CARTESIAN_POINT ( 'NONE',  ( 28.73437500061451644, 6.421520780324663323E-16, -5.243569643749999010 ) ) ;
#61980 = CARTESIAN_POINT ( 'NONE',  ( 8.962500000000002132, -5.773502691896255534, -1.060575238724906372E-15 ) ) ;
#61981 = CARTESIAN_POINT ( 'NONE',  ( 8.484601909799253346E-16, 15.27500000122903501, 34.61880215351700230 ) ) ;
#61982 = CARTESIAN_POINT ( 'NONE',  ( 10.23750000122903359, 4.330127018922191873, 2.499999999999999556 ) ) ;
#61983 = AXIS2_PLACEMENT_3D ( 'NONE', #53038, #47870, #25700 ) ;
#61984 = CARTESIAN_POINT ( 'NONE',  ( 18.90937500061451360, 4.541064518000418104, -2.621784821874998173 ) ) ;
#61985 = CARTESIAN_POINT ( 'NONE',  ( 13.88437500061451679, 6.421520780324663323E-16, -5.243569643749999010 ) ) ;
#61986 = CARTESIAN_POINT ( 'NONE',  ( -1.351880753582010319, 4.820610340066096455, -33.77395916724246661 ) ) ;
#61987 = ORIENTED_EDGE ( 'NONE', *, *, #28959, .T. ) ;
#61988 = CARTESIAN_POINT ( 'NONE',  ( 15.55312500061451608, -4.541064518000417216, -2.621784821875001281 ) ) ;
#61989 = AXIS2_PLACEMENT_3D ( 'NONE', #60675, #26720, #36690 ) ;
#61990 = CARTESIAN_POINT ( 'NONE',  ( 26.36250000122903003, 4.330127018922192761, -2.499999999999997780 ) ) ;
#61991 = CARTESIAN_POINT ( 'NONE',  ( 15.12187500061451750, -6.054752690667223547, -1.112240025338166033E-15 ) ) ;
#61992 = CARTESIAN_POINT ( 'NONE',  ( 0.4052273161492611075, 10.00000000000000178, -23.99999999999999645 ) ) ;
#61993 = CARTESIAN_POINT ( 'NONE',  ( 17.99062500061451786, 6.054752690667223547, 3.707466751127219781E-16 ) ) ;
#61994 = LINE ( 'NONE', #11394, #68084 ) ;
#61995 = CARTESIAN_POINT ( 'NONE',  ( 25.58437500061451431, 6.421520780324663323E-16, -5.243569643749999010 ) ) ;
#61996 = CARTESIAN_POINT ( 'NONE',  ( -4.243569643749999898, 9.865625000614517859, 27.54997392385601529 ) ) ;
#61997 = CARTESIAN_POINT ( 'NONE',  ( 15.00937500061451679, 0.000000000000000000, 5.243569643749999010 ) ) ;
#61998 = CARTESIAN_POINT ( 'NONE',  ( 13.76250000122903394, 4.330127018922192761, -2.499999999999997780 ) ) ;
#61999 = CARTESIAN_POINT ( 'NONE',  ( 7.621875000614519280, 2.746126346562645981, -4.756430356249997438 ) ) ;
#62000 = CARTESIAN_POINT ( 'NONE',  ( 2.121784821875001281, 19.10937500061451644, -26.32496088578401938 ) ) ;
#62001 = CARTESIAN_POINT ( 'NONE',  ( 17.07187500061451502, 3.027376345333613106, -5.243569643749998122 ) ) ;
#62002 = CARTESIAN_POINT ( 'NONE',  ( 19.72500000122903074, 2.886751345948126879, 4.999999999999999112 ) ) ;
#62003 = CARTESIAN_POINT ( 'NONE',  ( 15.42187500061451821, 3.027376345333611329, 5.243569643749999010 ) ) ;
#62004 = ADVANCED_FACE ( 'NONE', ( #30768 ), #13393, .F. ) ;
#62005 = CARTESIAN_POINT ( 'NONE',  ( -2.121784821874996840, 12.73437500061451821, 33.67503911421598417 ) ) ;
#62006 = CARTESIAN_POINT ( 'NONE',  ( 21.56250000122903288, 0.000000000000000000, 4.999999999999998224 ) ) ;
#62007 = CARTESIAN_POINT ( 'NONE',  ( 15.14062500061451644, -3.027376345333610441, -5.243569643749999898 ) ) ;
#62008 = VERTEX_POINT ( 'NONE', #18575 ) ;
#62009 = ORIENTED_EDGE ( 'NONE', *, *, #11874, .F. ) ;
#62010 = CARTESIAN_POINT ( 'NONE',  ( 20.06250000000000000, 2.886751345948126879, 4.999999999999999112 ) ) ;
#62011 = CARTESIAN_POINT ( 'NONE',  ( 0.000000000000000000, 27.50000000000000000, 30.00000000000000000 ) ) ;
#62012 = CARTESIAN_POINT ( 'NONE',  ( 21.59062500061451928, 6.054752690667223547, 3.707466751127219781E-16 ) ) ;
#62013 = CARTESIAN_POINT ( 'NONE',  ( 2.878125000614517592, -4.541064518000419881, 2.621784821874995952 ) ) ;
#62014 = CARTESIAN_POINT ( 'NONE',  ( 13.83750000122903323, 4.330127018922191873, 2.499999999999999556 ) ) ;
#62015 = CARTESIAN_POINT ( 'NONE',  ( 18.96562500061451573, 3.027376345333611329, 5.243569643749999010 ) ) ;
#62016 = CARTESIAN_POINT ( 'NONE',  ( 24.29062500061451502, 6.054752690667223547, 3.707466751127219781E-16 ) ) ;
#62017 = CARTESIAN_POINT ( 'NONE',  ( 5.540625000614515905, -3.027376345333614438, 5.243569643749998122 ) ) ;
#62018 = ORIENTED_EDGE ( 'NONE', *, *, #61665, .F. ) ;
#62019 = EDGE_CURVE ( 'NONE', #14534, #15843, #37146, .T. ) ;
#62020 = CARTESIAN_POINT ( 'NONE',  ( 1.071796769724491893, 14.28259618943233455, 33.99999999999999289 ) ) ;
#62021 = CARTESIAN_POINT ( 'NONE',  ( 3.440625000614518036, -3.027376345333610441, -5.243569643749999898 ) ) ;
#62022 = AXIS2_PLACEMENT_3D ( 'NONE', #49752, #43845, #9492 ) ;
#62023 = CARTESIAN_POINT ( 'NONE',  ( 9.759375000614516793, -4.119189519843965641, -2.378215178125001383 ) ) ;
#62024 = CARTESIAN_POINT ( 'NONE',  ( 3.999999999999998668, 13.06250000000000000, 27.69059892324149530 ) ) ;
#62025 = CARTESIAN_POINT ( 'NONE',  ( 1.999999999999998668, 11.41250000122903430, -33.46410161513775705 ) ) ;
#62026 = CARTESIAN_POINT ( 'NONE',  ( 2.121784821875001281, 17.30937500061451573, -26.32496088578401938 ) ) ;
#62027 = CARTESIAN_POINT ( 'NONE',  ( 5.700000001229033941, 5.773502691896255534, 3.535250795749688894E-16 ) ) ;
#62028 = APPLICATION_CONTEXT ( 'automotive_design' ) ;
#62029 = CARTESIAN_POINT ( 'NONE',  ( 8.512499999999999289, -5.773502691896255534, -1.060575238724906372E-15 ) ) ;
#62030 =( BOUNDED_CURVE ( )  B_SPLINE_CURVE ( 2, ( #91, #56583, #62130, #12238, #39245, #34769, #57302 ),
 .UNSPECIFIED., .F., .F. ) 
 B_SPLINE_CURVE_WITH_KNOTS ( ( 3, 2, 2, 3 ),
 ( 0.1833333333333333204, 0.1861111111111111160, 0.1888888888888888562, 0.1916666666666666519 ),
 .UNSPECIFIED. ) 
 CURVE ( )  GEOMETRIC_REPRESENTATION_ITEM ( )  RATIONAL_B_SPLINE_CURVE ( ( 1.000000000000000000, 0.8660254037844387076, 1.000000000000000000, 0.8660254037844387076, 1.000000000000000000, 0.8660254037844400399, 0.9999999999999986677 ) ) 
 REPRESENTATION_ITEM ( '' )  );
#62031 = AXIS2_PLACEMENT_3D ( 'NONE', #38526, #27081, #49612 ) ;
#62032 = CARTESIAN_POINT ( 'NONE',  ( 3.187500001229033764, -4.330127018922194537, 2.499999999999995559 ) ) ;
#62033 = CARTESIAN_POINT ( 'NONE',  ( 11.97187500061451892, -6.054752690667223547, -1.112240025338166033E-15 ) ) ;
#62034 = LINE ( 'NONE', #51679, #543 ) ;
#62035 = CARTESIAN_POINT ( 'NONE',  ( 3.651773823418189124, 3.415340091791402966, 3.978752903393068863 ) ) ;
#62036 = CARTESIAN_POINT ( 'NONE',  ( 0.000000000000000000, 20.00000000000000000, -30.00000000000000000 ) ) ;
#62037 = AXIS2_PLACEMENT_3D ( 'NONE', #53039, #24233, #52318 ) ;
#62038 = B_SPLINE_CURVE_WITH_KNOTS ( 'NONE', 3,
 ( #54409, #19671, #69931, #42225 ),
 .UNSPECIFIED., .F., .F.,
 ( 4, 4 ),
 ( 2.168404344971008868E-19, 0.0006166911802265985596 ),
 .UNSPECIFIED. ) ;
#62039 = CARTESIAN_POINT ( 'NONE',  ( 30.00000000000000000, 6.123233995736764310E-16, -4.999999999999998224 ) ) ;
#62040 = CARTESIAN_POINT ( 'NONE',  ( 11.10937500061451644, -4.541064518000417216, -2.621784821875001281 ) ) ;
#62041 = CARTESIAN_POINT ( 'NONE',  ( 20.43750000122903643, 6.123233995736764310E-16, -4.999999999999998224 ) ) ;
#62042 = CARTESIAN_POINT ( 'NONE',  ( 3.999999999999999112, 14.37500000000000000, 30.00000000000000000 ) ) ;
#62043 = CARTESIAN_POINT ( 'NONE',  ( 4.243569643749999898, 16.84062500061459389, 32.45002607614398471 ) ) ;
#62044 = CARTESIAN_POINT ( 'NONE',  ( 22.02187500061452141, 3.027376345333613106, -5.243569643749998122 ) ) ;
#62045 = PRESENTATION_STYLE_ASSIGNMENT (( #67598 ) ) ;
#62046 = CARTESIAN_POINT ( 'NONE',  ( 2.990625000614519191, -3.027376345333610441, -5.243569643749999898 ) ) ;
#62047 = CARTESIAN_POINT ( 'NONE',  ( 18.68437500061451573, -2.746126346562642428, -4.756430356249999214 ) ) ;
#62048 = CARTESIAN_POINT ( 'NONE',  ( 22.56562500061451715, 3.027376345333611329, 5.243569643749999010 ) ) ;
#62049 = CARTESIAN_POINT ( 'NONE',  ( 15.47812500061451679, -4.541064518000419881, 2.621784821874995952 ) ) ;
#62050 = CARTESIAN_POINT ( 'NONE',  ( 14.71875000122903465, 2.886751345948126879, 4.999999999999999112 ) ) ;
#62051 = CARTESIAN_POINT ( 'NONE',  ( 11.29687500061451644, 6.054752690667223547, 3.707466751127219781E-16 ) ) ;
#62052 = CARTESIAN_POINT ( 'NONE',  ( 28.76249999999999929, -5.773502691896255534, -1.060575238724906372E-15 ) ) ;
#62053 = CARTESIAN_POINT ( 'NONE',  ( 26.10000000122903430, -2.886751345948129988, 4.999999999999997335 ) ) ;
#62054 = CARTESIAN_POINT ( 'NONE',  ( 3.534375000614518036, 6.421520780324663323E-16, -5.243569643749999010 ) ) ;
#62055 = CARTESIAN_POINT ( 'NONE',  ( 15.23437500061451644, 6.421520780324663323E-16, -5.243569643749999010 ) ) ;
#62056 = CARTESIAN_POINT ( 'NONE',  ( 28.95937500061451431, 0.000000000000000000, 5.243569643749999010 ) ) ;
#62057 = CARTESIAN_POINT ( 'NONE',  ( -1.071796769724475906, 11.35759618943233562, 25.99999999999999289 ) ) ;
#62058 = CARTESIAN_POINT ( 'NONE',  ( -3.999999999999999112, 12.01250000122903394, 30.00000000000000000 ) ) ;
#62059 = CARTESIAN_POINT ( 'NONE',  ( 22.35937500061451644, -4.541064518000417216, -2.621784821875001281 ) ) ;
#62060 = CARTESIAN_POINT ( 'NONE',  ( 13.62187500061451750, 3.027376345333611329, 5.243569643749999010 ) ) ;
#62061 = CARTESIAN_POINT ( 'NONE',  ( 1.878215178124997609, 15.82812499938548356, 33.25316411605952993 ) ) ;
#62062 = CARTESIAN_POINT ( 'NONE',  ( 27.26249999999999929, 2.886751345948126879, 4.999999999999999112 ) ) ;
#62063 = CARTESIAN_POINT ( 'NONE',  ( 4.050000001229035362, -2.886751345948129988, 4.999999999999997335 ) ) ;
#62064 = CARTESIAN_POINT ( 'NONE',  ( 7.584375000614516971, 5.492252693125287522, 3.363034840372157021E-16 ) ) ;
#62065 = CARTESIAN_POINT ( 'NONE',  ( 18.44062500061451715, 6.054752690667223547, 3.707466751127219781E-16 ) ) ;
#62066 = CARTESIAN_POINT ( 'NONE',  ( 7.050000000000000711, 0.000000000000000000, 4.999999999999998224 ) ) ;
#62067 = CARTESIAN_POINT ( 'NONE',  ( 13.61250000122903359, -4.330127018922190985, -2.500000000000001332 ) ) ;
#62068 = CARTESIAN_POINT ( 'NONE',  ( 16.38749999999999929, 5.773502691896255534, 3.535250795749688894E-16 ) ) ;
#62069 = CARTESIAN_POINT ( 'NONE',  ( 2.121784821874999061, 13.80312500061451786, 26.32496088578401583 ) ) ;
#62070 = CARTESIAN_POINT ( 'NONE',  ( 24.88125000122903074, 6.123233995736764310E-16, -4.999999999999998224 ) ) ;
#62071 = CARTESIAN_POINT ( 'NONE',  ( 20.13750000122903216, 4.330127018922191873, 2.499999999999999556 ) ) ;
#62072 = CARTESIAN_POINT ( 'NONE',  ( -2.000000000000000000, 13.28750000122903430, 26.53589838486224650 ) ) ;
#62073 = CARTESIAN_POINT ( 'NONE',  ( 26.40937500061451715, -4.541064518000417216, -2.621784821875001281 ) ) ;
#62074 = VECTOR ( 'NONE', #51292, 1000.000000000000000 ) ;
#62075 = ORIENTED_EDGE ( 'NONE', *, *, #7791, .F. ) ;
#62076 = CARTESIAN_POINT ( 'NONE',  ( 22.71562500061451573, -6.054752690667223547, -1.112240025338166033E-15 ) ) ;
#62077 = CARTESIAN_POINT ( 'NONE',  ( 21.79687500061451644, -3.027376345333614438, 5.243569643749998122 ) ) ;
#62078 = CARTESIAN_POINT ( 'NONE',  ( 5.549999999999998934, 4.330127018922192761, -2.499999999999997780 ) ) ;
#62079 = CARTESIAN_POINT ( 'NONE',  ( 9.178125000614517859, -4.541064518000419881, 2.621784821874995952 ) ) ;
#62080 = CARTESIAN_POINT ( 'NONE',  ( 23.54062500061451146, -3.027376345333614438, 5.243569643749998122 ) ) ;
#62081 = CARTESIAN_POINT ( 'NONE',  ( 13.54687500061451999, 6.054752690667223547, 3.707466751127219781E-16 ) ) ;
#62082 = CARTESIAN_POINT ( 'NONE',  ( 17.40937500061451715, -4.541064518000417216, -2.621784821875001281 ) ) ;
#62083 = CARTESIAN_POINT ( 'NONE',  ( 4.426899456784435749, 2.324341024790166799, -4.700261844762904317 ) ) ;
#62084 = CARTESIAN_POINT ( 'NONE',  ( 2.121784821874999061, 18.30312500061451431, 26.32496088578401583 ) ) ;
#62085 = CARTESIAN_POINT ( 'NONE',  ( 20.36250000122903359, -4.330127018922190985, -2.500000000000001332 ) ) ;
#62086 = CARTESIAN_POINT ( 'NONE',  ( 15.04687500061451644, -2.746126346562646425, 4.756430356249996549 ) ) ;
#62087 = CARTESIAN_POINT ( 'NONE',  ( 11.95312500061451644, -4.541064518000417216, -2.621784821875001281 ) ) ;
#62088 = CARTESIAN_POINT ( 'NONE',  ( 6.646875000614518747, -3.027376345333610441, -5.243569643749999898 ) ) ;
#62089 = CARTESIAN_POINT ( 'NONE',  ( 4.771875000614516971, -6.054752690667223547, -1.112240025338166033E-15 ) ) ;
#62090 = VERTEX_POINT ( 'NONE', #35578 ) ;
#62091 = CARTESIAN_POINT ( 'NONE',  ( 28.69687500061451502, -3.027376345333610441, -5.243569643749999898 ) ) ;
#62092 = CARTESIAN_POINT ( 'NONE',  ( 16.37812500061451715, -4.541064518000419881, 2.621784821874995952 ) ) ;
#62093 = CARTESIAN_POINT ( 'NONE',  ( 28.12500000122902932, 2.886751345948129099, -4.999999999999998224 ) ) ;
#62094 = CARTESIAN_POINT ( 'NONE',  ( 27.92812500061451431, 4.541064518000418104, 2.621784821874999949 ) ) ;
#62095 = CARTESIAN_POINT ( 'NONE',  ( 20.85937500061451644, 0.000000000000000000, 5.243569643749999010 ) ) ;
#62096 = CARTESIAN_POINT ( 'NONE',  ( 18.10312500061451502, 0.000000000000000000, 5.243569643749999010 ) ) ;
#62097 = CARTESIAN_POINT ( 'NONE',  ( -0.6945855716117766976, 10.00052347946771825, 26.06076772914964934 ) ) ;
#62098 = CARTESIAN_POINT ( 'NONE',  ( 23.72812500061451502, 6.421520780324663323E-16, -5.243569643749999010 ) ) ;
#62099 = CARTESIAN_POINT ( 'NONE',  ( 4.800000001229032698, 5.773502691896255534, 3.535250795749688894E-16 ) ) ;
#62100 = EDGE_LOOP ( 'NONE', ( #23302, #58773, #47934, #42024 ) ) ;
#62101 = CARTESIAN_POINT ( 'NONE',  ( 27.56250000000000000, 2.886751345948129099, -4.999999999999998224 ) ) ;
#62102 = CARTESIAN_POINT ( 'NONE',  ( 4.000000000000000000, 12.08750000000000036, -27.69059892324149530 ) ) ;
#62103 = CARTESIAN_POINT ( 'NONE',  ( 2.655984681222220721E-16, 16.91562499938548214, 25.66244784525396483 ) ) ;
#62104 = EDGE_CURVE ( 'NONE', #9764, #1518, #31131, .T. ) ;
#62105 = CARTESIAN_POINT ( 'NONE',  ( 3.946875000614517681, -3.027376345333610441, -5.243569643749999898 ) ) ;
#62106 = CARTESIAN_POINT ( 'NONE',  ( 9.853125000614516793, 4.541064518000418104, -2.621784821874998173 ) ) ;
#62107 = CARTESIAN_POINT ( 'NONE',  ( 24.86250000122903359, -4.330127018922190985, -2.500000000000001332 ) ) ;
#62108 = CARTESIAN_POINT ( 'NONE',  ( 12.00937500061451857, -4.541064518000417216, -2.621784821875001281 ) ) ;
#62109 = CARTESIAN_POINT ( 'NONE',  ( 29.61562500061451431, 3.027376345333613106, -5.243569643749998122 ) ) ;
#62110 = CARTESIAN_POINT ( 'NONE',  ( 28.53749999999999787, 5.773502691896255534, 3.535250795749688894E-16 ) ) ;
#62111 = DIRECTION ( 'NONE',  ( 0.000000000000000000, 0.000000000000000000, 1.000000000000000000 ) ) ;
#62112 = CARTESIAN_POINT ( 'NONE',  ( 13.67812500061451786, -4.541064518000419881, 2.621784821874995952 ) ) ;
#62113 = VERTEX_POINT ( 'NONE', #70297 ) ;
#62114 = CARTESIAN_POINT ( 'NONE',  ( 10.00312500061451715, 0.000000000000000000, 5.243569643749999010 ) ) ;
#62115 = CARTESIAN_POINT ( 'NONE',  ( 6.103125000614515905, -4.541064518000417216, -2.621784821875001281 ) ) ;
#62116 = VECTOR ( 'NONE', #70518, 1000.000000000000000 ) ;
#62117 = CARTESIAN_POINT ( 'NONE',  ( 17.85937500061451999, -4.119189519843965641, -2.378215178125001383 ) ) ;
#62118 = DIRECTION ( 'NONE',  ( -1.000000000000000000, -0.000000000000000000, -0.000000000000000000 ) ) ;
#62119 = CARTESIAN_POINT ( 'NONE',  ( 16.27499999999999858, 6.123233995736764310E-16, -4.999999999999998224 ) ) ;
#62120 = CARTESIAN_POINT ( 'NONE',  ( 16.05937500061451573, -4.541064518000417216, -2.621784821875001281 ) ) ;
#62121 = CARTESIAN_POINT ( 'NONE',  ( 11.85000000122903430, -2.886751345948125991, -5.000000000000000000 ) ) ;
#62122 = CARTESIAN_POINT ( 'NONE',  ( 19.69687500061451857, -3.027376345333610441, -5.243569643749999898 ) ) ;
#62123 = CARTESIAN_POINT ( 'NONE',  ( 20.99999999999999645, 0.000000000000000000, 4.999999999999998224 ) ) ;
#62124 = CARTESIAN_POINT ( 'NONE',  ( 21.42187500061451644, -6.054752690667223547, -1.112240025338166033E-15 ) ) ;
#62125 = CARTESIAN_POINT ( 'NONE',  ( -4.243569643749997233, 14.89062500061451644, -27.54997392385601174 ) ) ;
#62126 = CARTESIAN_POINT ( 'NONE',  ( 7.312499999999998224, 2.886751345948062486, -5.000000000000113687 ) ) ;
#62127 = CARTESIAN_POINT ( 'NONE',  ( 24.87187500061451217, -4.119189519843968306, 2.378215178124996054 ) ) ;
#62128 = CARTESIAN_POINT ( 'NONE',  ( 3.999999999999999112, 11.67500000000000071, -30.00000000000000000 ) ) ;
#62129 = CARTESIAN_POINT ( 'NONE',  ( 27.92812500061451431, 4.541064518000418104, 2.621784821874999949 ) ) ;
#62130 = CARTESIAN_POINT ( 'NONE',  ( 24.97499999999999787, 4.330127018922191873, 2.499999999999999556 ) ) ;
#62131 = CARTESIAN_POINT ( 'NONE',  ( 28.95937500061451431, 0.000000000000000000, 5.243569643749999010 ) ) ;
#62132 = CARTESIAN_POINT ( 'NONE',  ( 24.00000000000000000, 4.330127018922192761, -2.499999999999997780 ) ) ;
#62133 = CARTESIAN_POINT ( 'NONE',  ( 8.915625000614515017, 3.027376345333613106, -5.243569643749998122 ) ) ;
#62134 = CARTESIAN_POINT ( 'NONE',  ( 27.34687500061451360, 4.119189519843966529, -2.378215178124998275 ) ) ;
#62135 = CARTESIAN_POINT ( 'NONE',  ( 19.47187500061451360, 3.027376345333611329, 5.243569643749999010 ) ) ;
#62136 = CARTESIAN_POINT ( 'NONE',  ( 10.88437500061451679, -2.746126346562646425, 4.756430356249996549 ) ) ;
#62137 = CARTESIAN_POINT ( 'NONE',  ( 6.253125000614517148, 4.541064518000418104, -2.621784821874998173 ) ) ;
#62138 = CARTESIAN_POINT ( 'NONE',  ( 9.759375000614516793, -4.541064518000417216, -2.621784821875001281 ) ) ;
#62139 = ORIENTED_EDGE ( 'NONE', *, *, #8132, .T. ) ;
#62140 = CARTESIAN_POINT ( 'NONE',  ( 20.37187500061451573, 3.027376345333611329, 5.243569643749999010 ) ) ;
#62141 = CARTESIAN_POINT ( 'NONE',  ( 28.87499999999999645, 6.123233995736764310E-16, -4.999999999999998224 ) ) ;
#62142 = CARTESIAN_POINT ( 'NONE',  ( 29.88749999999999929, 5.773502691896255534, 3.535250795749688894E-16 ) ) ;
#62143 = CARTESIAN_POINT ( 'NONE',  ( 4.987500000000002487, -2.886751345948125991, -5.000000000000000000 ) ) ;
#62144 = CARTESIAN_POINT ( 'NONE',  ( 15.11250000122903359, 4.330127018922192761, -2.499999999999997780 ) ) ;
#62145 = LINE ( 'NONE', #28886, #1887 ) ;
#62146 = CARTESIAN_POINT ( 'NONE',  ( -5.810221930991193690E-16, 18.98750000000000071, -34.00000000000000000 ) ) ;
#62147 = ORIENTED_EDGE ( 'NONE', *, *, #53394, .T. ) ;
#62148 = CARTESIAN_POINT ( 'NONE',  ( 13.87500000000000178, -4.330127018922194537, 2.499999999999995559 ) ) ;
#62149 = CARTESIAN_POINT ( 'NONE',  ( 24.59062500061451573, -3.027376345333610441, -5.243569643749999898 ) ) ;
#62150 = CARTESIAN_POINT ( 'NONE',  ( 13.12500000000000178, 6.123233995736764310E-16, -4.999999999999998224 ) ) ;
#62151 = CARTESIAN_POINT ( 'NONE',  ( 10.27500000122903323, 2.886751345948126879, 4.999999999999999112 ) ) ;
#62152 = CARTESIAN_POINT ( 'NONE',  ( 8.465625000614515727, 3.027376345333613106, -5.243569643749998122 ) ) ;
#62153 = ADVANCED_FACE ( 'NONE', ( #47037 ), #42223, .F. ) ;
#62154 = CARTESIAN_POINT ( 'NONE',  ( 8.362500000000002487, 2.886751345948126879, 4.999999999999999112 ) ) ;
#62155 = FACE_OUTER_BOUND ( 'NONE', #15694, .T. ) ;
#62156 = CARTESIAN_POINT ( 'NONE',  ( 4.243569643749999898, 13.78437500061451715, -30.00000000000000000 ) ) ;
#62157 = CARTESIAN_POINT ( 'NONE',  ( 28.98750000122903359, 6.123233995736764310E-16, -4.999999999999998224 ) ) ;
#62158 = CARTESIAN_POINT ( 'NONE',  ( 1.878215178125000495, 17.21562499938548285, 26.74683588394047007 ) ) ;
#62159 = CARTESIAN_POINT ( 'NONE',  ( 8.662499999999999645, 2.886751345948129099, -4.999999999999998224 ) ) ;
#62160 = CARTESIAN_POINT ( 'NONE',  ( -3.999999999999999112, 12.76250000000000107, 27.69059892324149885 ) ) ;
#62161 = ORIENTED_EDGE ( 'NONE', *, *, #36401, .F. ) ;
#62162 = CARTESIAN_POINT ( 'NONE',  ( 22.11562500061451786, 3.027376345333611329, 5.243569643749999010 ) ) ;
#62163 = CARTESIAN_POINT ( 'NONE',  ( 15.00000000122903465, -2.886751345948125991, -5.000000000000000000 ) ) ;
#62164 = CARTESIAN_POINT ( 'NONE',  ( 28.56562500061451715, -6.054752690667223547, -1.112240025338166033E-15 ) ) ;
#62165 = AXIS2_PLACEMENT_3D ( 'NONE', #42447, #60512, #30623 ) ;
#62166 = DIRECTION ( 'NONE',  ( -1.000000000000000000, -0.000000000000000000, -0.000000000000000000 ) ) ;
#62167 = CARTESIAN_POINT ( 'NONE',  ( 18.38437500061451857, 6.421520780324663323E-16, -5.243569643749999010 ) ) ;
#62168 = CARTESIAN_POINT ( 'NONE',  ( 16.22812500061451857, 4.541064518000418104, 2.621784821874999949 ) ) ;
#62169 = CARTESIAN_POINT ( 'NONE',  ( -4.243569643749999898, 12.11562500061459247, -32.45002607614398471 ) ) ;
#62170 = CARTESIAN_POINT ( 'NONE',  ( 6.890625000614516438, -3.027376345333614438, 5.243569643749998122 ) ) ;
#62171 = CARTESIAN_POINT ( 'NONE',  ( 29.51250000122903216, 4.330127018922192761, -2.499999999999997780 ) ) ;
#62172 = CARTESIAN_POINT ( 'NONE',  ( 21.04687500061451644, -2.746126346562641984, -4.756430356249999214 ) ) ;
#62173 = CARTESIAN_POINT ( 'NONE',  ( 18.96562500061451573, 3.027376345333611329, 5.243569643749999010 ) ) ;
#62174 = CARTESIAN_POINT ( 'NONE',  ( 13.46249999999999858, -5.773502691896255534, -1.060575238724906372E-15 ) ) ;
#62175 = CARTESIAN_POINT ( 'NONE',  ( 3.412500001229032964, 4.330127018922192761, -2.499999999999997780 ) ) ;
#62176 = CARTESIAN_POINT ( 'NONE',  ( 12.79687500061451821, -3.027376345333614438, 5.243569643749998122 ) ) ;
#62177 = CARTESIAN_POINT ( 'NONE',  ( 12.45937500061451786, -4.541064518000417216, -2.621784821875001281 ) ) ;
#62178 = CARTESIAN_POINT ( 'NONE',  ( 20.18437500061451573, 6.421520780324663323E-16, -5.243569643749999010 ) ) ;
#62179 = ORIENTED_EDGE ( 'NONE', *, *, #25113, .F. ) ;
#62180 = CARTESIAN_POINT ( 'NONE',  ( 30.00000000000000000, 0.000000000000000000, 0.000000000000000000 ) ) ;
#62181 = CARTESIAN_POINT ( 'NONE',  ( 24.10312500061451502, -4.541064518000417216, -2.621784821875001281 ) ) ;
#62182 = CARTESIAN_POINT ( 'NONE',  ( 24.21562500061451573, 3.027376345333613106, -5.243569643749998122 ) ) ;
#62183 = CARTESIAN_POINT ( 'NONE',  ( 2.393811435568372112E-14, 17.28124999877096712, 34.00000000000000000 ) ) ;
#62184 = CARTESIAN_POINT ( 'NONE',  ( 1.999999999999998668, 17.15000000000000213, 26.53589838486224650 ) ) ;
#62185 = CARTESIAN_POINT ( 'NONE',  ( 5.109375000614518214, 0.000000000000000000, 5.243569643749999010 ) ) ;
#62186 = CARTESIAN_POINT ( 'NONE',  ( 12.26250000122903394, -4.330127018922190985, -2.500000000000001332 ) ) ;
#62187 = B_SPLINE_CURVE_WITH_KNOTS ( 'NONE', 3,
 ( #45664, #27947, #963, #44939, #28304, #33114, #39032, #55652, #50839, #5048 ),
 .UNSPECIFIED., .F., .F.,
 ( 4, 3, 3, 4 ),
 ( 1.829295516389420302E-16, 0.0001572384447036336735, 0.0003144798658762968193, 0.0005339943342314175910 ),
 .UNSPECIFIED. ) ;
#62188 = CARTESIAN_POINT ( 'NONE',  ( 7.837500001229035007, 6.123233995736764310E-16, -4.999999999999998224 ) ) ;
#62189 = CARTESIAN_POINT ( 'NONE',  ( -0.1398361002794819008, 5.000000000000000888, 26.00000000000000000 ) ) ;
#62190 = CARTESIAN_POINT ( 'NONE',  ( 27.45000000122903572, -2.886751345948129988, 4.999999999999997335 ) ) ;
#62191 = CARTESIAN_POINT ( 'NONE',  ( 2.828200636599751609E-16, 18.85624999877096641, 25.38119784648299415 ) ) ;
#62192 = CARTESIAN_POINT ( 'NONE',  ( 16.06875000122903074, 2.886751345948126879, 4.999999999999999112 ) ) ;
#62193 = CARTESIAN_POINT ( 'NONE',  ( 10.84687500061451892, 6.054752690667223547, 3.707466751127219781E-16 ) ) ;
#62194 = CARTESIAN_POINT ( 'NONE',  ( 0.000000000000000000, 20.00000000000000000, 30.00000000000000000 ) ) ;
#62195 = CARTESIAN_POINT ( 'NONE',  ( 17.57812500061451644, 4.541064518000418104, 2.621784821874999949 ) ) ;
#62196 = CARTESIAN_POINT ( 'NONE',  ( 13.39687500061451608, -3.027376345333610441, -5.243569643749999898 ) ) ;
#62197 = CARTESIAN_POINT ( 'NONE',  ( 4.115625000614516082, 3.027376345333611329, 5.243569643749999010 ) ) ;
#62198 = CARTESIAN_POINT ( 'NONE',  ( 22.92187500061451644, 3.027376345333612662, -5.243569643749998122 ) ) ;
#62199 = CARTESIAN_POINT ( 'NONE',  ( 9.159375000614515372, 0.000000000000000000, 5.243569643749999010 ) ) ;
#62200 = CARTESIAN_POINT ( 'NONE',  ( 5.728125000614515905, 6.421520780324663323E-16, -5.243569643749999010 ) ) ;
#62201 =( BOUNDED_CURVE ( )  B_SPLINE_CURVE ( 2, ( #25839, #37283, #7116, #63618, #64988, #59805, #66087 ),
 .UNSPECIFIED., .F., .F. ) 
 B_SPLINE_CURVE_WITH_KNOTS ( ( 3, 2, 2, 3 ),
 ( 0.7750000000000001332, 0.7777777777777779011, 0.7805555555555556690, 0.7833333333333334370 ),
 .UNSPECIFIED. ) 
 CURVE ( )  GEOMETRIC_REPRESENTATION_ITEM ( )  RATIONAL_B_SPLINE_CURVE ( ( 0.9999999999999946709, 0.8660254037844440367, 1.000000000000000000, 0.8660254037844387076, 1.000000000000000000, 0.8660254037844333785, 1.000000000000005329 ) ) 
 REPRESENTATION_ITEM ( '' )  );
#62202 = CARTESIAN_POINT ( 'NONE',  ( 5.287500001229035185, 4.330127018922191873, 2.499999999999999556 ) ) ;
#62203 = CARTESIAN_POINT ( 'NONE',  ( 20.35312500061451502, 0.000000000000000000, 5.243569643749999010 ) ) ;
#62204 = CARTESIAN_POINT ( 'NONE',  ( 8.550000001229031810, -2.886751345948129988, 4.999999999999997335 ) ) ;
#62205 = CARTESIAN_POINT ( 'NONE',  ( 17.12812500061451715, 4.541064518000418104, 2.621784821874999949 ) ) ;
#62206 = CARTESIAN_POINT ( 'NONE',  ( 14.09062500061451750, -3.027376345333614438, 5.243569643749998122 ) ) ;
#62207 = CARTESIAN_POINT ( 'NONE',  ( 26.22187500061451715, 2.746126346562643317, 4.756430356249998326 ) ) ;
#62208 = CARTESIAN_POINT ( 'NONE',  ( 14.32500000000000107, -4.330127018922194537, 2.499999999999995559 ) ) ;
#62209 = CARTESIAN_POINT ( 'NONE',  ( 8.550000001229031810, -2.886751345948129988, 4.999999999999997335 ) ) ;
#62210 = EDGE_CURVE ( 'NONE', #38121, #38724, #57433, .T. ) ;
#62211 = CARTESIAN_POINT ( 'NONE',  ( 6.440625000614517148, -3.027376345333614438, 5.243569643749998122 ) ) ;
#62212 = CARTESIAN_POINT ( 'NONE',  ( 19.23750000122903714, 4.330127018922191873, 2.499999999999999556 ) ) ;
#62213 = CARTESIAN_POINT ( 'NONE',  ( 26.06250000000000000, -5.773502691896255534, -1.060575238724906372E-15 ) ) ;
#62214 = CARTESIAN_POINT ( 'NONE',  ( 4.243569643749999898, 10.14687500061451786, -27.54997392385601529 ) ) ;
#62215 = DIRECTION ( 'NONE',  ( 0.000000000000000000, 0.000000000000000000, 1.000000000000000000 ) ) ;
#62216 = CARTESIAN_POINT ( 'NONE',  ( 3.750000001229034652, -2.886751345948125991, -5.000000000000000000 ) ) ;
#62217 = CARTESIAN_POINT ( 'NONE',  ( -3.999999999999997335, 11.48750000000000071, -27.69059892324149530 ) ) ;
#62218 = CARTESIAN_POINT ( 'NONE',  ( 20.85937500061451644, 0.000000000000000000, 5.243569643749999010 ) ) ;
#62219 = CARTESIAN_POINT ( 'NONE',  ( -1.999999999999997113, 16.58750000122903501, 33.46410161513775705 ) ) ;
#62220 = CARTESIAN_POINT ( 'NONE',  ( 16.00312500061451715, -4.541064518000417216, -2.621784821875001281 ) ) ;
#62221 = CARTESIAN_POINT ( 'NONE',  ( 11.86875000122903145, 2.886751345948129099, -4.999999999999998224 ) ) ;
#62222 = CARTESIAN_POINT ( 'NONE',  ( 11.02500000000000036, 4.330127018922191873, 2.499999999999999556 ) ) ;
#62223 = CARTESIAN_POINT ( 'NONE',  ( 26.66250000000000142, 2.886751345948129099, -4.999999999999997335 ) ) ;
#62224 = CARTESIAN_POINT ( 'NONE',  ( 25.35937500061451644, 0.000000000000000000, 5.243569643749999010 ) ) ;
#62225 = CARTESIAN_POINT ( 'NONE',  ( 19.13437500061451857, -2.746126346562641984, -4.756430356249999214 ) ) ;
#62226 = CARTESIAN_POINT ( 'NONE',  ( 13.00312500061451537, 4.541064518000418104, -2.621784821874998173 ) ) ;
#62227 = CARTESIAN_POINT ( 'NONE',  ( 9.684375000614517504, -4.541064518000419881, 2.621784821874995952 ) ) ;
#62228 = ORIENTED_EDGE ( 'NONE', *, *, #44171, .T. ) ;
#62229 = CARTESIAN_POINT ( 'NONE',  ( 2.941572294020245337, -4.043263892169386864, -3.278731392431392333 ) ) ;
#62230 = CARTESIAN_POINT ( 'NONE',  ( 20.57812500061451644, 6.421520780324663323E-16, -5.243569643749999010 ) ) ;
#62231 = CARTESIAN_POINT ( 'NONE',  ( 4.000000000000000000, 11.18750000000000178, -27.69059892324149885 ) ) ;
#62232 = CARTESIAN_POINT ( 'NONE',  ( -1.071796769724475906, 12.82009619066136707, 25.99999999999999289 ) ) ;
#62233 =( BOUNDED_CURVE ( )  B_SPLINE_CURVE ( 2, ( #56228, #28157, #71767, #7420, #46224, #57298, #17410, #17759, #22950 ),
 .UNSPECIFIED., .F., .F. ) 
 B_SPLINE_CURVE_WITH_KNOTS ( ( 3, 2, 2, 2, 3 ),
 ( 0.2934782608695652439, 0.2971014492753623060, 0.3043478260869565410, 0.3115942028985507206, 0.3152173913043478382 ),
 .UNSPECIFIED. ) 
 CURVE ( )  GEOMETRIC_REPRESENTATION_ITEM ( )  RATIONAL_B_SPLINE_CURVE ( ( 0.9330127018922194093, 0.9330127018922198534, 1.000000000000000000, 0.8660254037844387076, 1.000000000000000000, 0.8660254037844387076, 1.000000000000000000, 0.9330127018922188542, 0.9330127018922194093 ) ) 
 REPRESENTATION_ITEM ( '' )  );
#62234 = CARTESIAN_POINT ( 'NONE',  ( 11.25000000000000000, -4.330127018922190985, -2.500000000000001332 ) ) ;
#62235 = CARTESIAN_POINT ( 'NONE',  ( 21.67500000122903359, -5.773502691896255534, -1.060575238724906372E-15 ) ) ;
#62236 = CARTESIAN_POINT ( 'NONE',  ( 15.55312500061451608, -4.541064518000417216, -2.621784821875001281 ) ) ;
#62237 = CARTESIAN_POINT ( 'NONE',  ( 12.19687500061451502, 0.000000000000000000, 4.756430356249998326 ) ) ;
#62238 = ORIENTED_EDGE ( 'NONE', *, *, #46580, .T. ) ;
#62239 = CARTESIAN_POINT ( 'NONE',  ( 20.21250000000000213, -5.773502691896255534, -1.060575238724906372E-15 ) ) ;
#62240 = CARTESIAN_POINT ( 'NONE',  ( 23.62500000000000000, 4.330127018922191873, 2.499999999999999556 ) ) ;
#62241 =( BOUNDED_CURVE ( )  B_SPLINE_CURVE ( 2, ( #33972, #56511, #45436, #11813, #49527, #40564, #52730 ),
 .UNSPECIFIED., .F., .F. ) 
 B_SPLINE_CURVE_WITH_KNOTS ( ( 3, 2, 2, 3 ),
 ( 0.7916666666666666297, 0.7944444444444443976, 0.7972222222222222765, 0.8000000000000000444 ),
 .UNSPECIFIED. ) 
 CURVE ( )  GEOMETRIC_REPRESENTATION_ITEM ( )  RATIONAL_B_SPLINE_CURVE ( ( 1.000000000000000000, 0.8660254037844387076, 1.000000000000000000, 0.8660254037844387076, 1.000000000000000000, 0.8660254037844387076, 1.000000000000000000 ) ) 
 REPRESENTATION_ITEM ( '' )  );
#62242 = CARTESIAN_POINT ( 'NONE',  ( 22.58437500061451431, 4.541064518000418104, 2.621784821874999949 ) ) ;
#62243 = CARTESIAN_POINT ( 'NONE',  ( 24.96562500061451573, -6.054752690667223547, -1.112240025338166033E-15 ) ) ;
#62244 = ORIENTED_EDGE ( 'NONE', *, *, #8791, .F. ) ;
#62245 = CARTESIAN_POINT ( 'NONE',  ( 7.640625000614517326, 6.054752690667223547, 3.707466751127219781E-16 ) ) ;
#62246 = CARTESIAN_POINT ( 'NONE',  ( 12.44999999999999929, 0.000000000000000000, 4.999999999999998224 ) ) ;
#62247 = CARTESIAN_POINT ( 'NONE',  ( 14.47499999999999964, 6.123233995736764310E-16, -4.999999999999998224 ) ) ;
#62248 = CARTESIAN_POINT ( 'NONE',  ( -3.000416591977282496E-16, 16.99062500061451786, 25.09994784771203058 ) ) ;
#62249 = CARTESIAN_POINT ( 'NONE',  ( 4.696875000614518569, -3.027376345333614438, 5.243569643749998122 ) ) ;
#62250 = CARTESIAN_POINT ( 'NONE',  ( 26.82187500061451857, -6.054752690667223547, -1.112240025338166033E-15 ) ) ;
#62251 = ORIENTED_EDGE ( 'NONE', *, *, #73107, .F. ) ;
#62252 = CARTESIAN_POINT ( 'NONE',  ( 23.16562500061451502, -6.054752690667223547, -1.112240025338166033E-15 ) ) ;
#62253 = CARTESIAN_POINT ( 'NONE',  ( 26.03437500061451715, 6.421520780324663323E-16, -5.243569643749999010 ) ) ;
#62254 = CARTESIAN_POINT ( 'NONE',  ( -4.243569643749998122, 18.49062500061459247, -27.54997392385601174 ) ) ;
#62255 = CARTESIAN_POINT ( 'NONE',  ( 11.77500000000000036, 6.123233995736764310E-16, -4.999999999999998224 ) ) ;
#62256 = CARTESIAN_POINT ( 'NONE',  ( 9.853125000614516793, 4.541064518000418104, -2.621784821874998173 ) ) ;
#62257 = CARTESIAN_POINT ( 'NONE',  ( 29.85937500061451644, 0.000000000000000000, 4.756430356249998326 ) ) ;
#62258 = CARTESIAN_POINT ( 'NONE',  ( 27.89062500061451289, 6.054752690667223547, 3.707466751127219781E-16 ) ) ;
#62259 = CARTESIAN_POINT ( 'NONE',  ( 25.86562500061451431, -6.054752690667223547, -1.112240025338166033E-15 ) ) ;
#62260 = CARTESIAN_POINT ( 'NONE',  ( 8.493750001229027902, -2.886751345948019409, 5.000000000000189182 ) ) ;
#62261 = CARTESIAN_POINT ( 'NONE',  ( 11.74687500061451573, 5.492252693125287522, 3.363034840372157021E-16 ) ) ;
#62262 = CARTESIAN_POINT ( 'NONE',  ( 2.915625000614516793, -6.054752690667223547, -1.112240025338166033E-15 ) ) ;
#62263 = CARTESIAN_POINT ( 'NONE',  ( 18.57187500061451857, 3.027376345333611329, 5.243569643749999010 ) ) ;
#62264 = CARTESIAN_POINT ( 'NONE',  ( -4.243569643749997233, 14.04687500061451999, 32.45002607614398471 ) ) ;
#62265 = EDGE_CURVE ( 'NONE', #38080, #63662, #64989, .T. ) ;
#62266 = CARTESIAN_POINT ( 'NONE',  ( 18.90937500061451360, 4.541064518000418104, -2.621784821874998173 ) ) ;
#62267 = CARTESIAN_POINT ( 'NONE',  ( 29.74687500061451217, 6.054752690667223547, 3.707466751127219781E-16 ) ) ;
#62268 = CARTESIAN_POINT ( 'NONE',  ( -4.243569643749998122, 17.19687500061451502, 32.45002607614398471 ) ) ;
#62269 = CARTESIAN_POINT ( 'NONE',  ( 9.928125000614517859, 4.541064518000418104, 2.621784821874999949 ) ) ;
#62270 = CARTESIAN_POINT ( 'NONE',  ( 8.062500000000000000, -5.773502691896255534, -1.060575238724906372E-15 ) ) ;
#62271 =( BOUNDED_CURVE ( )  B_SPLINE_CURVE ( 2, ( #28624, #62600, #11996, #51162, #69243, #6817, #29351 ),
 .UNSPECIFIED., .F., .F. ) 
 B_SPLINE_CURVE_WITH_KNOTS ( ( 3, 2, 2, 3 ),
 ( 0.7199999999999999734, 0.7233333333333333837, 0.7266666666666666829, 0.7299999999999999822 ),
 .UNSPECIFIED. ) 
 CURVE ( )  GEOMETRIC_REPRESENTATION_ITEM ( )  RATIONAL_B_SPLINE_CURVE ( ( 1.000000000000000000, 0.8660254037844387076, 1.000000000000000000, 0.8660254037844387076, 1.000000000000000000, 0.8660254037844387076, 1.000000000000000000 ) ) 
 REPRESENTATION_ITEM ( '' )  );
#62272 = CARTESIAN_POINT ( 'NONE',  ( 6.721875000614518925, 3.027376345333613106, -5.243569643749998122 ) ) ;
#62273 = DIRECTION ( 'NONE',  ( 0.000000000000000000, 0.000000000000000000, 1.000000000000000000 ) ) ;
#62274 = CARTESIAN_POINT ( 'NONE',  ( 8.428125000614517859, 6.421520780324663323E-16, -5.243569643749999010 ) ) ;
#62275 = CARTESIAN_POINT ( 'NONE',  ( 11.14687500061451608, -3.027376345333610441, -5.243569643749999898 ) ) ;
#62276 = CARTESIAN_POINT ( 'NONE',  ( 20.02500000122903145, 2.886751345948129099, -4.999999999999998224 ) ) ;
#62277 = CARTESIAN_POINT ( 'NONE',  ( 5.484375000614518214, 4.541064518000418104, 2.621784821874999949 ) ) ;
#62278 = CARTESIAN_POINT ( 'NONE',  ( 8.690625000614515372, -3.027376345333614438, 5.243569643749998122 ) ) ;
#62279 = CARTESIAN_POINT ( 'NONE',  ( 5.810221930991193690E-16, 17.50624999877096499, 26.00000000000000000 ) ) ;
#62280 = CARTESIAN_POINT ( 'NONE',  ( 24.20625000122903359, 0.000000000000000000, 4.999999999999998224 ) ) ;
#62281 = CARTESIAN_POINT ( 'NONE',  ( 18.00937500061451502, 4.541064518000418104, -2.621784821874998173 ) ) ;
#62282 = CARTESIAN_POINT ( 'NONE',  ( 3.999999999999998668, 13.17500000122903536, 27.69059892324149530 ) ) ;
#62283 = ORIENTED_EDGE ( 'NONE', *, *, #13482, .F. ) ;
#62284 = CARTESIAN_POINT ( 'NONE',  ( 27.10312500061451502, 0.000000000000000000, 5.243569643749999010 ) ) ;
#62285 = CARTESIAN_POINT ( 'NONE',  ( 13.15312500061451750, 0.000000000000000000, 5.243569643749999010 ) ) ;
#62286 = CARTESIAN_POINT ( 'NONE',  ( 29.78437500061451715, 4.541064518000418104, 2.621784821874999949 ) ) ;
#62287 = CARTESIAN_POINT ( 'NONE',  ( 12.40312500061451573, -4.541064518000417216, -2.621784821875001281 ) ) ;
#62288 = CARTESIAN_POINT ( 'NONE',  ( 2.121784821874999061, 10.70937500061451964, -33.67503911421598417 ) ) ;
#62289 = CARTESIAN_POINT ( 'NONE',  ( 12.86250000122903359, 4.330127018922192761, -2.499999999999997780 ) ) ;
#62290 = CARTESIAN_POINT ( 'NONE',  ( 26.57812500061451644, 4.541064518000418104, 2.621784821874999949 ) ) ;
#62291 = CARTESIAN_POINT ( 'NONE',  ( -2.121784821874996840, 13.57812500061451644, -26.32496088578401583 ) ) ;
#62292 = CARTESIAN_POINT ( 'NONE',  ( 15.26250000122903216, 0.000000000000000000, 4.999999999999998224 ) ) ;
#62293 = CARTESIAN_POINT ( 'NONE',  ( 14.24999999999999822, 0.000000000000000000, 4.999999999999998224 ) ) ;
#62294 = CARTESIAN_POINT ( 'NONE',  ( 21.32812500061451644, -4.541064518000419881, 2.621784821874995952 ) ) ;
#62295 = CARTESIAN_POINT ( 'NONE',  ( 8.671875000614518214, 3.027376345333611329, 5.243569643749999010 ) ) ;
#62296 = CARTESIAN_POINT ( 'NONE',  ( 8.400000001229035007, 5.773502691896255534, 3.535250795749688894E-16 ) ) ;
#62297 = CARTESIAN_POINT ( 'NONE',  ( 15.45000000122903216, -2.886751345948125991, -5.000000000000000000 ) ) ;
#62298 = CARTESIAN_POINT ( 'NONE',  ( 11.87812500061451537, -4.541064518000419881, 2.621784821874995952 ) ) ;
#62299 = CARTESIAN_POINT ( 'NONE',  ( 16.90312500061451573, -4.541064518000417216, -2.621784821875001281 ) ) ;
#62300 = CARTESIAN_POINT ( 'NONE',  ( 27.07500000122903216, -5.773502691896255534, -1.060575238724906372E-15 ) ) ;
#62301 = CARTESIAN_POINT ( 'NONE',  ( 21.60000000000000142, -4.330127018922190985, -2.500000000000001332 ) ) ;
#62302 = CARTESIAN_POINT ( 'NONE',  ( 24.27187500061452141, 3.027376345333613106, -5.243569643749998122 ) ) ;
#62303 = CYLINDRICAL_SURFACE ( 'NONE', #70089, 1.500000000000000444 ) ;
#62304 = ADVANCED_FACE ( 'NONE', ( #47397 ), #69929, .F. ) ;
#62305 = CARTESIAN_POINT ( 'NONE',  ( 11.06250000122903288, 4.330127018922192761, -2.499999999999997780 ) ) ;
#62306 = CARTESIAN_POINT ( 'NONE',  ( 28.17187500061451644, -6.054752690667223547, -1.112240025338166033E-15 ) ) ;
#62307 = CARTESIAN_POINT ( 'NONE',  ( 4.509375000614518569, 4.541064518000418104, -2.621784821874998173 ) ) ;
#62308 = CARTESIAN_POINT ( 'NONE',  ( 22.75312500061451360, -4.541064518000417216, -2.621784821875001281 ) ) ;
#62309 = CARTESIAN_POINT ( 'NONE',  ( 1.878215178124997609, 15.82812499938548356, 33.25316411605952993 ) ) ;
#62310 = CARTESIAN_POINT ( 'NONE',  ( 15.59999999999999964, 0.000000000000000000, 4.999999999999998224 ) ) ;
#62311 = CARTESIAN_POINT ( 'NONE',  ( 10.80937500061451928, 4.541064518000418104, -2.621784821874998173 ) ) ;
#62312 = CARTESIAN_POINT ( 'NONE',  ( 4.433683854237718158, 3.756322295769854325, -3.980998221622843669 ) ) ;
#62313 = CARTESIAN_POINT ( 'NONE',  ( 29.16562500061451502, 3.027376345333613106, -5.243569643749998122 ) ) ;
#62314 = CARTESIAN_POINT ( 'NONE',  ( 6.121875000614517504, -6.054752690667223547, -1.112240025338166033E-15 ) ) ;
#62315 = LINE ( 'NONE', #28334, #69047 ) ;
#62316 = CARTESIAN_POINT ( 'NONE',  ( 26.59687500061451360, 6.054752690667223547, 3.707466751127219781E-16 ) ) ;
#62317 = CARTESIAN_POINT ( 'NONE',  ( -4.243569643749998122, 10.39062500061459637, 32.45002607614398471 ) ) ;
#62318 = CARTESIAN_POINT ( 'NONE',  ( 18.33749999999999858, -2.886751345948129988, 4.999999999999997335 ) ) ;
#62319 = VERTEX_POINT ( 'NONE', #10071 ) ;
#62320 = CARTESIAN_POINT ( 'NONE',  ( 27.07499999999999929, 6.123233995736764310E-16, -4.999999999999998224 ) ) ;
#62321 = CARTESIAN_POINT ( 'NONE',  ( 28.58437500061451786, -4.541064518000419881, 2.621784821874995952 ) ) ;
#62322 = ORIENTED_EDGE ( 'NONE', *, *, #39433, .F. ) ;
#62323 = CARTESIAN_POINT ( 'NONE',  ( 16.52812500061451573, 6.421520780324663323E-16, -5.243569643749999010 ) ) ;
#62324 = CARTESIAN_POINT ( 'NONE',  ( 8.990625000614516082, 6.054752690667223547, 3.707466751127219781E-16 ) ) ;
#62325 = CARTESIAN_POINT ( 'NONE',  ( 19.54687500061451289, -4.119189519843965641, -2.378215178125001383 ) ) ;
#62326 = CARTESIAN_POINT ( 'NONE',  ( 5.071875000614519458, 3.027376345333611329, 5.243569643749999010 ) ) ;
#62327 = CARTESIAN_POINT ( 'NONE',  ( 17.13750000122903216, -4.330127018922194537, 2.499999999999995559 ) ) ;
#62328 = CARTESIAN_POINT ( 'NONE',  ( 22.68750000000000000, 5.773502691896255534, 3.535250795749688894E-16 ) ) ;
#62329 = CARTESIAN_POINT ( 'NONE',  ( 27.97500000000000142, 6.123233995736764310E-16, -4.999999999999998224 ) ) ;
#62330 = CARTESIAN_POINT ( 'NONE',  ( 3.646875000614520079, 6.054752690667223547, 3.707466751127219781E-16 ) ) ;
#62331 = CARTESIAN_POINT ( 'NONE',  ( 11.22187500061451892, 3.027376345333613106, -5.243569643749998122 ) ) ;
#62332 = CARTESIAN_POINT ( 'NONE',  ( 21.00937500061451857, -4.541064518000417216, -2.621784821875001281 ) ) ;
#62333 = CARTESIAN_POINT ( 'NONE',  ( -1.071796769724483234, 15.07009619066136885, -34.00000000000000711 ) ) ;
#62334 = EDGE_LOOP ( 'NONE', ( #50351, #53099, #16445, #71790, #36618, #20731, #40306, #70408, #10419, #45533, #11843, #19266, #60773, #42531, #9308, #25908, #21101, #39955, #5841, #57670, #67448, #20505, #58993, #4759, #70090, #15329, #51999, #56451, #65604, #4118, #56543, #48980, #33347, #42488, #57839, #63756, #62139, #1932, #3177, #46478, #63092, #70395, #72828 ) ) ;
#62335 = CARTESIAN_POINT ( 'NONE',  ( 4.621875000614516615, 3.027376345333611329, 5.243569643749999010 ) ) ;
#62336 = CARTESIAN_POINT ( 'NONE',  ( 7.734375000614517326, 4.541064518000418104, 2.621784821874999949 ) ) ;
#62337 = CARTESIAN_POINT ( 'NONE',  ( 18.37500000000000355, -4.330127018922194537, 2.499999999999995559 ) ) ;
#62338 = CARTESIAN_POINT ( 'NONE',  ( 15.74062500061451608, 6.054752690667223547, 3.707466751127219781E-16 ) ) ;
#62339 = CARTESIAN_POINT ( 'NONE',  ( 4.000000000000000000, 17.03750000000000142, 27.69059892324149530 ) ) ;
#62340 = CARTESIAN_POINT ( 'NONE',  ( 24.78750000122903074, -4.330127018922194537, 2.499999999999995559 ) ) ;
#62341 = EDGE_CURVE ( 'NONE', #13665, #40887, #37037, .T. ) ;
#62342 = CARTESIAN_POINT ( 'NONE',  ( 19.47187500061451360, 2.746126346562643317, 4.756430356249998326 ) ) ;
#62343 = CARTESIAN_POINT ( 'NONE',  ( 9.965625000614517504, 3.027376345333611329, 5.243569643749999010 ) ) ;
#62344 = CARTESIAN_POINT ( 'NONE',  ( 25.80937500061451928, 0.000000000000000000, 5.243569643749999010 ) ) ;
#62345 = CARTESIAN_POINT ( 'NONE',  ( 27.53437500061451360, 4.541064518000418104, 2.621784821874999949 ) ) ;
#62346 = CARTESIAN_POINT ( 'NONE',  ( 8.812500000000000000, 2.886751345948126879, 4.999999999999999112 ) ) ;
#62347 = CARTESIAN_POINT ( 'NONE',  ( -1.999999999999997113, 16.58750000122903501, 33.46410161513775705 ) ) ;
#62348 = CARTESIAN_POINT ( 'NONE',  ( 8.362500001229031810, 4.330127018922192761, -2.499999999999997780 ) ) ;
#62349 = CARTESIAN_POINT ( 'NONE',  ( 19.62187500061451573, -6.054752690667223547, -1.112240025338166033E-15 ) ) ;
#62350 = CARTESIAN_POINT ( 'NONE',  ( 15.12187500061451750, -6.054752690667223547, -1.112240025338166033E-15 ) ) ;
#62351 = CYLINDRICAL_SURFACE ( 'NONE', #40721, 4.999999999999998224 ) ;
#62352 = ORIENTED_EDGE ( 'NONE', *, *, #60856, .F. ) ;
#62353 = CARTESIAN_POINT ( 'NONE',  ( 14.46562500061451750, 3.027376345333611329, 5.243569643749999010 ) ) ;
#62354 = CARTESIAN_POINT ( 'NONE',  ( 26.21250000122903501, -4.330127018922190985, -2.500000000000001332 ) ) ;
#62355 = CARTESIAN_POINT ( 'NONE',  ( 16.05937500061451573, -4.541064518000417216, -2.621784821875001281 ) ) ;
#62356 = CARTESIAN_POINT ( 'NONE',  ( 4.150718249861528264, 3.881368968983215151, 3.764411030299838590 ) ) ;
#62357 = CARTESIAN_POINT ( 'NONE',  ( 17.35312500061451502, -4.541064518000417216, -2.621784821875001281 ) ) ;
#62358 = CARTESIAN_POINT ( 'NONE',  ( 29.45625000122903003, 4.330127018922192761, -2.499999999999997780 ) ) ;
#62359 = CARTESIAN_POINT ( 'NONE',  ( 25.43437500061451573, -4.541064518000419881, 2.621784821874995952 ) ) ;
#62360 = CARTESIAN_POINT ( 'NONE',  ( 2.121784821875001281, 10.95312500061451821, 33.67503911421598417 ) ) ;
#62361 = CARTESIAN_POINT ( 'NONE',  ( 14.48437500061451821, 4.541064518000418104, 2.621784821874999949 ) ) ;
#62362 = CARTESIAN_POINT ( 'NONE',  ( 13.98750000122903359, -4.330127018922194537, 2.499999999999995559 ) ) ;
#62363 = CARTESIAN_POINT ( 'NONE',  ( 8.034375000614518925, 5.824947211148865298E-16, -4.756430356249998326 ) ) ;
#62364 = CARTESIAN_POINT ( 'NONE',  ( -2.121784821874999949, 17.08437500061451786, -33.67503911421598417 ) ) ;
#62365 = CARTESIAN_POINT ( 'NONE',  ( 18.15937500061451715, 0.000000000000000000, 5.243569643749999010 ) ) ;
#62366 = CARTESIAN_POINT ( 'NONE',  ( 20.28750000122903074, -4.330127018922194537, 2.499999999999995559 ) ) ;
#62367 = CARTESIAN_POINT ( 'NONE',  ( 14.10937500061451644, 0.000000000000000000, 5.243569643749999010 ) ) ;
#62368 = CARTESIAN_POINT ( 'NONE',  ( 2.121784821874999061, 11.15937500061451715, 26.32496088578401583 ) ) ;
#62369 = CARTESIAN_POINT ( 'NONE',  ( 23.36250000122903359, 0.000000000000000000, 4.999999999999998224 ) ) ;
#62370 = CARTESIAN_POINT ( 'NONE',  ( 15.36562500061451608, 3.027376345333611329, 5.243569643749999010 ) ) ;
#62371 = CARTESIAN_POINT ( 'NONE',  ( 29.61562500061451431, 3.027376345333613106, -5.243569643749998122 ) ) ;
#62372 = ORIENTED_EDGE ( 'NONE', *, *, #56499, .T. ) ;
#62373 = ORIENTED_EDGE ( 'NONE', *, *, #61105, .F. ) ;
#62374 = CARTESIAN_POINT ( 'NONE',  ( 20.21250000000000213, -5.773502691896255534, -1.060575238724906372E-15 ) ) ;
#62375 = CARTESIAN_POINT ( 'NONE',  ( 17.55000000000000071, -4.330127018922190985, -2.500000000000001332 ) ) ;
#62376 = CARTESIAN_POINT ( 'NONE',  ( 3.578402880298070077, 3.495305883107370448, 28.19419513515084219 ) ) ;
#62377 = CARTESIAN_POINT ( 'NONE',  ( 15.03750000122903252, 6.123233995736764310E-16, -4.999999999999998224 ) ) ;
#62378 = CARTESIAN_POINT ( 'NONE',  ( 20.95312500061451999, -4.541064518000417216, -2.621784821875001281 ) ) ;
#62379 = CARTESIAN_POINT ( 'NONE',  ( 23.12812500061451360, -4.541064518000419881, 2.621784821874995952 ) ) ;
#62380 = CARTESIAN_POINT ( 'NONE',  ( 5.503125000614516260, 0.000000000000000000, 5.243569643749999010 ) ) ;
#62381 = CARTESIAN_POINT ( 'NONE',  ( 29.51249999999999929, 2.886751345948126879, 4.999999999999999112 ) ) ;
#62382 = CARTESIAN_POINT ( 'NONE',  ( 0.000000000000000000, 27.50000000000000000, 30.00000000000000000 ) ) ;
#62383 = CARTESIAN_POINT ( 'NONE',  ( 10.32187500061451679, 2.746126346562645981, -4.756430356249997438 ) ) ;
#62384 = FACE_OUTER_BOUND ( 'NONE', #23909, .T. ) ;
#62385 = CARTESIAN_POINT ( 'NONE',  ( -2.000000000000000000, 10.58750000122903323, -33.46410161513775705 ) ) ;
#62386 = CARTESIAN_POINT ( 'NONE',  ( -4.243569643749997233, 18.09687500061452070, -27.54997392385601174 ) ) ;
#62387 = CARTESIAN_POINT ( 'NONE',  ( 6.450000001229034829, -2.886751345948125991, -5.000000000000000000 ) ) ;
#62388 = CARTESIAN_POINT ( 'NONE',  ( 9.150000000000002132, 4.330127018922192761, -2.499999999999997780 ) ) ;
#62389 = ADVANCED_FACE ( 'NONE', ( #21139 ), #48501, .T. ) ;
#62390 = CARTESIAN_POINT ( 'NONE',  ( 4.537500001229034297, -4.330127018922194537, 2.499999999999995559 ) ) ;
#62391 = CARTESIAN_POINT ( 'NONE',  ( 12.23437500061451821, 4.541064518000418104, 2.621784821874999949 ) ) ;
#62392 = FACE_OUTER_BOUND ( 'NONE', #40422, .T. ) ;
#62393 = CARTESIAN_POINT ( 'NONE',  ( 4.546875000614517326, 6.054752690667223547, 3.707466751127219781E-16 ) ) ;
#62394 = LINE ( 'NONE', #50239, #43251 ) ;
#62395 = DIRECTION ( 'NONE',  ( -1.000000000000000000, -0.000000000000000000, -0.000000000000000000 ) ) ;
#62396 = CARTESIAN_POINT ( 'NONE',  ( 9.196875000614518569, -3.027376345333614438, 5.243569643749998122 ) ) ;
#62397 = CARTESIAN_POINT ( 'NONE',  ( 14.63437500061451679, -4.541064518000419881, 2.621784821874995952 ) ) ;
#62398 = CARTESIAN_POINT ( 'NONE',  ( 2.000000000000001332, 17.11250000122903359, -26.53589838486224650 ) ) ;
#62399 = CARTESIAN_POINT ( 'NONE',  ( 5.475000000000000533, 6.123233995736764310E-16, -4.999999999999998224 ) ) ;
#62400 = CARTESIAN_POINT ( 'NONE',  ( -4.243569643749999898, 17.10312500061459318, 30.00000000000000000 ) ) ;
#62401 = CARTESIAN_POINT ( 'NONE',  ( 21.45937500061451786, -4.541064518000417216, -2.621784821875001281 ) ) ;
#62402 = CARTESIAN_POINT ( 'NONE',  ( -5.810221930991193690E-16, 12.68750000000000000, -34.00000000000000000 ) ) ;
#62403 = CARTESIAN_POINT ( 'NONE',  ( 27.00000000122903288, -2.886751345948129988, 4.999999999999997335 ) ) ;
#62404 = CARTESIAN_POINT ( 'NONE',  ( 17.97187500061451360, 4.119189519843966529, 2.378215178124999607 ) ) ;
#62405 = CARTESIAN_POINT ( 'NONE',  ( 23.69062500061451004, -3.027376345333610441, -5.243569643749999898 ) ) ;
#62406 = CARTESIAN_POINT ( 'NONE',  ( 14.84062500061451750, 6.054752690667223547, 3.707466751127219781E-16 ) ) ;
#62407 = CARTESIAN_POINT ( 'NONE',  ( 25.17187500061451644, 4.119189519843966529, 2.378215178124999607 ) ) ;
#62408 = CARTESIAN_POINT ( 'NONE',  ( 12.98437500061451821, 6.421520780324663323E-16, -5.243569643749999010 ) ) ;
#62409 = CARTESIAN_POINT ( 'NONE',  ( 27.56250000000000000, 2.886751345948129099, -4.999999999999998224 ) ) ;
#62410 = CARTESIAN_POINT ( 'NONE',  ( 24.18750000122903288, 4.330127018922191873, 2.499999999999999556 ) ) ;
#62411 = CARTESIAN_POINT ( 'NONE',  ( 3.046875000614519990, -3.027376345333610441, -5.243569643749999898 ) ) ;
#62412 = CARTESIAN_POINT ( 'NONE',  ( 13.50937500061451679, 4.541064518000418104, -2.621784821874998173 ) ) ;
#62413 = CARTESIAN_POINT ( 'NONE',  ( 29.25937500061451502, 4.541064518000418104, -2.621784821874998173 ) ) ;
#62414 = CARTESIAN_POINT ( 'NONE',  ( 21.82499999999999574, 4.330127018922191873, 2.499999999999999556 ) ) ;
#62415 = CARTESIAN_POINT ( 'NONE',  ( -1.071796769724488563, 12.10490381179670116, 34.00000000000000000 ) ) ;
#62416 = CARTESIAN_POINT ( 'NONE',  ( 23.03437500061451715, 4.541064518000418104, 2.621784821874999949 ) ) ;
#62417 = CARTESIAN_POINT ( 'NONE',  ( 13.43437500061451750, 6.421520780324663323E-16, -5.243569643749999010 ) ) ;
#62418 = CARTESIAN_POINT ( 'NONE',  ( 3.756430356249998770, 15.41562499938548392, 32.16877607737302469 ) ) ;
#62419 = CARTESIAN_POINT ( 'NONE',  ( 26.28749999999999432, 5.773502691896255534, 3.535250795749688894E-16 ) ) ;
#62420 = CARTESIAN_POINT ( 'NONE',  ( 3.187500001229033764, -4.330127018922194537, 2.499999999999995559 ) ) ;
#62421 = CARTESIAN_POINT ( 'NONE',  ( 27.75937500061451502, -4.119189519843965641, -2.378215178125001383 ) ) ;
#62422 = CARTESIAN_POINT ( 'NONE',  ( 17.69062500061451715, -3.027376345333614438, 5.243569643749998122 ) ) ;
#62423 = CARTESIAN_POINT ( 'NONE',  ( 6.712500000000000355, -5.773502691896255534, -1.060575238724906372E-15 ) ) ;
#62424 = CARTESIAN_POINT ( 'NONE',  ( -2.000000000000000000, 14.07500000000000107, 26.53589838486224650 ) ) ;
#62425 = CARTESIAN_POINT ( 'NONE',  ( 17.43750000000000355, -2.886751345948129988, 4.999999999999997335 ) ) ;
#62426 = EDGE_CURVE ( 'NONE', #33889, #44184, #15592, .T. ) ;
#62427 = CARTESIAN_POINT ( 'NONE',  ( 4.243569643749999010, 12.86562500061451608, 27.54997392385601174 ) ) ;
#62428 = CARTESIAN_POINT ( 'NONE',  ( 3.242103837493086330E-14, 11.33750000000000213, -34.00000000000000000 ) ) ;
#62429 = CARTESIAN_POINT ( 'NONE',  ( 20.62500000122903288, 2.886751345948126879, 4.999999999999999112 ) ) ;
#62430 = CARTESIAN_POINT ( 'NONE',  ( 28.32187500061451502, 3.027376345333613106, -5.243569643749998122 ) ) ;
#62431 = ORIENTED_EDGE ( 'NONE', *, *, #63830, .F. ) ;
#62432 = CARTESIAN_POINT ( 'NONE',  ( 20.99062500061451431, -3.027376345333610441, -5.243569643749999898 ) ) ;
#62433 = CARTESIAN_POINT ( 'NONE',  ( 22.28437500061451715, -4.541064518000419881, 2.621784821874995952 ) ) ;
#62434 = CARTESIAN_POINT ( 'NONE',  ( 4.200000000000001954, 4.330127018922192761, -2.499999999999997780 ) ) ;
#62435 = CARTESIAN_POINT ( 'NONE',  ( 8.878125000614515372, 6.421520780324663323E-16, -5.243569643749999010 ) ) ;
#62436 = CARTESIAN_POINT ( 'NONE',  ( 23.39062500061451289, 6.054752690667223547, 3.707466751127219781E-16 ) ) ;
#62437 = CARTESIAN_POINT ( 'NONE',  ( 12.49687500061451573, -3.027376345333610441, -5.243569643749999898 ) ) ;
#62438 = CARTESIAN_POINT ( 'NONE',  ( 15.90937500061451892, 0.000000000000000000, 5.243569643749999010 ) ) ;
#62439 = CARTESIAN_POINT ( 'NONE',  ( -4.243569643749999898, 17.10312500061451502, 30.00000000000000000 ) ) ;
#62440 = CARTESIAN_POINT ( 'NONE',  ( 20.43750000122903643, 6.123233995736764310E-16, -4.999999999999998224 ) ) ;
#62441 = CARTESIAN_POINT ( 'NONE',  ( 13.58437500061451786, 4.119189519843966529, 2.378215178124999607 ) ) ;
#62442 = CARTESIAN_POINT ( 'NONE',  ( 11.24062500061451608, 6.054752690667223547, 3.707466751127219781E-16 ) ) ;
#62443 = CARTESIAN_POINT ( 'NONE',  ( 4.734375000614518214, -4.541064518000419881, 2.621784821874995952 ) ) ;
#62444 = CARTESIAN_POINT ( 'NONE',  ( 5.334375000614517859, 6.421520780324663323E-16, -5.243569643749999010 ) ) ;
#62445 = ORIENTED_EDGE ( 'NONE', *, *, #2787, .F. ) ;
#62446 = CARTESIAN_POINT ( 'NONE',  ( 25.95937500061451431, -4.541064518000417216, -2.621784821875001281 ) ) ;
#62447 = CARTESIAN_POINT ( 'NONE',  ( 16.04062500061451857, -3.027376345333610441, -5.243569643749999898 ) ) ;
#62448 = CARTESIAN_POINT ( 'NONE',  ( 26.81250000122903288, 4.330127018922192761, -2.499999999999997780 ) ) ;
#62449 = CARTESIAN_POINT ( 'NONE',  ( 27.47812500061451502, 4.541064518000418104, 2.621784821874999949 ) ) ;
#62450 = CARTESIAN_POINT ( 'NONE',  ( 22.32187500061451502, -6.054752690667223547, -1.112240025338166033E-15 ) ) ;
#62451 = CARTESIAN_POINT ( 'NONE',  ( 16.79062500061451857, -3.027376345333614438, 5.243569643749998122 ) ) ;
#62452 = CARTESIAN_POINT ( 'NONE',  ( -4.243569643749999898, 19.37187500061451928, 27.54997392385601529 ) ) ;
#62453 = CARTESIAN_POINT ( 'NONE',  ( 22.90312500061451573, 4.541064518000418104, -2.621784821874998173 ) ) ;
#62454 = CARTESIAN_POINT ( 'NONE',  ( 3.487500001229035362, 4.330127018922191873, 2.499999999999999556 ) ) ;
#62455 = ORIENTED_EDGE ( 'NONE', *, *, #14420, .T. ) ;
#62456 = CARTESIAN_POINT ( 'NONE',  ( 28.53749999999999787, 5.773502691896255534, 3.535250795749688894E-16 ) ) ;
#62457 = CARTESIAN_POINT ( 'NONE',  ( -3.999999999999997335, 13.73749999999999893, -27.69059892324149175 ) ) ;
#62458 = CARTESIAN_POINT ( 'NONE',  ( 3.756430356250000546, 18.19062499938548427, 27.83122392262697886 ) ) ;
#62459 = CARTESIAN_POINT ( 'NONE',  ( 29.01562500061451644, -6.054752690667223547, -1.112240025338166033E-15 ) ) ;
#62460 = CARTESIAN_POINT ( 'NONE',  ( 10.79062500061451679, 6.054752690667223547, 3.707466751127219781E-16 ) ) ;
#62461 = CARTESIAN_POINT ( 'NONE',  ( 22.27500000122903145, 2.886751345948129099, -4.999999999999998224 ) ) ;
#62462 = CARTESIAN_POINT ( 'NONE',  ( 12.42187500061451821, -6.054752690667223547, -1.112240025338166033E-15 ) ) ;
#62463 = CARTESIAN_POINT ( 'NONE',  ( 26.54062500061451146, 6.054752690667223547, 3.707466751127219781E-16 ) ) ;
#62464 = CARTESIAN_POINT ( 'NONE',  ( 26.58750000000000213, -2.886751345948125991, -5.000000000000000000 ) ) ;
#62465 = CARTESIAN_POINT ( 'NONE',  ( -3.999999999999999112, 17.86250000122903359, -30.00000000000000000 ) ) ;
#62466 = DIRECTION ( 'NONE',  ( -1.000000000000000000, -0.000000000000000000, -0.000000000000000000 ) ) ;
#62467 = CARTESIAN_POINT ( 'NONE',  ( 13.75312500061451715, -4.541064518000417216, -2.621784821875001281 ) ) ;
#62468 =( BOUNDED_CURVE ( )  B_SPLINE_CURVE ( 2, ( #59654, #42314, #15321, #70748, #65570, #36765, #9063, #26051, #3897 ),
 .UNSPECIFIED., .F., .F. ) 
 B_SPLINE_CURVE_WITH_KNOTS ( ( 3, 2, 2, 2, 3 ),
 ( 0.01388888888888888985, 0.01851851851851851749, 0.02777777777777777624, 0.03703703703703703498, 0.04166666666666667129 ),
 .UNSPECIFIED. ) 
 CURVE ( )  GEOMETRIC_REPRESENTATION_ITEM ( )  RATIONAL_B_SPLINE_CURVE ( ( 0.9330127018922194093, 0.9330127018922194093, 1.000000000000000000, 0.8660254037844387076, 1.000000000000000000, 0.8660254037844387076, 1.000000000000000000, 0.9330127018922191873, 0.9330127018922192983 ) ) 
 REPRESENTATION_ITEM ( '' )  );
#62469 = ORIENTED_EDGE ( 'NONE', *, *, #46996, .F. ) ;
#62470 = CARTESIAN_POINT ( 'NONE',  ( 6.590625000614518392, -3.027376345333610441, -5.243569643749999898 ) ) ;
#62471 = CARTESIAN_POINT ( 'NONE',  ( 5.728125000614515905, 6.421520780324663323E-16, -5.243569643749999010 ) ) ;
#62472 = CARTESIAN_POINT ( 'NONE',  ( 16.54687500061451644, -2.746126346562642428, -4.756430356249999214 ) ) ;
#62473 = CARTESIAN_POINT ( 'NONE',  ( 2.812500001229033320, -4.330127018922190985, -2.500000000000001332 ) ) ;
#62474 = CARTESIAN_POINT ( 'NONE',  ( 14.84999999999999964, -4.330127018922190985, -2.500000000000001332 ) ) ;
#62475 = CARTESIAN_POINT ( 'NONE',  ( 16.28437500061452070, 4.541064518000418104, 2.621784821874999949 ) ) ;
#62476 = CARTESIAN_POINT ( 'NONE',  ( 10.20000000122903572, 5.773502691896255534, 3.535250795749688894E-16 ) ) ;
#62477 = CARTESIAN_POINT ( 'NONE',  ( 19.65937500061451360, -4.541064518000417216, -2.621784821875001281 ) ) ;
#62478 = CARTESIAN_POINT ( 'NONE',  ( 16.80000000000000071, 4.330127018922192761, -2.499999999999997780 ) ) ;
#62479 = CARTESIAN_POINT ( 'NONE',  ( 20.93437500061451573, -4.541064518000419881, 2.621784821874995952 ) ) ;
#62480 = CARTESIAN_POINT ( 'NONE',  ( -4.243569643749999898, 14.40312500061451750, -30.00000000000000000 ) ) ;
#62481 = DIRECTION ( 'NONE',  ( -1.000000000000000000, -0.000000000000000000, -0.000000000000000000 ) ) ;
#62482 = CARTESIAN_POINT ( 'NONE',  ( 24.75937500061451502, 2.746126346562643317, 4.756430356249998326 ) ) ;
#62483 = CARTESIAN_POINT ( 'NONE',  ( 3.999999999999998668, 11.71250000000000036, -32.30940107675850470 ) ) ;
#62484 = CARTESIAN_POINT ( 'NONE',  ( 26.54062500061451146, 6.054752690667223547, 3.707466751127219781E-16 ) ) ;
#62485 = CARTESIAN_POINT ( 'NONE',  ( -1.999999999999997113, 19.62500000000000000, -26.53589838486224295 ) ) ;
#62486 = CARTESIAN_POINT ( 'NONE',  ( 29.63437500061451502, 6.421520780324663323E-16, -5.243569643749999010 ) ) ;
#62487 = CARTESIAN_POINT ( 'NONE',  ( 24.03750000000000142, 5.773502691896255534, 3.535250795749688894E-16 ) ) ;
#62488 = CARTESIAN_POINT ( 'NONE',  ( 6.065625000614516260, -6.054752690667223547, -1.112240025338166033E-15 ) ) ;
#62489 = CARTESIAN_POINT ( 'NONE',  ( 23.89687500061451431, 0.000000000000000000, 4.756430356249998326 ) ) ;
#62490 = CARTESIAN_POINT ( 'NONE',  ( 18.45937500061451431, 4.541064518000418104, -2.621784821874998173 ) ) ;
#62491 = CARTESIAN_POINT ( 'NONE',  ( 10.35937500061451644, 2.746126346562643317, 4.756430356249998326 ) ) ;
#62492 = CARTESIAN_POINT ( 'NONE',  ( 5.465625000614517504, 3.027376345333611329, 5.243569643749999010 ) ) ;
#62493 = CARTESIAN_POINT ( 'NONE',  ( 11.55937500061451928, -4.541064518000417216, -2.621784821875001281 ) ) ;
#62494 = ORIENTED_EDGE ( 'NONE', *, *, #54021, .T. ) ;
#62495 = CARTESIAN_POINT ( 'NONE',  ( 20.44687500061451857, -3.027376345333614438, 5.243569643749998122 ) ) ;
#62496 = CARTESIAN_POINT ( 'NONE',  ( -1.626862140677534273E-15, 15.93124999877096748, 34.00000000000000000 ) ) ;
#62497 = CARTESIAN_POINT ( 'NONE',  ( 28.12499999999999645, 4.330127018922191873, 2.499999999999999556 ) ) ;
#62498 = CARTESIAN_POINT ( 'NONE',  ( 28.92187500061451644, 3.027376345333611329, 5.243569643749999010 ) ) ;
#62499 = LINE ( 'NONE', #5271, #53758 ) ;
#62500 = CARTESIAN_POINT ( 'NONE',  ( 3.403125000614518836, -4.541064518000417216, -2.621784821875001281 ) ) ;
#62501 = ORIENTED_EDGE ( 'NONE', *, *, #15601, .F. ) ;
#62502 = CARTESIAN_POINT ( 'NONE',  ( 9.525000000000002132, 6.123233995736764310E-16, -4.999999999999998224 ) ) ;
#62503 = CARTESIAN_POINT ( 'NONE',  ( 13.39687500061451431, 4.119189519843966529, -2.378215178124998275 ) ) ;
#62504 = CARTESIAN_POINT ( 'NONE',  ( 23.35312500061451857, 4.541064518000418104, -2.621784821874998173 ) ) ;
#62505 = CARTESIAN_POINT ( 'NONE',  ( 15.26249999999999929, -5.773502691896255534, -1.060575238724906372E-15 ) ) ;
#62506 = CARTESIAN_POINT ( 'NONE',  ( 11.43750000122903465, 6.123233995736764310E-16, -4.999999999999998224 ) ) ;
#62507 = CARTESIAN_POINT ( 'NONE',  ( 9.740625000614516082, -3.027376345333610441, -5.243569643749999898 ) ) ;
#62508 = ADVANCED_FACE ( 'NONE', ( #38134 ), #72560, .T. ) ;
#62509 = CARTESIAN_POINT ( 'NONE',  ( 8.737500000000002487, 5.773502691896255534, 3.535250795749688894E-16 ) ) ;
#62510 = CYLINDRICAL_SURFACE ( 'NONE', #22993, 4.000000000000000000 ) ;
#62511 = CARTESIAN_POINT ( 'NONE',  ( 28.23750000122903359, 4.330127018922191873, 2.499999999999999556 ) ) ;
#62512 = CARTESIAN_POINT ( 'NONE',  ( -7.967954043666661671E-16, 16.57812499938548356, 34.33755215474603517 ) ) ;
#62513 = CARTESIAN_POINT ( 'NONE',  ( 7.687500000000000000, -2.886751345948125991, -5.000000000000000000 ) ) ;
#62514 = DIRECTION ( 'NONE',  ( 0.000000000000000000, 0.000000000000000000, 1.000000000000000000 ) ) ;
#62515 = ORIENTED_EDGE ( 'NONE', *, *, #66601, .T. ) ;
#62516 = CARTESIAN_POINT ( 'NONE',  ( 21.51562500061451644, 3.027376345333613106, -5.243569643749998122 ) ) ;
#62517 = CARTESIAN_POINT ( 'NONE',  ( 28.22812500061451502, 6.421520780324663323E-16, -5.243569643749999010 ) ) ;
#62518 = CARTESIAN_POINT ( 'NONE',  ( 29.18437500061451573, 6.421520780324663323E-16, -5.243569643749999010 ) ) ;
#62519 = AXIS2_PLACEMENT_3D ( 'NONE', #17857, #23413, #57749 ) ;
#62520 = CARTESIAN_POINT ( 'NONE',  ( 19.13437500061451857, -4.541064518000419881, 2.621784821874995952 ) ) ;
#62521 = CARTESIAN_POINT ( 'NONE',  ( 16.11562500061451786, 3.027376345333613106, -5.243569643749998122 ) ) ;
#62522 = CARTESIAN_POINT ( 'NONE',  ( -4.243569643749998122, 10.84062500061459211, -27.54997392385601174 ) ) ;
#62523 = CARTESIAN_POINT ( 'NONE',  ( 5.315625000614516260, 3.027376345333613106, -5.243569643749998122 ) ) ;
#62524 = CARTESIAN_POINT ( 'NONE',  ( 29.32500000122903216, -5.773502691896255534, -1.060575238724906372E-15 ) ) ;
#62525 = CARTESIAN_POINT ( 'NONE',  ( 22.69687500061451857, -2.746126346562646425, 4.756430356249996549 ) ) ;
#62526 = CARTESIAN_POINT ( 'NONE',  ( 18.44062500061451715, 6.054752690667223547, 3.707466751127219781E-16 ) ) ;
#62527 = CARTESIAN_POINT ( 'NONE',  ( 25.10625000122903216, 0.000000000000000000, 4.999999999999998224 ) ) ;
#62528 = CARTESIAN_POINT ( 'NONE',  ( 3.712500001229034563, -4.330127018922190985, -2.500000000000001332 ) ) ;
#62529 = CARTESIAN_POINT ( 'NONE',  ( 12.23437500061451821, 4.541064518000418104, 2.621784821874999949 ) ) ;
#62530 = CARTESIAN_POINT ( 'NONE',  ( 10.92187500061451644, 3.027376345333611329, 5.243569643749999010 ) ) ;
#62531 = CARTESIAN_POINT ( 'NONE',  ( 20.10937500061451289, -4.541064518000417216, -2.621784821875001281 ) ) ;
#62532 = ORIENTED_EDGE ( 'NONE', *, *, #16952, .F. ) ;
#62533 = CARTESIAN_POINT ( 'NONE',  ( -2.698377630233220081, 9.636255672932170668, 24.62661337867154288 ) ) ;
#62534 = CARTESIAN_POINT ( 'NONE',  ( 23.50312500061451360, 0.000000000000000000, 5.243569643749999010 ) ) ;
#62535 = CARTESIAN_POINT ( 'NONE',  ( 18.83437500061451431, 6.421520780324663323E-16, -5.243569643749999010 ) ) ;
#62536 = CARTESIAN_POINT ( 'NONE',  ( 24.62812500061451715, 6.421520780324663323E-16, -5.243569643749999010 ) ) ;
#62537 = CARTESIAN_POINT ( 'NONE',  ( -5.810221930991193690E-16, 12.23750000000000071, -34.00000000000000000 ) ) ;
#62538 = CARTESIAN_POINT ( 'NONE',  ( -3.999999999999999556, 16.81250000000000000, 27.69059892324149530 ) ) ;
#62539 = CARTESIAN_POINT ( 'NONE',  ( 29.80312500061451431, 0.000000000000000000, 5.243569643749999010 ) ) ;
#62540 = CARTESIAN_POINT ( 'NONE',  ( 11.17500000122903536, 2.886751345948126879, 4.999999999999999112 ) ) ;
#62541 = CARTESIAN_POINT ( 'NONE',  ( 7.762500001229033053, -4.330127018922190985, -2.500000000000001332 ) ) ;
#62542 = CARTESIAN_POINT ( 'NONE',  ( 28.83750000122903145, -4.330127018922194537, 2.499999999999995559 ) ) ;
#62543 = CARTESIAN_POINT ( 'NONE',  ( 26.81250000122903288, 4.330127018922192761, -2.499999999999997780 ) ) ;
#62544 = CARTESIAN_POINT ( 'NONE',  ( -2.000000000000001776, 18.59374999877096357, 33.46410161513775705 ) ) ;
#62545 = CARTESIAN_POINT ( 'NONE',  ( 15.46875000122903110, 2.886751345948129099, -4.999999999999998224 ) ) ;
#62546 = CARTESIAN_POINT ( 'NONE',  ( 8.896875000614517859, -3.027376345333610441, -5.243569643749999898 ) ) ;
#62547 = PRODUCT_RELATED_PRODUCT_CATEGORY ( 'part', '', ( #14280 ) ) ;
#62548 = CARTESIAN_POINT ( 'NONE',  ( 29.41875000122903216, 2.886751345948139313, -4.999999999999980460 ) ) ;
#62549 = CARTESIAN_POINT ( 'NONE',  ( 16.26562500061451289, 3.027376345333611329, 5.243569643749999010 ) ) ;
#62550 = CARTESIAN_POINT ( 'NONE',  ( 12.38437500061451857, -4.541064518000419881, 2.621784821874995952 ) ) ;
#62551 = CARTESIAN_POINT ( 'NONE',  ( 28.61250000122903359, 4.330127018922192761, -2.499999999999997780 ) ) ;
#62552 = CARTESIAN_POINT ( 'NONE',  ( 20.10937500061451289, -4.541064518000417216, -2.621784821875001281 ) ) ;
#62553 = CARTESIAN_POINT ( 'NONE',  ( 6.309375000614517504, 4.541064518000418104, -2.621784821874998173 ) ) ;
#62554 = CARTESIAN_POINT ( 'NONE',  ( 3.253125000614518036, 0.000000000000000000, 5.243569643749999010 ) ) ;
#62555 = CARTESIAN_POINT ( 'NONE',  ( 5.737499999999998934, -2.886751345948063374, 5.000000000000112799 ) ) ;
#62556 = CARTESIAN_POINT ( 'NONE',  ( 9.178125000614517859, -4.541064518000419881, 2.621784821874995952 ) ) ;
#62557 = CARTESIAN_POINT ( 'NONE',  ( 21.10312500061451502, 4.541064518000418104, -2.621784821874998173 ) ) ;
#62558 = ORIENTED_EDGE ( 'NONE', *, *, #66024, .T. ) ;
#62559 = CARTESIAN_POINT ( 'NONE',  ( 4.987500001229032698, -4.330127018922194537, 2.499999999999995559 ) ) ;
#62560 = CARTESIAN_POINT ( 'NONE',  ( 17.95312500061451644, 4.541064518000418104, -2.621784821874998173 ) ) ;
#62561 = CARTESIAN_POINT ( 'NONE',  ( 14.01562500061451644, 3.027376345333611329, 5.243569643749999010 ) ) ;
#62562 = CARTESIAN_POINT ( 'NONE',  ( 24.72187500061451360, 2.746126346562645981, -4.756430356249997438 ) ) ;
#62563 = CARTESIAN_POINT ( 'NONE',  ( 12.82499999999999929, 4.330127018922191873, 2.499999999999999556 ) ) ;
#62564 = CARTESIAN_POINT ( 'NONE',  ( 8.212500001229035007, -4.330127018922190985, -2.500000000000001332 ) ) ;
#62565 = CARTESIAN_POINT ( 'NONE',  ( 5.315625000614516260, 3.027376345333613106, -5.243569643749998122 ) ) ;
#62566 = EDGE_CURVE ( 'NONE', #23474, #26902, #41318, .T. ) ;
#62567 = CARTESIAN_POINT ( 'NONE',  ( 18.86250000122903359, 0.000000000000000000, 4.999999999999998224 ) ) ;
#62568 = CARTESIAN_POINT ( 'NONE',  ( 26.88749999999999574, -2.886751345948129988, 4.999999999999997335 ) ) ;
#62569 = EDGE_CURVE ( 'NONE', #964, #48607, #6959, .T. ) ;
#62570 = CARTESIAN_POINT ( 'NONE',  ( -2.121784821874999949, 12.13437500061451857, -33.67503911421598417 ) ) ;
#62571 = CARTESIAN_POINT ( 'NONE',  ( 1.626862140677534273E-15, 16.17500000122903359, 34.00000000000000000 ) ) ;
#62572 = CARTESIAN_POINT ( 'NONE',  ( 2.700000001229035718, -2.886751345948129988, 4.999999999999997335 ) ) ;
#62573 = CARTESIAN_POINT ( 'NONE',  ( 1.071796769724488785, 14.65759618943233455, 34.00000000000000000 ) ) ;
#62574 = CARTESIAN_POINT ( 'NONE',  ( 18.53437500061451715, 4.541064518000418104, 2.621784821874999949 ) ) ;
#62575 = EDGE_CURVE ( 'NONE', #10639, #72600, #64239, .T. ) ;
#62576 = CARTESIAN_POINT ( 'NONE',  ( 16.67812500061451786, 4.541064518000418104, 2.621784821874999949 ) ) ;
#62577 = CARTESIAN_POINT ( 'NONE',  ( 10.03125000122903288, 6.123233995736764310E-16, -4.999999999999998224 ) ) ;
#62578 = CARTESIAN_POINT ( 'NONE',  ( 3.999999999999998668, 16.51249999999999929, 32.30940107675850470 ) ) ;
#62579 = CARTESIAN_POINT ( 'NONE',  ( 29.85937500061451644, 0.000000000000000000, 5.243569643749999010 ) ) ;
#62580 = CARTESIAN_POINT ( 'NONE',  ( 26.82187500061451857, -6.054752690667223547, -1.112240025338166033E-15 ) ) ;
#62581 = CARTESIAN_POINT ( 'NONE',  ( 18.12187500061451928, -4.119189519843968306, 2.378215178124996054 ) ) ;
#62582 = CARTESIAN_POINT ( 'NONE',  ( 12.81562500061451537, -6.054752690667223547, -1.112240025338166033E-15 ) ) ;
#62583 = CARTESIAN_POINT ( 'NONE',  ( 11.37187500061451750, 3.027376345333611329, 5.243569643749999010 ) ) ;
#62584 = ORIENTED_EDGE ( 'NONE', *, *, #30725, .T. ) ;
#62585 = CARTESIAN_POINT ( 'NONE',  ( 28.94062500061452070, -3.027376345333614438, 5.243569643749998122 ) ) ;
#62586 = CARTESIAN_POINT ( 'NONE',  ( 19.79062500061451502, 6.054752690667223547, 3.707466751127219781E-16 ) ) ;
#62587 = FACE_OUTER_BOUND ( 'NONE', #45562, .T. ) ;
#62588 = EDGE_CURVE ( 'NONE', #59726, #2356, #3299, .T. ) ;
#62589 = CARTESIAN_POINT ( 'NONE',  ( 20.47500000000000142, 4.330127018922191873, 2.499999999999999556 ) ) ;
#62590 = CARTESIAN_POINT ( 'NONE',  ( 10.91250000000000320, 2.886751345948129099, -4.999999999999998224 ) ) ;
#62591 = CARTESIAN_POINT ( 'NONE',  ( 21.33750000122903145, 6.123233995736764310E-16, -4.999999999999998224 ) ) ;
#62592 = CARTESIAN_POINT ( 'NONE',  ( 15.32812500061451644, 4.541064518000418104, 2.621784821874999949 ) ) ;
#62593 = CARTESIAN_POINT ( 'NONE',  ( 12.34687500061451537, -4.119189519843965641, -2.378215178125001383 ) ) ;
#62594 = ORIENTED_EDGE ( 'NONE', *, *, #56020, .T. ) ;
#62595 = CARTESIAN_POINT ( 'NONE',  ( 20.10000000000000142, 0.000000000000000000, 4.999999999999998224 ) ) ;
#62596 = CARTESIAN_POINT ( 'NONE',  ( 21.18749999999999645, -2.886751345948125991, -5.000000000000000000 ) ) ;
#62597 = CARTESIAN_POINT ( 'NONE',  ( 21.90937500061451715, -4.541064518000417216, -2.621784821875001281 ) ) ;
#62598 = CARTESIAN_POINT ( 'NONE',  ( 25.64062500061451644, 6.054752690667223547, 3.707466751127219781E-16 ) ) ;
#62599 = ORIENTED_EDGE ( 'NONE', *, *, #4648, .T. ) ;
#62600 = CARTESIAN_POINT ( 'NONE',  ( 13.76250000000000107, 2.886751345948126879, 4.999999999999998224 ) ) ;
#62601 = CARTESIAN_POINT ( 'NONE',  ( 7.528125000614515727, 6.421520780324663323E-16, -5.243569643749999010 ) ) ;
#62602 = CARTESIAN_POINT ( 'NONE',  ( 3.999999999999999112, 12.12500000000000000, 30.00000000000000000 ) ) ;
#62603 = CARTESIAN_POINT ( 'NONE',  ( 14.02499999999999858, 6.123233995736764310E-16, -4.999999999999998224 ) ) ;
#62604 = CARTESIAN_POINT ( 'NONE',  ( 4.243569643749999898, 16.84062500061451573, 32.45002607614398471 ) ) ;
#62605 = CARTESIAN_POINT ( 'NONE',  ( 29.12812500061451715, 6.421520780324663323E-16, -5.243569643749999010 ) ) ;
#62606 = CARTESIAN_POINT ( 'NONE',  ( 25.84687500061451360, -3.027376345333614438, 5.243569643749998122 ) ) ;
#62607 = VERTEX_POINT ( 'NONE', #53528 ) ;
#62608 = CARTESIAN_POINT ( 'NONE',  ( 23.50312500061451360, 0.000000000000000000, 5.243569643749999010 ) ) ;
#62609 = CARTESIAN_POINT ( 'NONE',  ( 24.12187500061451217, -6.054752690667223547, -1.112240025338166033E-15 ) ) ;
#62610 = CARTESIAN_POINT ( 'NONE',  ( 4.243569643749999010, 17.81562500061459176, -32.45002607614398471 ) ) ;
#62611 = CARTESIAN_POINT ( 'NONE',  ( 10.98750000000000071, 5.773502691896255534, 3.535250795749688894E-16 ) ) ;
#62612 = CARTESIAN_POINT ( 'NONE',  ( 9.403125000614517504, 4.541064518000418104, -2.621784821874998173 ) ) ;
#62613 = CARTESIAN_POINT ( 'NONE',  ( 29.16562500061451502, 3.027376345333613106, -5.243569643749998122 ) ) ;
#62614 = CARTESIAN_POINT ( 'NONE',  ( 26.80312500061451431, -4.541064518000417216, -2.621784821875001281 ) ) ;
#62615 = CARTESIAN_POINT ( 'NONE',  ( 29.48437500061451644, -2.746126346562641984, -4.756430356249999214 ) ) ;
#62616 = CARTESIAN_POINT ( 'NONE',  ( 13.43437500061451750, 5.824947211148865298E-16, -4.756430356249998326 ) ) ;
#62617 = CARTESIAN_POINT ( 'NONE',  ( 18.90937500061451360, 4.541064518000418104, -2.621784821874998173 ) ) ;
#62619 = CARTESIAN_POINT ( 'NONE',  ( -2.121784821874996840, 13.18437500061451750, 33.67503911421598417 ) ) ;
#62618 =( BOUNDED_CURVE ( )  B_SPLINE_CURVE ( 2, ( #68636, #62356, #53727, #34269, #63075, #46461, #40557 ),
 .UNSPECIFIED., .F., .F. ) 
 B_SPLINE_CURVE_WITH_KNOTS ( ( 3, 2, 2, 3 ),
 ( 0.9514681797180121192, 0.9527777777777777235, 0.9555555555555556024, 0.9567451072665406064 ),
 .UNSPECIFIED. ) 
 CURVE ( )  GEOMETRIC_REPRESENTATION_ITEM ( )  RATIONAL_B_SPLINE_CURVE ( ( 0.9332310268437209455, 0.9368369663457591923, 1.000000000000000000, 0.8660254037844387076, 1.000000000000000000, 0.9426269043435712147, 0.9343925588410226801 ) ) 
 REPRESENTATION_ITEM ( '' )  );
#62620 = CARTESIAN_POINT ( 'NONE',  ( 20.40937500061451715, 0.000000000000000000, 5.243569643749999010 ) ) ;
#62622 = EDGE_CURVE ( 'NONE', #11718, #49995, #3664, .T. ) ;
#62621 = CARTESIAN_POINT ( 'NONE',  ( 27.30937500061451573, -4.541064518000417216, -2.621784821875001281 ) ) ;
#62623 = CARTESIAN_POINT ( 'NONE',  ( -4.243569643749999898, 16.70937500061451786, 30.00000000000000000 ) ) ;
#62624 = CARTESIAN_POINT ( 'NONE',  ( 7.115625000614516082, 3.027376345333613106, -5.243569643749998122 ) ) ;
#62625 = CARTESIAN_POINT ( 'NONE',  ( -3.999999999999997335, 18.23750000000000071, -27.69059892324149530 ) ) ;
#62626 = CARTESIAN_POINT ( 'NONE',  ( 5.184375000614516615, -4.541064518000419881, 2.621784821874995952 ) ) ;
#62627 = CARTESIAN_POINT ( 'NONE',  ( -2.000000000000000000, 15.98750000122903181, -33.46410161513775705 ) ) ;
#62628 = CARTESIAN_POINT ( 'NONE',  ( 6.703125000614516438, 4.541064518000418104, -2.621784821874998173 ) ) ;
#62629 = CARTESIAN_POINT ( 'NONE',  ( 10.88437500061451679, 4.541064518000418104, 2.621784821874999949 ) ) ;
#62630 =( NAMED_UNIT ( * ) SI_UNIT ( $, .STERADIAN. ) SOLID_ANGLE_UNIT ( ) );
#62631 = CARTESIAN_POINT ( 'NONE',  ( 18.48750000122903359, -4.330127018922194537, 2.499999999999995559 ) ) ;
#62632 = CARTESIAN_POINT ( 'NONE',  ( 6.234375000614519102, 6.421520780324663323E-16, -5.243569643749999010 ) ) ;
#62633 = CARTESIAN_POINT ( 'NONE',  ( 7.678125000614516082, 4.541064518000418104, 2.621784821874999949 ) ) ;
#62634 = CARTESIAN_POINT ( 'NONE',  ( 22.33125000122903003, 4.330127018922191873, 2.499999999999999556 ) ) ;
#62635 = CARTESIAN_POINT ( 'NONE',  ( 15.83437500061451608, 4.541064518000418104, 2.621784821874999949 ) ) ;
#62636 = DIRECTION ( 'NONE',  ( -1.000000000000000000, 0.000000000000000000, 0.000000000000000000 ) ) ;
#62637 = ORIENTED_EDGE ( 'NONE', *, *, #4430, .F. ) ;
#62638 = CARTESIAN_POINT ( 'NONE',  ( 25.67812500061451431, 4.541064518000418104, 2.621784821874999949 ) ) ;
#62639 = CARTESIAN_POINT ( 'NONE',  ( 11.65312500061451573, 4.541064518000418104, -2.621784821874998173 ) ) ;
#62640 = CARTESIAN_POINT ( 'NONE',  ( 27.15937500061451360, 0.000000000000000000, 5.243569643749999010 ) ) ;
#62641 = CARTESIAN_POINT ( 'NONE',  ( 10.49062500061451431, -3.027376345333614438, 5.243569643749998122 ) ) ;
#62642 = CARTESIAN_POINT ( 'NONE',  ( 1.592000809091587073E-14, 15.05000000122903714, -34.00000000000000000 ) ) ;
#62643 = CARTESIAN_POINT ( 'NONE',  ( 12.60000000122903430, -2.886751345948129988, 4.999999999999997335 ) ) ;
#62644 = CARTESIAN_POINT ( 'NONE',  ( 28.34062500061451928, 6.054752690667223547, 3.707466751127219781E-16 ) ) ;
#62645 = CARTESIAN_POINT ( 'NONE',  ( 4.243569643749999898, 12.34062500061451750, -27.54997392385601529 ) ) ;
#62646 = CARTESIAN_POINT ( 'NONE',  ( 12.93750000122903465, 4.330127018922191873, 2.499999999999999556 ) ) ;
#62647 = CARTESIAN_POINT ( 'NONE',  ( 11.77500000000000036, 6.123233995736764310E-16, -4.999999999999998224 ) ) ;
#62648 = CARTESIAN_POINT ( 'NONE',  ( 19.67812500061451786, 6.421520780324663323E-16, -5.243569643749999010 ) ) ;
#62649 = CARTESIAN_POINT ( 'NONE',  ( 8.784375000614518925, -4.541064518000419881, 2.621784821874995952 ) ) ;
#62650 = CARTESIAN_POINT ( 'NONE',  ( 20.40000000000000213, 4.330127018922192761, -2.499999999999997780 ) ) ;
#62651 = CARTESIAN_POINT ( 'NONE',  ( 8.212500001229035007, -4.330127018922190985, -2.500000000000001332 ) ) ;
#62652 = CARTESIAN_POINT ( 'NONE',  ( 16.87500000122903288, 2.886751345948129099, -4.999999999999998224 ) ) ;
#62653 = CARTESIAN_POINT ( 'NONE',  ( 14.01562500061451644, 3.027376345333611329, 5.243569643749999010 ) ) ;
#62654 = AXIS2_PLACEMENT_3D ( 'NONE', #13605, #69420, #35062 ) ;
#62655 = CARTESIAN_POINT ( 'NONE',  ( 16.41562500061451857, -6.054752690667223547, -1.112240025338166033E-15 ) ) ;
#62656 = CARTESIAN_POINT ( 'NONE',  ( 24.52500000122903145, 2.886751345948129099, -4.999999999999998224 ) ) ;
#62657 = CARTESIAN_POINT ( 'NONE',  ( 21.11249999999999716, -5.773502691896255534, -1.060575238724906372E-15 ) ) ;
#62658 = CARTESIAN_POINT ( 'NONE',  ( 23.74687500061451573, -3.027376345333610441, -5.243569643749999898 ) ) ;
#62659 = CARTESIAN_POINT ( 'NONE',  ( 45.00000000000000000, 0.000000000000000000, 0.000000000000000000 ) ) ;
#62660 = CARTESIAN_POINT ( 'NONE',  ( 9.150000001229033231, -2.886751345948125991, -5.000000000000000000 ) ) ;
#62661 = CARTESIAN_POINT ( 'NONE',  ( 9.909375000614517148, 4.541064518000418104, -2.621784821874998173 ) ) ;
#62662 = CARTESIAN_POINT ( 'NONE',  ( 28.62187500061451573, -6.054752690667223547, -1.112240025338166033E-15 ) ) ;
#62663 = ADVANCED_FACE ( 'NONE', ( #20262, #20629 ), #30628, .T. ) ;
#62664 =( BOUNDED_CURVE ( )  B_SPLINE_CURVE ( 2, ( #44177, #66707, #61876, #205, #50447, #16080, #10548 ),
 .UNSPECIFIED., .F., .F. ) 
 B_SPLINE_CURVE_WITH_KNOTS ( ( 3, 2, 2, 3 ),
 ( 0.4500000000000001221, 0.4527777777777778345, 0.4555555555555555469, 0.4583333333333332593 ),
 .UNSPECIFIED. ) 
 CURVE ( )  GEOMETRIC_REPRESENTATION_ITEM ( )  RATIONAL_B_SPLINE_CURVE ( ( 0.9999999999999946709, 0.8660254037844440367, 1.000000000000000000, 0.8660254037844387076, 1.000000000000000000, 0.8660254037844413721, 0.9999999999999973355 ) ) 
 REPRESENTATION_ITEM ( '' )  );
#62665 = CARTESIAN_POINT ( 'NONE',  ( 4.226174930415019126, -2.672125389006213325, -4.285040371159579031 ) ) ;
#62666 = CARTESIAN_POINT ( 'NONE',  ( 23.57812500061451289, -4.541064518000419881, 2.621784821874995952 ) ) ;
#62667 = CARTESIAN_POINT ( 'NONE',  ( 25.65937500061451715, 4.541064518000418104, -2.621784821874998173 ) ) ;
#62668 = CARTESIAN_POINT ( 'NONE',  ( -1.878215178124999163, 13.80312499938548321, 26.74683588394047007 ) ) ;
#62669 = CARTESIAN_POINT ( 'NONE',  ( 7.837499999999999467, 5.773502691896255534, 3.535250795749688401E-16 ) ) ;
#62670 = CARTESIAN_POINT ( 'NONE',  ( 7.134375000614516793, 6.421520780324663323E-16, -5.243569643749999010 ) ) ;
#62671 = CARTESIAN_POINT ( 'NONE',  ( 15.90000000000000036, 4.330127018922192761, -2.499999999999997780 ) ) ;
#62672 = CARTESIAN_POINT ( 'NONE',  ( 26.35312500061451857, -4.541064518000417216, -2.621784821875001281 ) ) ;
#62673 = CARTESIAN_POINT ( 'NONE',  ( 5.971875000614516260, 3.027376345333611329, 5.243569643749999010 ) ) ;
#62674 =( GEOMETRIC_REPRESENTATION_CONTEXT ( 3 ) GLOBAL_UNCERTAINTY_ASSIGNED_CONTEXT ( ( #7773 ) ) GLOBAL_UNIT_ASSIGNED_CONTEXT ( ( #51324, #67243, #39518 ) ) REPRESENTATION_CONTEXT ( 'NONE', 'WORKASPACE' ) );
#62675 = CARTESIAN_POINT ( 'NONE',  ( -2.000000000000000000, 16.43750000122903643, -33.46410161513775705 ) ) ;
#62676 = CARTESIAN_POINT ( 'NONE',  ( 25.54687500061451644, -3.027376345333610441, -5.243569643749999898 ) ) ;
#62677 = CARTESIAN_POINT ( 'NONE',  ( -4.243569643749999898, 10.76562500061459460, 27.54997392385601529 ) ) ;
#62678 = CARTESIAN_POINT ( 'NONE',  ( 16.61250000000000426, -5.773502691896255534, -1.060575238724906372E-15 ) ) ;
#62679 = ORIENTED_EDGE ( 'NONE', *, *, #45083, .F. ) ;
#62680 = CARTESIAN_POINT ( 'NONE',  ( 26.32499999999999929, 4.330127018922191873, 2.499999999999999556 ) ) ;
#62681 = CARTESIAN_POINT ( 'NONE',  ( 28.69687500061451502, -3.027376345333610441, -5.243569643749999898 ) ) ;
#62682 = ORIENTED_EDGE ( 'NONE', *, *, #2964, .F. ) ;
#62683 = CARTESIAN_POINT ( 'NONE',  ( 15.06562500061451537, -6.054752690667223547, -1.112240025338166033E-15 ) ) ;
#62684 = CARTESIAN_POINT ( 'NONE',  ( 6.853125000614516793, 0.000000000000000000, 5.243569643749999010 ) ) ;
#62685 = CARTESIAN_POINT ( 'NONE',  ( 18.53437500061451360, -2.746126346562646425, 4.756430356249996549 ) ) ;
#62686 = CARTESIAN_POINT ( 'NONE',  ( 5.184375000614516615, -4.541064518000419881, 2.621784821874995952 ) ) ;
#62687 = CARTESIAN_POINT ( 'NONE',  ( 14.47500000122903430, -5.773502691896255534, -1.060575238724906372E-15 ) ) ;
#62688 = CARTESIAN_POINT ( 'NONE',  ( 22.91249999999999432, -5.773502691896255534, -1.060575238724906372E-15 ) ) ;
#62689 = LINE ( 'NONE', #11725, #43306 ) ;
#62690 = CARTESIAN_POINT ( 'NONE',  ( 4.734375000614518214, -4.541064518000419881, 2.621784821874995952 ) ) ;
#62691 = CARTESIAN_POINT ( 'NONE',  ( 8.296875000614516438, -3.027376345333614438, 5.243569643749998122 ) ) ;
#62692 = CARTESIAN_POINT ( 'NONE',  ( 22.32187500061451502, -6.054752690667223547, -1.112240025338166033E-15 ) ) ;
#62693 = CARTESIAN_POINT ( 'NONE',  ( -3.999999999999999112, 17.26249999999999929, -32.30940107675850470 ) ) ;
#62694 = ORIENTED_EDGE ( 'NONE', *, *, #30819, .F. ) ;
#62695 = CARTESIAN_POINT ( 'NONE',  ( 3.759375000614517681, 0.000000000000000000, 5.243569643749999010 ) ) ;
#62697 = EDGE_CURVE ( 'NONE', #67289, #21751, #14496, .T. ) ;
#62696 = CARTESIAN_POINT ( 'NONE',  ( 6.796875000614516438, 6.054752690667223547, 3.707466751127219781E-16 ) ) ;
#62698 = CARTESIAN_POINT ( 'NONE',  ( 17.96250000000000213, -5.773502691896255534, -1.060575238724906372E-15 ) ) ;
#62699 = CARTESIAN_POINT ( 'NONE',  ( 16.19062500061451715, 6.054752690667223547, 3.707466751127219781E-16 ) ) ;
#62700 = CARTESIAN_POINT ( 'NONE',  ( -4.000000000000000000, 20.37500000000000000, 30.00000000000000000 ) ) ;
#62702 = CARTESIAN_POINT ( 'NONE',  ( -3.999999999999999112, 20.00000000000000000, 30.00000000000000000 ) ) ;
#62701 = VECTOR ( 'NONE', #45099, 1000.000000000000000 ) ;
#62703 = CARTESIAN_POINT ( 'NONE',  ( 18.87187500061451573, 2.746126346562645981, -4.756430356249997438 ) ) ;
#62704 = CARTESIAN_POINT ( 'NONE',  ( 9.440625000614517148, 6.054752690667223547, 3.707466751127219781E-16 ) ) ;
#62705 = CARTESIAN_POINT ( 'NONE',  ( 26.52187500061451431, 3.027376345333613106, -5.243569643749998122 ) ) ;
#62706 = FACE_OUTER_BOUND ( 'NONE', #4729, .T. ) ;
#62707 = CARTESIAN_POINT ( 'NONE',  ( 25.35937500061451644, 0.000000000000000000, 5.243569643749999010 ) ) ;
#62708 = CARTESIAN_POINT ( 'NONE',  ( 8.099999999999999645, -4.330127018922190985, -2.500000000000001332 ) ) ;
#62709 = CARTESIAN_POINT ( 'NONE',  ( -2.828200636599751609E-16, 12.80000000122903181, 25.38119784648299770 ) ) ;
#62710 = CARTESIAN_POINT ( 'NONE',  ( 7.762500001229033053, -4.330127018922190985, -2.500000000000001332 ) ) ;
#62711 = CARTESIAN_POINT ( 'NONE',  ( 19.39687500061451786, 6.054752690667223547, 3.707466751127219781E-16 ) ) ;
#62712 = CARTESIAN_POINT ( 'NONE',  ( 11.48437500061451644, -4.541064518000419881, 2.621784821874995952 ) ) ;
#62713 = CARTESIAN_POINT ( 'NONE',  ( -4.000165449326166467, 2.999779401354842445, -30.13373215374999603 ) ) ;
#62714 = ORIENTED_EDGE ( 'NONE', *, *, #34377, .F. ) ;
#62715 = CARTESIAN_POINT ( 'NONE',  ( 14.80312500061451608, 4.541064518000418104, -2.621784821874998173 ) ) ;
#62716 = CARTESIAN_POINT ( 'NONE',  ( 27.48750000122903359, -4.330127018922194537, 2.499999999999995559 ) ) ;
#62717 = CARTESIAN_POINT ( 'NONE',  ( 13.24687500061451750, -3.027376345333614438, 5.243569643749998122 ) ) ;
#62718 = CARTESIAN_POINT ( 'NONE',  ( 3.871875000614519280, -6.054752690667223547, -1.112240025338166033E-15 ) ) ;
#62719 = CARTESIAN_POINT ( 'NONE',  ( 14.54062500061451679, -3.027376345333614438, 5.243569643749998122 ) ) ;
#62720 = CARTESIAN_POINT ( 'NONE',  ( 26.43750000122903288, 4.330127018922191873, 2.499999999999999556 ) ) ;
#62721 = EDGE_CURVE ( 'NONE', #9134, #69337, #22054, .T. ) ;
#62722 = CARTESIAN_POINT ( 'NONE',  ( 26.25937500061451857, 0.000000000000000000, 5.243569643749999010 ) ) ;
#62723 = CARTESIAN_POINT ( 'NONE',  ( 2.226602359779148887, 9.751272476441998904, 25.29835638300850320 ) ) ;
#62724 = CARTESIAN_POINT ( 'NONE',  ( 12.97500000122903252, 2.886751345948126879, 4.999999999999999112 ) ) ;
#62725 = DIRECTION ( 'NONE',  ( -0.000000000000000000, -1.000000000000000000, -0.000000000000000000 ) ) ;
#62726 = CARTESIAN_POINT ( 'NONE',  ( -4.243569643749999898, 17.15937500061451715, -30.00000000000000000 ) ) ;
#62727 = CARTESIAN_POINT ( 'NONE',  ( 16.99687500061451573, -3.027376345333610441, -5.243569643749999898 ) ) ;
#62728 = CARTESIAN_POINT ( 'NONE',  ( 19.23750000122903714, 4.330127018922191873, 2.499999999999999556 ) ) ;
#62729 = CARTESIAN_POINT ( 'NONE',  ( 14.70937500061451786, -4.541064518000417216, -2.621784821875001281 ) ) ;
#62730 = CARTESIAN_POINT ( 'NONE',  ( 4.243569643749999898, 10.63437500061451857, 30.00000000000000000 ) ) ;
#62731 = CARTESIAN_POINT ( 'NONE',  ( 21.30000000122903359, -2.886751345948125991, -5.000000000000000000 ) ) ;
#62732 = CARTESIAN_POINT ( 'NONE',  ( 16.04062500061451857, -3.027376345333610441, -5.243569643749999898 ) ) ;
#62733 = CARTESIAN_POINT ( 'NONE',  ( 29.20312500061451644, 4.541064518000418104, -2.621784821874998173 ) ) ;
#62734 = ORIENTED_EDGE ( 'NONE', *, *, #65317, .T. ) ;
#62735 = ORIENTED_EDGE ( 'NONE', *, *, #29767, .F. ) ;
#62736 = CARTESIAN_POINT ( 'NONE',  ( 18.22499999999999787, 4.330127018922191873, 2.499999999999999556 ) ) ;
#62737 = CARTESIAN_POINT ( 'NONE',  ( 5.810221930991193690E-16, 18.40624999877096357, 26.00000000000000000 ) ) ;
#62738 = CARTESIAN_POINT ( 'NONE',  ( 3.403125000614518836, -4.541064518000417216, -2.621784821875001281 ) ) ;
#62739 = CARTESIAN_POINT ( 'NONE',  ( 15.52500000122903323, 2.886751345948129099, -4.999999999999998224 ) ) ;
#62740 = CARTESIAN_POINT ( 'NONE',  ( 20.99062500061451431, -3.027376345333610441, -5.243569643749999898 ) ) ;
#62741 = ADVANCED_FACE ( 'NONE', ( #64975 ), #70152, .F. ) ;
#62742 = CARTESIAN_POINT ( 'NONE',  ( 22.56562500061451715, 3.027376345333611329, 5.243569643749999010 ) ) ;
#62743 = CARTESIAN_POINT ( 'NONE',  ( 3.815625000614518036, -6.054752690667223547, -1.112240025338166033E-15 ) ) ;
#62744 = CARTESIAN_POINT ( 'NONE',  ( 27.63749999999999929, 5.773502691896255534, 3.535250795749688894E-16 ) ) ;
#62745 = CARTESIAN_POINT ( 'NONE',  ( 17.79375000122903572, 5.773502691896255534, 3.535250795749688401E-16 ) ) ;
#62746 = CARTESIAN_POINT ( 'NONE',  ( 8.259375000614518569, 0.000000000000000000, 4.756430356249998326 ) ) ;
#62747 = CARTESIAN_POINT ( 'NONE',  ( 29.44687500061451857, -3.027376345333614438, 5.243569643749998122 ) ) ;
#62748 = CARTESIAN_POINT ( 'NONE',  ( 2.000000000000001332, 12.16250000122903430, -26.53589838486224650 ) ) ;
#62749 = CARTESIAN_POINT ( 'NONE',  ( 2.121784821875001281, 16.40937500061452070, -26.32496088578401938 ) ) ;
#62750 = CARTESIAN_POINT ( 'NONE',  ( 6.825000001229034829, -5.773502691896255534, -1.060575238724906372E-15 ) ) ;
#62751 = CARTESIAN_POINT ( 'NONE',  ( 7.425000000000000711, 4.330127018922191873, 2.499999999999999556 ) ) ;
#62752 = CARTESIAN_POINT ( 'NONE',  ( 4.312500001229034652, 4.330127018922192761, -2.499999999999997780 ) ) ;
#62753 = CARTESIAN_POINT ( 'NONE',  ( 9.084375000614517859, 4.541064518000418104, 2.621784821874999949 ) ) ;
#62754 = VECTOR ( 'NONE', #29034, 1000.000000000000000 ) ;
#62755 = CARTESIAN_POINT ( 'NONE',  ( 3.590625000614518836, 6.054752690667223547, 3.707466751127219781E-16 ) ) ;
#62756 = CARTESIAN_POINT ( 'NONE',  ( 28.12499999999999645, 4.330127018922191873, 2.499999999999999556 ) ) ;
#62757 = CARTESIAN_POINT ( 'NONE',  ( 9.712500000000002132, 2.886751345948126879, 4.999999999999998224 ) ) ;
#62758 = CARTESIAN_POINT ( 'NONE',  ( 8.259375000614518569, 0.000000000000000000, 5.243569643749999010 ) ) ;
#62759 = CARTESIAN_POINT ( 'NONE',  ( 12.68437500061451573, 4.541064518000418104, 2.621784821874999949 ) ) ;
#62760 = CARTESIAN_POINT ( 'NONE',  ( 7.320879633048903241E-15, 18.53750000000000142, -34.00000000000000000 ) ) ;
#62761 = CARTESIAN_POINT ( 'NONE',  ( 6.600000000000001421, 0.000000000000000000, 4.999999999999998224 ) ) ;
#62762 = CARTESIAN_POINT ( 'NONE',  ( -4.243569643749998122, 17.14062500061459460, 32.45002607614398471 ) ) ;
#62763 = CARTESIAN_POINT ( 'NONE',  ( 21.34687500061451715, -3.027376345333614438, 5.243569643749998122 ) ) ;
#62764 = CARTESIAN_POINT ( 'NONE',  ( 26.40000000122902790, 5.773502691896255534, 3.535250795749688894E-16 ) ) ;
#62765 = B_SPLINE_CURVE_WITH_KNOTS ( 'NONE', 3,
 ( #70018, #30499, #54134, #64470, #43044, #14960, #48224, #71116, #58918, #36405 ),
 .UNSPECIFIED., .F., .F.,
 ( 4, 3, 3, 4 ),
 ( 2.168404344971008868E-19, 0.0001572616466639377138, 0.0002553267708066046891, 0.0003534655997994981189 ),
 .UNSPECIFIED. ) ;
#62766 = CARTESIAN_POINT ( 'NONE',  ( 16.95937500061451431, 2.746126346562645981, -4.756430356249997438 ) ) ;
#62767 = CARTESIAN_POINT ( 'NONE',  ( 23.65312500061451573, -4.541064518000417216, -2.621784821875001281 ) ) ;
#62768 = CARTESIAN_POINT ( 'NONE',  ( 16.37812500061451715, -4.541064518000419881, 2.621784821874995952 ) ) ;
#62769 = CARTESIAN_POINT ( 'NONE',  ( 26.89687500061451431, 4.119189519843966529, -2.378215178124998275 ) ) ;
#62770 = CARTESIAN_POINT ( 'NONE',  ( 12.68437500061451573, 4.541064518000418104, 2.621784821874999949 ) ) ;
#62771 = CARTESIAN_POINT ( 'NONE',  ( 28.01249999999999574, 2.886751345948129099, -4.999999999999998224 ) ) ;
#62772 = CARTESIAN_POINT ( 'NONE',  ( 25.72500000122903074, -5.773502691896255534, -1.060575238724906372E-15 ) ) ;
#62773 = DIRECTION ( 'NONE',  ( -0.000000000000000000, -1.000000000000000000, -0.000000000000000000 ) ) ;
#62774 = CARTESIAN_POINT ( 'NONE',  ( 12.64687500061451608, 6.054752690667223547, 3.707466751127219781E-16 ) ) ;
#62775 = CARTESIAN_POINT ( 'NONE',  ( 27.90937500061451715, 4.541064518000418104, -2.621784821874998173 ) ) ;
#62776 = DIRECTION ( 'NONE',  ( -0.000000000000000000, -1.000000000000000000, -0.000000000000000000 ) ) ;
#62777 = CARTESIAN_POINT ( 'NONE',  ( -3.999999999999999112, 11.97500000122903430, 27.69059892324149885 ) ) ;
#62778 = CARTESIAN_POINT ( 'NONE',  ( 22.09687500061451715, 6.054752690667223547, 3.707466751127219781E-16 ) ) ;
#62779 = CARTESIAN_POINT ( 'NONE',  ( 13.47187500061451537, 3.027376345333613106, -5.243569643749998122 ) ) ;
#62780 = CARTESIAN_POINT ( 'NONE',  ( -3.756430356250001434, 17.96562499938548285, 32.16877607737301048 ) ) ;
#62781 = CARTESIAN_POINT ( 'NONE',  ( 26.39999999999999858, 0.000000000000000000, 4.999999999999998224 ) ) ;
#62782 = CARTESIAN_POINT ( 'NONE',  ( -8.484601909799255319E-16, 13.28749999999999964, 34.61880215351700940 ) ) ;
#62783 = CARTESIAN_POINT ( 'NONE',  ( 26.03437500061451715, 5.824947211148865298E-16, -4.756430356249998326 ) ) ;
#62784 = CARTESIAN_POINT ( 'NONE',  ( 17.80312500061451786, -4.541064518000417216, -2.621784821875001281 ) ) ;
#62785 = CARTESIAN_POINT ( 'NONE',  ( 8.099999999999999645, -4.330127018922190985, -2.500000000000001332 ) ) ;
#62786 = CARTESIAN_POINT ( 'NONE',  ( 2.000000000000001332, 13.51250000122903394, 33.46410161513774995 ) ) ;
#62787 = CARTESIAN_POINT ( 'NONE',  ( 17.32499999999999929, 4.330127018922191873, 2.499999999999999556 ) ) ;
#62788 = CARTESIAN_POINT ( 'NONE',  ( 4.243569643749999010, 11.06562500061451715, 27.54997392385601174 ) ) ;
#62789 = CARTESIAN_POINT ( 'NONE',  ( -3.999999999999999112, 16.28750000000000142, 27.69059892324149530 ) ) ;
#62790 = CARTESIAN_POINT ( 'NONE',  ( 28.17187500061451644, -6.054752690667223547, -1.112240025338166033E-15 ) ) ;
#62791 = EDGE_LOOP ( 'NONE', ( #51237, #19653, #28754, #39123 ) ) ;
#62792 = CARTESIAN_POINT ( 'NONE',  ( 21.55312500061451431, 4.541064518000418104, -2.621784821874998173 ) ) ;
#62793 = CARTESIAN_POINT ( 'NONE',  ( 19.80937500061451573, 4.541064518000418104, -2.621784821874998173 ) ) ;
#62794 = CARTESIAN_POINT ( 'NONE',  ( 4.575000000000002842, 6.123233995736764310E-16, -4.999999999999998224 ) ) ;
#62795 = CARTESIAN_POINT ( 'NONE',  ( 7.865625000614516971, -6.054752690667223547, -1.112240025338166033E-15 ) ) ;
#62796 = CARTESIAN_POINT ( 'NONE',  ( 23.12812500061451360, -4.541064518000419881, 2.621784821874995952 ) ) ;
#62797 = CARTESIAN_POINT ( 'NONE',  ( 12.68437500061451573, 4.541064518000418104, 2.621784821874999949 ) ) ;
#62798 = CARTESIAN_POINT ( 'NONE',  ( 17.25937500061451502, 0.000000000000000000, 5.243569643749999010 ) ) ;
#62799 = CARTESIAN_POINT ( 'NONE',  ( -2.121784821874999949, 18.37812500061451715, 26.32496088578401938 ) ) ;
#62800 = CARTESIAN_POINT ( 'NONE',  ( 17.96250000122903501, 0.000000000000000000, 4.999999999999998224 ) ) ;
#62801 = CARTESIAN_POINT ( 'NONE',  ( 15.72187500061451892, 2.746126346562645981, -4.756430356249997438 ) ) ;
#62802 = CARTESIAN_POINT ( 'NONE',  ( 9.178125000614517859, -4.541064518000419881, 2.621784821874995952 ) ) ;
#62803 = CARTESIAN_POINT ( 'NONE',  ( 5.484375000614518214, 4.541064518000418104, 2.621784821874999949 ) ) ;
#62804 = CARTESIAN_POINT ( 'NONE',  ( 4.584375000614516971, 4.541064518000418104, 2.621784821874999949 ) ) ;
#62805 = ORIENTED_EDGE ( 'NONE', *, *, #38215, .F. ) ;
#62806 = CARTESIAN_POINT ( 'NONE',  ( 26.22187500061451715, 3.027376345333611329, 5.243569643749999010 ) ) ;
#62807 = CARTESIAN_POINT ( 'NONE',  ( 17.91562500061451502, 3.027376345333613106, -5.243569643749998122 ) ) ;
#62808 = CARTESIAN_POINT ( 'NONE',  ( 28.20000000122903216, 5.773502691896255534, 3.535250795749688894E-16 ) ) ;
#62809 = CARTESIAN_POINT ( 'NONE',  ( 27.36562500061451786, 3.027376345333613106, -5.243569643749998122 ) ) ;
#62810 = VECTOR ( 'NONE', #11437, 1000.000000000000000 ) ;
#62811 = CARTESIAN_POINT ( 'NONE',  ( 21.49687500061451573, -3.027376345333610441, -5.243569643749999898 ) ) ;
#62812 = CARTESIAN_POINT ( 'NONE',  ( 17.35312500061451502, -4.541064518000417216, -2.621784821875001281 ) ) ;
#62813 = CARTESIAN_POINT ( 'NONE',  ( 9.001249775931846008E-16, 16.82187500061451857, 34.90005215228797653 ) ) ;
#62814 = CARTESIAN_POINT ( 'NONE',  ( 21.77812500061451928, -4.541064518000419881, 2.621784821874995952 ) ) ;
#62815 = CARTESIAN_POINT ( 'NONE',  ( 21.89999999999999858, 0.000000000000000000, 4.999999999999998224 ) ) ;
#62816 = EDGE_LOOP ( 'NONE', ( #6952, #61638, #19423, #35701 ) ) ;
#62817 = CARTESIAN_POINT ( 'NONE',  ( 28.64999999999999858, 0.000000000000000000, 4.999999999999998224 ) ) ;
#62818 = CARTESIAN_POINT ( 'NONE',  ( -3.999999999999999112, 14.15000000000000036, -30.00000000000000000 ) ) ;
#62819 = CARTESIAN_POINT ( 'NONE',  ( 3.756430356249998770, 19.91562499938548214, 32.16877607737302469 ) ) ;
#62820 = CARTESIAN_POINT ( 'NONE',  ( 29.50312500061451360, -4.541064518000417216, -2.621784821875001281 ) ) ;
#62821 = CARTESIAN_POINT ( 'NONE',  ( 9.328125000614518214, 6.421520780324663323E-16, -5.243569643749999010 ) ) ;
#62822 = CARTESIAN_POINT ( 'NONE',  ( 22.05000000122903714, -2.886751345948129988, 4.999999999999997335 ) ) ;
#62823 = CARTESIAN_POINT ( 'NONE',  ( 28.34062500061451928, 6.054752690667223547, 3.707466751127219781E-16 ) ) ;
#62824 = CARTESIAN_POINT ( 'NONE',  ( 28.35000000000000142, -4.330127018922190985, -2.500000000000001332 ) ) ;
#62825 = CARTESIAN_POINT ( 'NONE',  ( -1.999999999999997113, 17.48750000122903359, -26.53589838486224295 ) ) ;
#62826 = CARTESIAN_POINT ( 'NONE',  ( 1.592000809091587073E-14, 16.28750000000000142, 26.00000000000000000 ) ) ;
#62827 = CARTESIAN_POINT ( 'NONE',  ( 11.65312500061451573, 4.541064518000418104, -2.621784821874998173 ) ) ;
#62828 = ORIENTED_EDGE ( 'NONE', *, *, #2690, .T. ) ;
#62829 = CARTESIAN_POINT ( 'NONE',  ( 8.053125000614516082, 4.541064518000418104, -2.621784821874998173 ) ) ;
#62830 = CARTESIAN_POINT ( 'NONE',  ( 5.690625000614516260, -3.027376345333610441, -5.243569643749999898 ) ) ;
#62831 = CARTESIAN_POINT ( 'NONE',  ( 16.99687500061451573, -2.746126346562642428, -4.756430356249999214 ) ) ;
#62832 = PLANE ( 'NONE',  #58560 ) ;
#62833 = EDGE_CURVE ( 'NONE', #29422, #26491, #14366, .T. ) ;
#62834 = CARTESIAN_POINT ( 'NONE',  ( 14.55000000000000071, 4.330127018922192761, -2.499999999999997780 ) ) ;
#62835 = EDGE_CURVE ( 'NONE', #13067, #47310, #15094, .T. ) ;
#62836 = CARTESIAN_POINT ( 'NONE',  ( 16.88437500061451502, -4.541064518000419881, 2.621784821874995952 ) ) ;
#62837 = CARTESIAN_POINT ( 'NONE',  ( 12.41250000122903430, 4.330127018922192761, -2.499999999999997780 ) ) ;
#62838 = CARTESIAN_POINT ( 'NONE',  ( 18.94687500061451502, 6.054752690667223547, 3.707466751127219781E-16 ) ) ;
#62839 = CARTESIAN_POINT ( 'NONE',  ( 16.27499999999999858, 6.123233995736764310E-16, -4.999999999999998224 ) ) ;
#62840 = CARTESIAN_POINT ( 'NONE',  ( 21.64687500061451786, 6.054752690667223547, 3.707466751127219781E-16 ) ) ;
#62841 = CARTESIAN_POINT ( 'NONE',  ( -3.000416591977282496E-16, 14.74062500061451786, -34.90005215228797653 ) ) ;
#62842 = CARTESIAN_POINT ( 'NONE',  ( 26.10937500061451644, 2.746126346562643317, 4.756430356249998326 ) ) ;
#62843 = CARTESIAN_POINT ( 'NONE',  ( 4.140919957849956923, 2.802311140224996944, 4.431956019633390476 ) ) ;
#62844 = CARTESIAN_POINT ( 'NONE',  ( 26.05312500061451431, 4.541064518000418104, -2.621784821874998173 ) ) ;
#62845 = DIRECTION ( 'NONE',  ( 0.000000000000000000, -1.000000000000000000, 0.000000000000000000 ) ) ;
#62846 = CARTESIAN_POINT ( 'NONE',  ( 28.92187500061451644, 3.027376345333611329, 5.243569643749999010 ) ) ;
#62847 = CARTESIAN_POINT ( 'NONE',  ( 23.36250000000000071, -5.773502691896255534, -1.060575238724906372E-15 ) ) ;
#62848 = CARTESIAN_POINT ( 'NONE',  ( 5.840625000614516615, 6.054752690667223547, 3.707466751127219781E-16 ) ) ;
#62849 = CARTESIAN_POINT ( 'NONE',  ( 23.78437500061451360, 5.492252693125287522, 3.363034840372157021E-16 ) ) ;
#62850 = CARTESIAN_POINT ( 'NONE',  ( 19.95937500061451786, 0.000000000000000000, 5.243569643749999010 ) ) ;
#62851 = CARTESIAN_POINT ( 'NONE',  ( 10.09687500061451715, -4.119189519843965641, -2.378215178125001383 ) ) ;
#62852 = CARTESIAN_POINT ( 'NONE',  ( 4.940625000614515372, 6.054752690667223547, 3.707466751127219781E-16 ) ) ;
#62853 = CARTESIAN_POINT ( 'NONE',  ( 8.371875000614515727, -6.054752690667223547, -1.112240025338166033E-15 ) ) ;
#62854 = EDGE_LOOP ( 'NONE', ( #18107, #23708, #60618, #63238 ) ) ;
#62855 = CARTESIAN_POINT ( 'NONE',  ( 18.19687500061451502, -3.027376345333614438, 5.243569643749998122 ) ) ;
#62856 = CARTESIAN_POINT ( 'NONE',  ( -5.810221930991193690E-16, 11.90000000122903323, 26.00000000000000355 ) ) ;
#62857 = CARTESIAN_POINT ( 'NONE',  ( 28.04999999999999716, 4.330127018922192761, -2.499999999999997780 ) ) ;
#62858 = CARTESIAN_POINT ( 'NONE',  ( 3.337499999999999911, 5.773502691896255534, 3.535250795749688894E-16 ) ) ;
#62859 = CARTESIAN_POINT ( 'NONE',  ( -1.626862140677534273E-15, 15.53750000000000142, 34.00000000000000000 ) ) ;
#62860 = ORIENTED_EDGE ( 'NONE', *, *, #4790, .F. ) ;
#62861 = CARTESIAN_POINT ( 'NONE',  ( 11.06250000000000000, 2.886751345948126879, 4.999999999999999112 ) ) ;
#62862 = CARTESIAN_POINT ( 'NONE',  ( 10.99687500061451573, -4.119189519843965641, -2.378215178125001383 ) ) ;
#62863 = CARTESIAN_POINT ( 'NONE',  ( 24.44062500061451715, -3.027376345333614438, 5.243569643749998122 ) ) ;
#62864 = CARTESIAN_POINT ( 'NONE',  ( 13.53749999999999964, -2.886751345948125991, -5.000000000000000000 ) ) ;
#62865 = CARTESIAN_POINT ( 'NONE',  ( 9.975000001229034297, -5.773502691896255534, -1.060575238724906372E-15 ) ) ;
#62866 = CARTESIAN_POINT ( 'NONE',  ( 10.07812500061451644, -4.541064518000419881, 2.621784821874995952 ) ) ;
#62867 = CARTESIAN_POINT ( 'NONE',  ( 24.44999999999999929, 4.330127018922192761, -2.499999999999997780 ) ) ;
#62868 = CARTESIAN_POINT ( 'NONE',  ( 21.29062500061451502, -3.027376345333614438, 5.243569643749998122 ) ) ;
#62869 = CARTESIAN_POINT ( 'NONE',  ( 14.92500000000000071, 6.123233995736764310E-16, -4.999999999999998224 ) ) ;
#62870 = CARTESIAN_POINT ( 'NONE',  ( 27.90000000122903145, -2.886751345948129988, 4.999999999999997335 ) ) ;
#62871 = CARTESIAN_POINT ( 'NONE',  ( -1.878215178124999163, 16.84062499938548285, 26.74683588394047007 ) ) ;
#62872 = CARTESIAN_POINT ( 'NONE',  ( 6.562500000000001776, 2.886751345948126879, 4.999999999999999112 ) ) ;
#62873 = EDGE_LOOP ( 'NONE', ( #24873, #45813, #44496, #32485 ) ) ;
#62874 = CARTESIAN_POINT ( 'NONE',  ( 22.49062500061451431, 6.054752690667223547, 3.707466751127219781E-16 ) ) ;
#62875 = CARTESIAN_POINT ( 'NONE',  ( 28.64062500061451289, -3.027376345333610441, -5.243569643749999898 ) ) ;
#62876 = LINE ( 'NONE', #72523, #69119 ) ;
#62877 = CARTESIAN_POINT ( 'NONE',  ( 19.35937500061451644, 4.541064518000418104, -2.621784821874998173 ) ) ;
#62878 = CARTESIAN_POINT ( 'NONE',  ( 13.34062500061451750, -3.027376345333610441, -5.243569643749999898 ) ) ;
#62879 = FACE_BOUND ( 'NONE', #70176, .T. ) ;
#62880 = CARTESIAN_POINT ( 'NONE',  ( 26.47500000122903074, 2.886751345948126879, 4.999999999999999112 ) ) ;
#62881 = CARTESIAN_POINT ( 'NONE',  ( 22.80937500061451573, -4.119189519843965641, -2.378215178125001383 ) ) ;
#62882 = CARTESIAN_POINT ( 'NONE',  ( 16.60312500061451857, 4.541064518000418104, -2.621784821874998173 ) ) ;
#62883 = CARTESIAN_POINT ( 'NONE',  ( 30.00000000000000000, 0.000000000000000000, 0.000000000000000000 ) ) ;
#62884 = CARTESIAN_POINT ( 'NONE',  ( 4.500000001229034652, -2.886751345948129988, 4.999999999999997335 ) ) ;
#62885 = CARTESIAN_POINT ( 'NONE',  ( 12.45937500061451786, -4.541064518000417216, -2.621784821875001281 ) ) ;
#62886 = CARTESIAN_POINT ( 'NONE',  ( 12.64687500061451608, 6.054752690667223547, 3.707466751127219781E-16 ) ) ;
#62887 = CARTESIAN_POINT ( 'NONE',  ( 20.74687500061451573, 6.054752690667223547, 3.707466751127219781E-16 ) ) ;
#62888 = ORIENTED_EDGE ( 'NONE', *, *, #9933, .F. ) ;
#62889 = CARTESIAN_POINT ( 'NONE',  ( -5.959432963256015015, 8.030867404579451474, 30.80300165410438851 ) ) ;
#62890 = CARTESIAN_POINT ( 'NONE',  ( 23.99062500061451786, -3.027376345333614438, 5.243569643749998122 ) ) ;
#62891 =( BOUNDED_CURVE ( )  B_SPLINE_CURVE ( 2, ( #28203, #46269, #6021, #62174, #68808, #18164, #22283 ),
 .UNSPECIFIED., .F., .F. ) 
 B_SPLINE_CURVE_WITH_KNOTS ( ( 3, 2, 2, 3 ),
 ( 0.6083333333333332815, 0.6111111111111111605, 0.6138888888888889284, 0.6166666666666666963 ),
 .UNSPECIFIED. ) 
 CURVE ( )  GEOMETRIC_REPRESENTATION_ITEM ( )  RATIONAL_B_SPLINE_CURVE ( ( 1.000000000000000000, 0.8660254037844387076, 1.000000000000000000, 0.8660254037844387076, 1.000000000000000000, 0.8660254037844387076, 1.000000000000000000 ) ) 
 REPRESENTATION_ITEM ( '' )  );
#62892 = CARTESIAN_POINT ( 'NONE',  ( 19.54687500061451644, -3.027376345333614438, 5.243569643749998122 ) ) ;
#62893 = CARTESIAN_POINT ( 'NONE',  ( 24.02812500061451573, -4.541064518000419881, 2.621784821874995952 ) ) ;
#62894 = CARTESIAN_POINT ( 'NONE',  ( 18.35625000122903216, 0.000000000000000000, 4.999999999999998224 ) ) ;
#62895 = CARTESIAN_POINT ( 'NONE',  ( 2.000000000000001332, 15.65000000000000036, 33.46410161513774995 ) ) ;
#62896 = CARTESIAN_POINT ( 'NONE',  ( 28.86562500061451786, 3.027376345333611329, 5.243569643749999010 ) ) ;
#62897 = CARTESIAN_POINT ( 'NONE',  ( 10.65000000122903323, 5.773502691896255534, 3.535250795749688894E-16 ) ) ;
#62898 = CARTESIAN_POINT ( 'NONE',  ( 5.850000001229035185, -2.886751345948129988, 4.999999999999997335 ) ) ;
#62899 = CARTESIAN_POINT ( 'NONE',  ( 30.00000000000000000, 0.000000000000000000, 4.999999999999998224 ) ) ;
#62900 = CARTESIAN_POINT ( 'NONE',  ( 27.86250000122903359, 0.000000000000000000, 4.999999999999998224 ) ) ;
#62901 = CARTESIAN_POINT ( 'NONE',  ( 1.999999999999997335, 19.56874999877096499, 33.46410161513775705 ) ) ;
#62902 = CARTESIAN_POINT ( 'NONE',  ( 16.48125000122903216, 4.330127018922191873, 2.499999999999999556 ) ) ;
#62903 = CARTESIAN_POINT ( 'NONE',  ( 9.421875000614519990, 3.027376345333613106, -5.243569643749998122 ) ) ;
#62904 = CARTESIAN_POINT ( 'NONE',  ( 10.10625000122903216, 4.330127018922192761, -2.499999999999997780 ) ) ;
#62905 = CARTESIAN_POINT ( 'NONE',  ( 17.46562500061451217, 3.027376345333613106, -5.243569643749998122 ) ) ;
#62906 = CARTESIAN_POINT ( 'NONE',  ( 10.54687500061451644, -3.027376345333614438, 5.243569643749998122 ) ) ;
#62907 = CARTESIAN_POINT ( 'NONE',  ( 28.50000000122903288, -2.886751345948125991, -5.000000000000000000 ) ) ;
#62908 = CARTESIAN_POINT ( 'NONE',  ( 19.99687500061451573, -3.027376345333614438, 5.243569643749998122 ) ) ;
#62909 = CARTESIAN_POINT ( 'NONE',  ( 7.809375000614519280, 0.000000000000000000, 5.243569643749999010 ) ) ;
#62910 = CARTESIAN_POINT ( 'NONE',  ( 2.803125000614518747, 0.000000000000000000, 5.243569643749999010 ) ) ;
#62911 = CARTESIAN_POINT ( 'NONE',  ( 6.150000000000003020, 0.000000000000000000, 4.999999999999998224 ) ) ;
#62912 = CARTESIAN_POINT ( 'NONE',  ( 8.990625000614516082, 6.054752690667223547, 3.707466751127219781E-16 ) ) ;
#62913 = CARTESIAN_POINT ( 'NONE',  ( 19.15312500061451573, -4.541064518000417216, -2.621784821875001281 ) ) ;
#62914 = EDGE_LOOP ( 'NONE', ( #24976, #71794, #72471 ) ) ;
#62915 = CARTESIAN_POINT ( 'NONE',  ( 5.100000001229034297, -2.886751345948125991, -5.000000000000000000 ) ) ;
#62916 = CARTESIAN_POINT ( 'NONE',  ( 14.24062500061451608, -3.027376345333610441, -5.243569643749999898 ) ) ;
#62917 = CARTESIAN_POINT ( 'NONE',  ( 12.81562500061451537, -6.054752690667223547, -1.112240025338166033E-15 ) ) ;
#62918 = CARTESIAN_POINT ( 'NONE',  ( 24.15937500061451715, -4.119189519843965641, -2.378215178125001383 ) ) ;
#62919 = CARTESIAN_POINT ( 'NONE',  ( 13.95000000000000107, -4.330127018922190985, -2.500000000000001332 ) ) ;
#62920 = CARTESIAN_POINT ( 'NONE',  ( 7.912500001229033408, 4.330127018922192761, -2.499999999999997780 ) ) ;
#62921 = CARTESIAN_POINT ( 'NONE',  ( 6.290625000614517681, 6.054752690667223547, 3.707466751127219781E-16 ) ) ;
#62922 = EDGE_CURVE ( 'NONE', #16658, #60892, #29597, .T. ) ;
#62923 = CARTESIAN_POINT ( 'NONE',  ( 19.12500000122903288, 2.886751345948129099, -4.999999999999998224 ) ) ;
#62924 = CARTESIAN_POINT ( 'NONE',  ( 23.47499999999999787, 6.123233995736764310E-16, -4.999999999999998224 ) ) ;
#62925 = CARTESIAN_POINT ( 'NONE',  ( 4.243569643749999898, 11.94687500061451857, -27.54997392385601529 ) ) ;
#62926 = CARTESIAN_POINT ( 'NONE',  ( 8.512499999999999289, -5.773502691896255534, -1.060575238724906372E-15 ) ) ;
#62927 = CARTESIAN_POINT ( 'NONE',  ( 3.337500001229034563, 6.123233995736764310E-16, -4.999999999999998224 ) ) ;
#62928 = CARTESIAN_POINT ( 'NONE',  ( -3.999999999999999112, 11.41250000000000142, -32.30940107675850470 ) ) ;
#62929 = CYLINDRICAL_SURFACE ( 'NONE', #706, 4.999999999999998224 ) ;
#62930 = CARTESIAN_POINT ( 'NONE',  ( 18.38437500061451857, 6.421520780324663323E-16, -5.243569643749999010 ) ) ;
#62931 = CARTESIAN_POINT ( 'NONE',  ( 21.33750000122903145, 6.123233995736764310E-16, -4.999999999999998224 ) ) ;
#62932 = CARTESIAN_POINT ( 'NONE',  ( 14.24062500061451608, -3.027376345333610441, -5.243569643749999898 ) ) ;
#62933 = CARTESIAN_POINT ( 'NONE',  ( 9.243750001229033231, 5.773502691896255534, 3.535250795749688894E-16 ) ) ;
#62934 = CARTESIAN_POINT ( 'NONE',  ( 1.071796769724479237, 16.64240381056766438, 25.99999999999999645 ) ) ;
#62935 = CARTESIAN_POINT ( 'NONE',  ( 26.63437500061451857, 4.541064518000418104, 2.621784821874999949 ) ) ;
#62936 = CARTESIAN_POINT ( 'NONE',  ( 17.63437500061451502, -2.746126346562646425, 4.756430356249996549 ) ) ;
#62937 = CARTESIAN_POINT ( 'NONE',  ( 13.26562500061451644, -6.054752690667223547, -1.112240025338166033E-15 ) ) ;
#62938 = CARTESIAN_POINT ( 'NONE',  ( 10.24687500061451750, -3.027376345333610441, -5.243569643749999898 ) ) ;
#62939 = ORIENTED_EDGE ( 'NONE', *, *, #37818, .F. ) ;
#62940 = CARTESIAN_POINT ( 'NONE',  ( 2.869618986945705608, -4.094575117703225686, -3.017297621565764310 ) ) ;
#62941 = CARTESIAN_POINT ( 'NONE',  ( 20.20312500061451644, 4.541064518000418104, -2.621784821874998173 ) ) ;
#62942 = LINE ( 'NONE', #35956, #30950 ) ;
#62943 = CARTESIAN_POINT ( 'NONE',  ( 10.81875000122903252, -5.773502691896255534, -1.060575238724906372E-15 ) ) ;
#62944 = CARTESIAN_POINT ( 'NONE',  ( 9.187500000000001776, 5.773502691896255534, 3.535250795749688894E-16 ) ) ;
#62945 = CARTESIAN_POINT ( 'NONE',  ( 20.13750000122903216, 4.330127018922191873, 2.499999999999999556 ) ) ;
#62946 = CARTESIAN_POINT ( 'NONE',  ( 3.999999999999998668, 10.36250000000000426, 27.69059892324149530 ) ) ;
#62947 = CARTESIAN_POINT ( 'NONE',  ( 9.571875000614515017, -4.119189519843968306, 2.378215178124996054 ) ) ;
#62948 = VERTEX_POINT ( 'NONE', #52800 ) ;
#62949 = CARTESIAN_POINT ( 'NONE',  ( 17.36249999999999716, 2.886751345948126879, 4.999999999999999112 ) ) ;
#62950 = CARTESIAN_POINT ( 'NONE',  ( 20.51249999999999929, 2.886751345948126879, 4.999999999999999112 ) ) ;
#62951 = CARTESIAN_POINT ( 'NONE',  ( 19.05937500061451928, 0.000000000000000000, 5.243569643749999010 ) ) ;
#62952 = CARTESIAN_POINT ( 'NONE',  ( 24.36562500061451786, 3.027376345333611329, 5.243569643749999010 ) ) ;
#62953 = ORIENTED_EDGE ( 'NONE', *, *, #53010, .T. ) ;
#62954 = CARTESIAN_POINT ( 'NONE',  ( -3.999999999999999112, 16.92500000122903359, 27.69059892324149885 ) ) ;
#62955 = CARTESIAN_POINT ( 'NONE',  ( 8.990625000614516082, 6.054752690667223547, 3.707466751127219781E-16 ) ) ;
#62956 = LINE ( 'NONE', #1284, #61872 ) ;
#62957 = CARTESIAN_POINT ( 'NONE',  ( 15.07499999999999929, 4.330127018922191873, 2.499999999999999556 ) ) ;
#62958 = CARTESIAN_POINT ( 'NONE',  ( 2.121784821874999061, 18.75312500061451715, 26.32496088578401583 ) ) ;
#62959 = CARTESIAN_POINT ( 'NONE',  ( 3.196875000614516793, 6.054752690667223547, 3.707466751127219781E-16 ) ) ;
#62960 = CARTESIAN_POINT ( 'NONE',  ( 10.20000000000000107, 0.000000000000000000, 4.999999999999998224 ) ) ;
#62961 = CARTESIAN_POINT ( 'NONE',  ( 1.878215178125000495, 14.96562499938548463, 26.74683588394047007 ) ) ;
#62962 = CARTESIAN_POINT ( 'NONE',  ( 25.50937500061451502, -4.541064518000417216, -2.621784821875001281 ) ) ;
#62963 = ORIENTED_EDGE ( 'NONE', *, *, #12710, .T. ) ;
#62964 = CARTESIAN_POINT ( 'NONE',  ( 24.06562500061451715, -6.054752690667223547, -1.112240025338166033E-15 ) ) ;
#62965 = CARTESIAN_POINT ( 'NONE',  ( 23.63437500061451502, -4.541064518000419881, 2.621784821874995952 ) ) ;
#62966 = CARTESIAN_POINT ( 'NONE',  ( -4.243569643749999898, 17.06562500061459176, -32.45002607614398471 ) ) ;
#62967 = CARTESIAN_POINT ( 'NONE',  ( 10.68750000000000000, -2.886751345948129988, 4.999999999999997335 ) ) ;
#62968 = CARTESIAN_POINT ( 'NONE',  ( 8.015625000614518214, 3.027376345333613106, -5.243569643749998122 ) ) ;
#62969 = CARTESIAN_POINT ( 'NONE',  ( 3.787500000000002753, 5.773502691896255534, 3.535250795749688401E-16 ) ) ;
#62970 = CARTESIAN_POINT ( 'NONE',  ( 28.94062500061452070, -3.027376345333614438, 5.243569643749998122 ) ) ;
#62971 = CARTESIAN_POINT ( 'NONE',  ( 27.29062500061451502, -3.027376345333610441, -5.243569643749999898 ) ) ;
#62972 = CARTESIAN_POINT ( 'NONE',  ( 28.28437500061451715, 5.492252693125287522, 3.363034840372157021E-16 ) ) ;
#62973 = CARTESIAN_POINT ( 'NONE',  ( 12.42187500061451821, -5.492252693125287522, -1.008910452111647106E-15 ) ) ;
#62974 = CARTESIAN_POINT ( 'NONE',  ( 19.28437500061451360, 6.421520780324663323E-16, -5.243569643749999010 ) ) ;
#62975 = CARTESIAN_POINT ( 'NONE',  ( -4.243569643749997233, 11.79687500061451999, 32.45002607614398471 ) ) ;
#62976 = CARTESIAN_POINT ( 'NONE',  ( 18.34687500061451715, -3.027376345333610441, -5.243569643749999898 ) ) ;
#62977 = CARTESIAN_POINT ( 'NONE',  ( 28.39687500061452141, 6.054752690667223547, 3.707466751127219781E-16 ) ) ;
#62978 = CARTESIAN_POINT ( 'NONE',  ( 4.243569643749999898, 16.48437500061451644, 30.00000000000000000 ) ) ;
#62979 = CARTESIAN_POINT ( 'NONE',  ( 8.203125000614518214, 0.000000000000000000, 5.243569643749999010 ) ) ;
#62980 = CARTESIAN_POINT ( 'NONE',  ( -1.071796769724492338, 18.29240381056766651, -26.00000000000000711 ) ) ;
#62981 = CARTESIAN_POINT ( 'NONE',  ( 3.534375000614518036, 6.421520780324663323E-16, -5.243569643749999010 ) ) ;
#62982 = CARTESIAN_POINT ( 'NONE',  ( 0.000000000000000000, 20.00000000000000000, 26.00000000000000000 ) ) ;
#62983 = CARTESIAN_POINT ( 'NONE',  ( 5.615625000614517859, -6.054752690667223547, -1.112240025338166033E-15 ) ) ;
#62984 = CARTESIAN_POINT ( 'NONE',  ( 9.946875000614516793, 6.054752690667223547, 3.707466751127219781E-16 ) ) ;
#62985 = SURFACE_STYLE_FILL_AREA ( #40470 ) ;
#62986 = CARTESIAN_POINT ( 'NONE',  ( 17.70000000122903216, -2.886751345948125991, -5.000000000000000000 ) ) ;
#62987 = CARTESIAN_POINT ( 'NONE',  ( 5.446875000614518569, 6.054752690667223547, 3.707466751127219781E-16 ) ) ;
#62988 = CARTESIAN_POINT ( 'NONE',  ( 6.890625000614516438, -3.027376345333614438, 5.243569643749998122 ) ) ;
#62989 = CARTESIAN_POINT ( 'NONE',  ( 2.000000000000000444, 12.57500000000000107, 26.53589838486224650 ) ) ;
#62990 = CARTESIAN_POINT ( 'NONE',  ( 23.23125000122903216, 4.330127018922191873, 2.499999999999999556 ) ) ;
#62991 = CARTESIAN_POINT ( 'NONE',  ( 16.58437500061451786, 6.421520780324663323E-16, -5.243569643749999010 ) ) ;
#62992 = CARTESIAN_POINT ( 'NONE',  ( 1.071796769724479237, 19.28615380933863221, 25.99999999999999645 ) ) ;
#62993 = ORIENTED_EDGE ( 'NONE', *, *, #33221, .T. ) ;
#62994 = CARTESIAN_POINT ( 'NONE',  ( 23.61562500061451431, -6.054752690667223547, -1.112240025338166033E-15 ) ) ;
#62995 = CARTESIAN_POINT ( 'NONE',  ( 9.103125000614515017, 0.000000000000000000, 5.243569643749999010 ) ) ;
#62996 = CARTESIAN_POINT ( 'NONE',  ( 27.34687500061451360, -3.027376345333610441, -5.243569643749999898 ) ) ;
#62997 =( REPRESENTATION_RELATIONSHIP ('NONE','NONE', #33485, #25944 ) REPRESENTATION_RELATIONSHIP_WITH_TRANSFORMATION ( #11218 )SHAPE_REPRESENTATION_RELATIONSHIP( ) );
#62998 = CARTESIAN_POINT ( 'NONE',  ( 10.79062500061451679, 6.054752690667223547, 3.707466751127219781E-16 ) ) ;
#62999 = CARTESIAN_POINT ( 'NONE',  ( -2.121784821874996840, 10.03437500061451892, -26.32496088578401583 ) ) ;
#63000 = CARTESIAN_POINT ( 'NONE',  ( 9.712500001229033231, 4.330127018922192761, -2.499999999999997780 ) ) ;
#63001 = CARTESIAN_POINT ( 'NONE',  ( 26.99062500061451431, 6.054752690667223547, 3.707466751127219781E-16 ) ) ;
#63002 = CARTESIAN_POINT ( 'NONE',  ( 2.121784821875001281, 11.85312500061451857, -26.32496088578401938 ) ) ;
#63003 = CARTESIAN_POINT ( 'NONE',  ( 12.60000000122903430, -2.886751345948129988, 4.999999999999997335 ) ) ;
#63004 = CARTESIAN_POINT ( 'NONE',  ( 10.46249999999999858, 2.886751345948129099, -4.999999999999998224 ) ) ;
#63005 = CARTESIAN_POINT ( 'NONE',  ( 20.31562500061451715, 3.027376345333611329, 5.243569643749999010 ) ) ;
#63006 = CARTESIAN_POINT ( 'NONE',  ( 30.00000000000000000, 0.000000000000000000, 4.999999999999998224 ) ) ;
#63007 = EDGE_CURVE ( 'NONE', #72067, #9906, #26516, .T. ) ;
#63008 = CARTESIAN_POINT ( 'NONE',  ( 20.77500000000000213, 6.123233995736764310E-16, -4.999999999999998224 ) ) ;
#63009 = CARTESIAN_POINT ( 'NONE',  ( 7.162500001229032520, 0.000000000000000000, 4.999999999999998224 ) ) ;
#63010 = CARTESIAN_POINT ( 'NONE',  ( 15.93750000122903110, 6.123233995736764310E-16, -4.999999999999998224 ) ) ;
#63011 = CARTESIAN_POINT ( 'NONE',  ( 11.91562500061451857, -6.054752690667223547, -1.112240025338166033E-15 ) ) ;
#63012 = CARTESIAN_POINT ( 'NONE',  ( 17.01562500061451644, 3.027376345333613106, -5.243569643749998122 ) ) ;
#63013 = CARTESIAN_POINT ( 'NONE',  ( 26.66250000122903430, -4.330127018922190985, -2.500000000000001332 ) ) ;
#63014 = CARTESIAN_POINT ( 'NONE',  ( 20.81250000000000000, 2.886751345948129099, -4.999999999999998224 ) ) ;
#63015 = CARTESIAN_POINT ( 'NONE',  ( 24.42187500061451999, 3.027376345333611329, 5.243569643749999010 ) ) ;
#63016 = CARTESIAN_POINT ( 'NONE',  ( 25.27499999999999858, 6.123233995736764310E-16, -4.999999999999998224 ) ) ;
#63017 = CARTESIAN_POINT ( 'NONE',  ( 9.412500001229034297, 0.000000000000000000, 4.999999999999998224 ) ) ;
#63018 = CARTESIAN_POINT ( 'NONE',  ( 9.346875000614517148, -3.027376345333610441, -5.243569643749999898 ) ) ;
#63019 = CARTESIAN_POINT ( 'NONE',  ( 25.84687500061451360, -3.027376345333614438, 5.243569643749998122 ) ) ;
#63020 = DIRECTION ( 'NONE',  ( -1.000000000000000000, -0.000000000000000000, -0.000000000000000000 ) ) ;
#63021 = CARTESIAN_POINT ( 'NONE',  ( 20.99062500061451431, -3.027376345333610441, -5.243569643749999898 ) ) ;
#63022 = CARTESIAN_POINT ( 'NONE',  ( 26.85937500061451644, -4.541064518000417216, -2.621784821875001281 ) ) ;
#63023 = CARTESIAN_POINT ( 'NONE',  ( -3.756430356250000990, 16.16562499938548569, 32.16877607737301048 ) ) ;
#63024 = CARTESIAN_POINT ( 'NONE',  ( 18.56250000000000000, 2.886751345948129099, -4.999999999999997335 ) ) ;
#63025 = CARTESIAN_POINT ( 'NONE',  ( 7.884375000614517681, -4.541064518000419881, 2.621784821874995952 ) ) ;
#63026 = CARTESIAN_POINT ( 'NONE',  ( 19.19062500061452070, -3.027376345333610441, -5.243569643749999898 ) ) ;
#63027 = CARTESIAN_POINT ( 'NONE',  ( -5.000000000000000000, 39.99999999999999289, 15.00000000000000178 ) ) ;
#63028 = CARTESIAN_POINT ( 'NONE',  ( 28.34062500061451928, 6.054752690667223547, 3.707466751127219781E-16 ) ) ;
#63029 = CARTESIAN_POINT ( 'NONE',  ( 4.396875000614516971, -3.027376345333610441, -5.243569643749999898 ) ) ;
#63030 = CARTESIAN_POINT ( 'NONE',  ( 4.898587196589411843E-16, 20.00000000000000000, -26.00000000000000000 ) ) ;
#63031 = CARTESIAN_POINT ( 'NONE',  ( 4.040625000614517681, 6.054752690667223547, 3.707466751127219781E-16 ) ) ;
#63032 = CARTESIAN_POINT ( 'NONE',  ( 18.22499999999999787, 4.330127018922191873, 2.499999999999999556 ) ) ;
#63033 = ORIENTED_EDGE ( 'NONE', *, *, #31877, .F. ) ;
#63034 = CARTESIAN_POINT ( 'NONE',  ( 25.08749999999999858, -2.886751345948129988, 4.999999999999997335 ) ) ;
#63035 =( BOUNDED_CURVE ( )  B_SPLINE_CURVE ( 2, ( #55675, #4710, #72671, #5072, #33858, #27241, #50141 ),
 .UNSPECIFIED., .F., .F. ) 
 B_SPLINE_CURVE_WITH_KNOTS ( ( 3, 2, 2, 3 ),
 ( 0.4166666666666667407, 0.4194444444444445086, 0.4222222222222222210, 0.4249999999999999889 ),
 .UNSPECIFIED. ) 
 CURVE ( )  GEOMETRIC_REPRESENTATION_ITEM ( )  RATIONAL_B_SPLINE_CURVE ( ( 0.9999999999999973355, 0.8660254037844413721, 1.000000000000000000, 0.8660254037844387076, 1.000000000000000000, 0.8660254037844387076, 1.000000000000000000 ) ) 
 REPRESENTATION_ITEM ( '' )  );
#63036 = CARTESIAN_POINT ( 'NONE',  ( 27.38437500061451857, 6.421520780324663323E-16, -5.243569643749999010 ) ) ;
#63037 = VERTEX_POINT ( 'NONE', #39464 ) ;
#63038 = CARTESIAN_POINT ( 'NONE',  ( 14.69062500061451537, -3.027376345333610441, -5.243569643749999898 ) ) ;
#63039 = CARTESIAN_POINT ( 'NONE',  ( 6.365625000614518747, 3.027376345333611329, 5.243569643749999010 ) ) ;
#63040 = CARTESIAN_POINT ( 'NONE',  ( 19.58437500061451786, -2.746126346562642428, -4.756430356249999214 ) ) ;
#63041 = CARTESIAN_POINT ( 'NONE',  ( 4.884375000614518569, 6.421520780324663323E-16, -5.243569643749999010 ) ) ;
#63042 = CARTESIAN_POINT ( 'NONE',  ( 15.48750000122903359, 6.123233995736764310E-16, -4.999999999999998224 ) ) ;
#63043 = CARTESIAN_POINT ( 'NONE',  ( 21.67500000000000071, 6.123233995736764310E-16, -4.999999999999998224 ) ) ;
#63044 = CARTESIAN_POINT ( 'NONE',  ( 28.46249999999999858, 2.886751345948129099, -4.999999999999998224 ) ) ;
#63045 = CARTESIAN_POINT ( 'NONE',  ( 4.134375000614517681, 4.541064518000418104, 2.621784821874999949 ) ) ;
#63046 = CARTESIAN_POINT ( 'NONE',  ( 9.534375000614517148, 4.541064518000418104, 2.621784821874999949 ) ) ;
#63047 = CARTESIAN_POINT ( 'NONE',  ( 20.78437500061451715, 4.541064518000418104, 2.621784821874999949 ) ) ;
#63048 = CARTESIAN_POINT ( 'NONE',  ( 9.750000000000001776, 0.000000000000000000, 4.999999999999998224 ) ) ;
#63049 = ORIENTED_EDGE ( 'NONE', *, *, #70507, .F. ) ;
#63050 = CARTESIAN_POINT ( 'NONE',  ( 4.209375000614516971, 0.000000000000000000, 5.243569643749999010 ) ) ;
#63051 = CARTESIAN_POINT ( 'NONE',  ( 5.475000000000000533, 6.123233995736764310E-16, -4.999999999999998224 ) ) ;
#63052 = CARTESIAN_POINT ( 'NONE',  ( 6.421875000614519102, 3.027376345333611329, 5.243569643749999010 ) ) ;
#63053 = CARTESIAN_POINT ( 'NONE',  ( 18.75000000000000000, 0.000000000000000000, 4.999999999999998224 ) ) ;
#63054 = CARTESIAN_POINT ( 'NONE',  ( 15.25312500061451715, 4.541064518000418104, -2.621784821874998173 ) ) ;
#63055 = CARTESIAN_POINT ( 'NONE',  ( 4.000000000000000000, 19.73749999999999716, 27.69059892324149530 ) ) ;
#63056 = LINE ( 'NONE', #17621, #46931 ) ;
#63057 = CARTESIAN_POINT ( 'NONE',  ( 19.54687500061451644, -2.746126346562646425, 4.756430356249996549 ) ) ;
#63058 = CARTESIAN_POINT ( 'NONE',  ( 9.253125000614517148, -4.541064518000417216, -2.621784821875001281 ) ) ;
#63059 = CARTESIAN_POINT ( 'NONE',  ( 27.72187500061451715, -6.054752690667223547, -1.112240025338166033E-15 ) ) ;
#63060 = CARTESIAN_POINT ( 'NONE',  ( -4.243569643749999898, 19.82187500061451857, 27.54997392385601529 ) ) ;
#63061 = CARTESIAN_POINT ( 'NONE',  ( 25.84687500061451360, -3.027376345333614438, 5.243569643749998122 ) ) ;
#63062 = CARTESIAN_POINT ( 'NONE',  ( 8.662499999999999645, 2.886751345948129099, -4.999999999999998224 ) ) ;
#63063 = CARTESIAN_POINT ( 'NONE',  ( 3.999999999999999112, 12.68750000122903465, 30.00000000000000000 ) ) ;
#63064 = CARTESIAN_POINT ( 'NONE',  ( 13.97812500061451679, 4.541064518000418104, 2.621784821874999949 ) ) ;
#63065 = CARTESIAN_POINT ( 'NONE',  ( 7.200000001229035718, -2.886751345948129988, 4.999999999999997335 ) ) ;
#63066 = ADVANCED_FACE ( 'NONE', ( #66074 ), #43919, .F. ) ;
#63067 = CARTESIAN_POINT ( 'NONE',  ( 17.63437500061451502, 4.541064518000418104, 2.621784821874999949 ) ) ;
#63068 = CARTESIAN_POINT ( 'NONE',  ( 11.63437500061451857, 6.421520780324663323E-16, -5.243569643749999010 ) ) ;
#63069 = CARTESIAN_POINT ( 'NONE',  ( -3.963752180954430493, 3.047823949009541344, -29.44540563775499820 ) ) ;
#63070 = EDGE_LOOP ( 'NONE', ( #56601, #41481, #22707, #14567 ) ) ;
#63071 = VECTOR ( 'NONE', #39508, 1000.000000000000000 ) ;
#63072 = CARTESIAN_POINT ( 'NONE',  ( 13.37812500061451715, 6.421520780324663323E-16, -5.243569643749999010 ) ) ;
#63073 = CARTESIAN_POINT ( 'NONE',  ( 26.70000000122903572, -2.886751345948125991, -5.000000000000000000 ) ) ;
#63074 = CARTESIAN_POINT ( 'NONE',  ( 12.79687500061451821, -3.027376345333614438, 5.243569643749998122 ) ) ;
#63075 = CARTESIAN_POINT ( 'NONE',  ( 4.059375000614519280, 4.541064518000418104, -2.621784821874998173 ) ) ;
#63076 = CARTESIAN_POINT ( 'NONE',  ( 13.67812500061451786, -4.541064518000419881, 2.621784821874995952 ) ) ;
#63077 = EDGE_CURVE ( 'NONE', #7820, #16810, #26932, .T. ) ;
#63078 = CARTESIAN_POINT ( 'NONE',  ( 1.071796769724489895, 18.96740381056766722, -34.00000000000000000 ) ) ;
#63079 = CARTESIAN_POINT ( 'NONE',  ( 22.84687500061451715, -3.027376345333610441, -5.243569643749999898 ) ) ;
#63080 = CARTESIAN_POINT ( 'NONE',  ( -4.243569643749997233, 10.84062500061451395, 32.45002607614398471 ) ) ;
#63081 = CARTESIAN_POINT ( 'NONE',  ( 10.61250000122903536, 4.330127018922192761, -2.499999999999997780 ) ) ;
#63082 = DIRECTION ( 'NONE',  ( 0.000000000000000000, 0.000000000000000000, 1.000000000000000000 ) ) ;
#63083 = CARTESIAN_POINT ( 'NONE',  ( 1.510657702057710734E-15, 19.43750000000000000, 26.00000000000000000 ) ) ;
#63084 = CARTESIAN_POINT ( 'NONE',  ( 2.121784821874999061, 17.00937500061451857, -33.67503911421598417 ) ) ;
#63085 = ADVANCED_FACE ( 'NONE', ( #5120 ), #55726, .F. ) ;
#63086 = CARTESIAN_POINT ( 'NONE',  ( 18.72187500061451360, -6.054752690667223547, -1.112240025338166033E-15 ) ) ;
#63087 = CARTESIAN_POINT ( 'NONE',  ( 20.02500000122903145, 2.886751345948129099, -4.999999999999998224 ) ) ;
#63088 = CARTESIAN_POINT ( 'NONE',  ( 13.84687500061451537, -3.027376345333610441, -5.243569643749999898 ) ) ;
#63089 = CARTESIAN_POINT ( 'NONE',  ( 4.243569643749999898, 19.54062500061451857, -27.54997392385601529 ) ) ;
#63090 = CARTESIAN_POINT ( 'NONE',  ( 18.93750000122903288, -4.330127018922194537, 2.499999999999995559 ) ) ;
#63091 = CARTESIAN_POINT ( 'NONE',  ( 14.80312500061451608, 4.541064518000418104, -2.621784821874998173 ) ) ;
#63092 = ORIENTED_EDGE ( 'NONE', *, *, #32653, .T. ) ;
#63093 = ORIENTED_EDGE ( 'NONE', *, *, #6767, .T. ) ;
#63094 = CARTESIAN_POINT ( 'NONE',  ( 17.69999999999999929, 4.330127018922192761, -2.499999999999997780 ) ) ;
#63095 = CARTESIAN_POINT ( 'NONE',  ( 5.857864376269046325, 9.999999999999998224, -5.857864376269046325 ) ) ;
#63096 = CARTESIAN_POINT ( 'NONE',  ( 3.992981257374419890, 3.009426956198104186, 30.27415453858231942 ) ) ;
#63097 = CARTESIAN_POINT ( 'NONE',  ( 14.96250000122903323, -4.330127018922190985, -2.500000000000001332 ) ) ;
#63098 = CARTESIAN_POINT ( 'NONE',  ( 27.38437500061451857, 6.421520780324663323E-16, -5.243569643749999010 ) ) ;
#63099 = CARTESIAN_POINT ( 'NONE',  ( 19.41562500061451146, 3.027376345333611329, 5.243569643749999010 ) ) ;
#63100 = CARTESIAN_POINT ( 'NONE',  ( 24.17812500061451786, 6.421520780324663323E-16, -5.243569643749999010 ) ) ;
#63101 = CARTESIAN_POINT ( 'NONE',  ( 3.328125000614516438, -4.541064518000419881, 2.621784821874995952 ) ) ;
#63102 =( BOUNDED_CURVE ( )  B_SPLINE_CURVE ( 2, ( #9472, #60061, #49368, #19806, #2829, #3939, #59322 ),
 .UNSPECIFIED., .F., .F. ) 
 B_SPLINE_CURVE_WITH_KNOTS ( ( 3, 2, 2, 3 ),
 ( 0.9600368262957028609, 0.9611111111111111382, 0.9638888888888889062, 0.9648669314804571018 ),
 .UNSPECIFIED. ) 
 CURVE ( )  GEOMETRIC_REPRESENTATION_ITEM ( )  RATIONAL_B_SPLINE_CURVE ( ( 0.9364497541642147205, 0.9481863252286599764, 1.000000000000000000, 0.8660254037844387076, 1.000000000000000000, 0.9528281699366905055, 0.9388743022987573461 ) ) 
 REPRESENTATION_ITEM ( '' )  );
#63103 = CARTESIAN_POINT ( 'NONE',  ( 28.72500000000000142, -4.330127018922194537, 2.499999999999995559 ) ) ;
#63104 = CARTESIAN_POINT ( 'NONE',  ( 4.633613603196540254, 1.878729617659674167, 4.895446622381335544 ) ) ;
#63105 = CARTESIAN_POINT ( 'NONE',  ( 8.521875000614516082, 2.746126346562645981, -4.756430356249997438 ) ) ;
#63106 = CARTESIAN_POINT ( 'NONE',  ( 4.000000000000000000, 17.93750000000000355, 27.69059892324149885 ) ) ;
#63107 = CARTESIAN_POINT ( 'NONE',  ( 28.68749999999999289, -2.886751345948114000, 5.000000000000024869 ) ) ;
#63108 = CARTESIAN_POINT ( 'NONE',  ( -2.121784821874996840, 16.78437500061452070, -26.32496088578401583 ) ) ;
#63109 = EDGE_CURVE ( 'NONE', #65422, #38854, #49098, .T. ) ;
#63110 = CARTESIAN_POINT ( 'NONE',  ( 5.812500001229035540, 0.000000000000000000, 4.999999999999998224 ) ) ;
#63111 = CARTESIAN_POINT ( 'NONE',  ( 5.437500000000001776, -2.886751345948125991, -5.000000000000000000 ) ) ;
#63112 = CARTESIAN_POINT ( 'NONE',  ( 4.425000001229032698, 2.886751345948126879, 4.999999999999999112 ) ) ;
#63113 = CARTESIAN_POINT ( 'NONE',  ( 9.346875000614517148, -3.027376345333610441, -5.243569643749999898 ) ) ;
#63114 = CARTESIAN_POINT ( 'NONE',  ( 24.56250000122903288, 4.330127018922192761, -2.499999999999997780 ) ) ;
#63115 = DIRECTION ( 'NONE',  ( 0.000000000000000000, 0.000000000000000000, 1.000000000000000000 ) ) ;
#63116 = CARTESIAN_POINT ( 'NONE',  ( -6.000139530219994910, 7.999895352344700505, -29.59567021705531786 ) ) ;
#63117 = VECTOR ( 'NONE', #70108, 1000.000000000000000 ) ;
#63118 = CARTESIAN_POINT ( 'NONE',  ( 9.750000000000001776, 0.000000000000000000, 4.999999999999998224 ) ) ;
#63119 = CARTESIAN_POINT ( 'NONE',  ( 8.746875000614515727, -3.027376345333614438, 5.243569643749998122 ) ) ;
#63120 = CARTESIAN_POINT ( 'NONE',  ( 14.18437500061451750, -4.541064518000419881, 2.621784821874995952 ) ) ;
#63121 = CARTESIAN_POINT ( 'NONE',  ( 6.487499999999999822, 5.773502691896255534, 3.535250795749688894E-16 ) ) ;
#63122 = CARTESIAN_POINT ( 'NONE',  ( 9.001249775931846008E-16, 16.31562500061459531, 34.90005215228797653 ) ) ;
#63123 = CARTESIAN_POINT ( 'NONE',  ( 20.89687500061452141, -3.027376345333614438, 5.243569643749998122 ) ) ;
#63124 = CARTESIAN_POINT ( 'NONE',  ( 9.600000000000001421, 4.330127018922192761, -2.499999999999997780 ) ) ;
#63125 = CARTESIAN_POINT ( 'NONE',  ( 27.11250000122903359, -4.330127018922190985, -2.500000000000001332 ) ) ;
#63126 = CARTESIAN_POINT ( 'NONE',  ( 16.84687500061451715, -4.119189519843965641, -2.378215178125001383 ) ) ;
#63127 = CARTESIAN_POINT ( 'NONE',  ( 21.70312500061451644, 0.000000000000000000, 5.243569643749999010 ) ) ;
#63128 = CARTESIAN_POINT ( 'NONE',  ( 12.14062500061451821, 6.054752690667223547, 3.707466751127219781E-16 ) ) ;
#63129 = CARTESIAN_POINT ( 'NONE',  ( 27.04687500061451289, 0.000000000000000000, 4.756430356249998326 ) ) ;
#63130 = CARTESIAN_POINT ( 'NONE',  ( 12.38437500061451857, -4.541064518000419881, 2.621784821874995952 ) ) ;
#63131 = CARTESIAN_POINT ( 'NONE',  ( 29.43750000000000000, 5.773502691896255534, 3.535250795749688894E-16 ) ) ;
#63132 = CARTESIAN_POINT ( 'NONE',  ( 23.32500000122903572, 2.886751345948126879, 4.999999999999999112 ) ) ;
#63133 = FACE_OUTER_BOUND ( 'NONE', #62791, .T. ) ;
#63134 = AXIS2_PLACEMENT_3D ( 'NONE', #36850, #64924, #42402 ) ;
#63135 = CARTESIAN_POINT ( 'NONE',  ( 10.73437500061451644, 6.421520780324663323E-16, -5.243569643749999010 ) ) ;
#63136 = CARTESIAN_POINT ( 'NONE',  ( 28.35937500061451289, 4.541064518000418104, -2.621784821874998173 ) ) ;
#63137 = CARTESIAN_POINT ( 'NONE',  ( 3.534375000614518036, 6.421520780324663323E-16, -5.243569643749999010 ) ) ;
#63138 = CARTESIAN_POINT ( 'NONE',  ( -1.071796769724488563, 13.00490381179669974, -26.00000000000000000 ) ) ;
#63139 = CARTESIAN_POINT ( 'NONE',  ( 21.34687500061451715, -3.027376345333614438, 5.243569643749998122 ) ) ;
#63140 = CARTESIAN_POINT ( 'NONE',  ( 13.69687500061451679, -3.027376345333614438, 5.243569643749998122 ) ) ;
#63141 = CARTESIAN_POINT ( 'NONE',  ( -1.878215178124999163, 18.30312499938548143, 26.74683588394047007 ) ) ;
#63142 = CARTESIAN_POINT ( 'NONE',  ( 24.89999999999999858, 4.330127018922192761, -2.499999999999997780 ) ) ;
#63143 = CARTESIAN_POINT ( 'NONE',  ( -3.756430356249999214, 20.02812499938548285, 27.83122392262697531 ) ) ;
#63144 = CARTESIAN_POINT ( 'NONE',  ( 26.18437500061451573, 4.119189519843966529, 2.378215178124999607 ) ) ;
#63145 = CARTESIAN_POINT ( 'NONE',  ( 16.64062500061451289, 6.054752690667223547, 3.707466751127219781E-16 ) ) ;
#63146 = CARTESIAN_POINT ( 'NONE',  ( 7.350000000000002309, 4.330127018922192761, -2.499999999999997780 ) ) ;
#63147 = CARTESIAN_POINT ( 'NONE',  ( 0.000000000000000000, 25.54316770519903557, 26.00000000000000000 ) ) ;
#63148 = CARTESIAN_POINT ( 'NONE',  ( 14.17500000000000071, 4.330127018922191873, 2.499999999999999556 ) ) ;
#63149 = CARTESIAN_POINT ( 'NONE',  ( -4.243569643749999898, 10.35312500061451857, 30.00000000000000000 ) ) ;
#63150 = LINE ( 'NONE', #12545, #36023 ) ;
#63151 = CARTESIAN_POINT ( 'NONE',  ( 24.57187500061451502, -6.054752690667223547, -1.112240025338166033E-15 ) ) ;
#63152 = ORIENTED_EDGE ( 'NONE', *, *, #19846, .F. ) ;
#63153 = CARTESIAN_POINT ( 'NONE',  ( 23.01562500061451644, 3.027376345333611329, 5.243569643749999010 ) ) ;
#63154 = CARTESIAN_POINT ( 'NONE',  ( 20.48437500061451289, -4.541064518000419881, 2.621784821874995952 ) ) ;
#63155 = CARTESIAN_POINT ( 'NONE',  ( 4.537500000000000533, -2.886751345948125991, -5.000000000000000000 ) ) ;
#63156 = CARTESIAN_POINT ( 'NONE',  ( 6.965625000614518392, -6.054752690667223547, -1.112240025338166033E-15 ) ) ;
#63157 = CARTESIAN_POINT ( 'NONE',  ( 21.55312500061451431, 4.541064518000418104, -2.621784821874998173 ) ) ;
#63158 = CARTESIAN_POINT ( 'NONE',  ( 12.98437500061451821, 6.421520780324663323E-16, -5.243569643749999010 ) ) ;
#63159 = CARTESIAN_POINT ( 'NONE',  ( 17.97187500061451715, 3.027376345333613106, -5.243569643749998122 ) ) ;
#63160 = CARTESIAN_POINT ( 'NONE',  ( -4.243569643749999898, 17.06562500061451360, 27.54997392385601529 ) ) ;
#63161 = CARTESIAN_POINT ( 'NONE',  ( 19.27500000122903145, 2.886751345948126879, 4.999999999999999112 ) ) ;
#63162 = CARTESIAN_POINT ( 'NONE',  ( 15.30937500061451750, 4.119189519843966529, -2.378215178124998275 ) ) ;
#63163 = CARTESIAN_POINT ( 'NONE',  ( 10.07812500061451644, -4.541064518000419881, 2.621784821874995952 ) ) ;
#63164 = CARTESIAN_POINT ( 'NONE',  ( 5.259375000614518569, -4.541064518000417216, -2.621784821875001281 ) ) ;
#63165 = CARTESIAN_POINT ( 'NONE',  ( 5.521875000614517859, 3.027376345333611329, 5.243569643749999010 ) ) ;
#63166 = EDGE_CURVE ( 'NONE', #48969, #48104, #44731, .T. ) ;
#63167 = CARTESIAN_POINT ( 'NONE',  ( 26.44687500061451502, -3.027376345333610441, -5.243569643749999898 ) ) ;
#63168 = CARTESIAN_POINT ( 'NONE',  ( 17.84062500061451573, -3.027376345333610441, -5.243569643749999898 ) ) ;
#63169 = CARTESIAN_POINT ( 'NONE',  ( 28.01250000122903216, -4.330127018922190985, -2.500000000000001332 ) ) ;
#63170 = CARTESIAN_POINT ( 'NONE',  ( 26.42812500061451431, 6.421520780324663323E-16, -5.243569643749999010 ) ) ;
#63171 = CARTESIAN_POINT ( 'NONE',  ( 22.95937500061451431, 4.541064518000418104, -2.621784821874998173 ) ) ;
#63172 = CARTESIAN_POINT ( 'NONE',  ( 17.39062500061451644, -3.027376345333610441, -5.243569643749999898 ) ) ;
#63173 = CARTESIAN_POINT ( 'NONE',  ( -2.121784821874999949, 17.53437500061451715, 26.32496088578401938 ) ) ;
#63174 = AXIS2_PLACEMENT_3D ( 'NONE', #47459, #35642, #58891 ) ;
#63175 = CARTESIAN_POINT ( 'NONE',  ( 21.21562500061451573, 3.027376345333611329, 5.243569643749999010 ) ) ;
#63176 = CARTESIAN_POINT ( 'NONE',  ( 3.412500001229032964, 4.330127018922192761, -2.499999999999997780 ) ) ;
#63177 = VERTEX_POINT ( 'NONE', #16550 ) ;
#63178 = CARTESIAN_POINT ( 'NONE',  ( 26.32499999999999929, 4.330127018922191873, 2.499999999999999556 ) ) ;
#63179 = CARTESIAN_POINT ( 'NONE',  ( -3.999999999999999556, 13.66250000000000142, -32.30940107675850470 ) ) ;
#63180 = CARTESIAN_POINT ( 'NONE',  ( 28.15312500061451573, -4.541064518000417216, -2.621784821875001281 ) ) ;
#63181 = CARTESIAN_POINT ( 'NONE',  ( 10.30312500061451431, 4.541064518000418104, -2.621784821874998173 ) ) ;
#63182 = CARTESIAN_POINT ( 'NONE',  ( 23.02500000122903145, -5.773502691896255534, -1.060575238724906372E-15 ) ) ;
#63183 = CARTESIAN_POINT ( 'NONE',  ( 26.87812500061451360, 6.421520780324663323E-16, -5.243569643749999010 ) ) ;
#63184 = CARTESIAN_POINT ( 'NONE',  ( 28.49999999999999645, 4.330127018922192761, -2.499999999999997780 ) ) ;
#63185 = CARTESIAN_POINT ( 'NONE',  ( 4.000000000000000000, 16.70000000122903572, -27.69059892324149530 ) ) ;
#63186 = CARTESIAN_POINT ( 'NONE',  ( 29.46562500061451573, -6.054752690667223547, -1.112240025338166033E-15 ) ) ;
#63187 = CARTESIAN_POINT ( 'NONE',  ( 10.86562500061451431, 3.027376345333611329, 5.243569643749999010 ) ) ;
#63188 = ORIENTED_EDGE ( 'NONE', *, *, #70897, .T. ) ;
#63189 = AXIS2_PLACEMENT_3D ( 'NONE', #6133, #44942, #5412 ) ;
#63190 = CARTESIAN_POINT ( 'NONE',  ( 25.37812500061451715, -4.541064518000419881, 2.621784821874995952 ) ) ;
#63191 = CARTESIAN_POINT ( 'NONE',  ( 7.003125000614518036, -4.541064518000417216, -2.621784821875001281 ) ) ;
#63192 = AXIS2_PLACEMENT_3D ( 'NONE', #66722, #33449, #33090 ) ;
#63193 = CARTESIAN_POINT ( 'NONE',  ( 5.953125000614519102, 0.000000000000000000, 5.243569643749999010 ) ) ;
#63194 = CARTESIAN_POINT ( 'NONE',  ( 17.14687500061451786, 5.492252693125287522, 3.363034840372157021E-16 ) ) ;
#63195 = CYLINDRICAL_SURFACE ( 'NONE', #68038, 4.999999999999998224 ) ;
#63196 = CARTESIAN_POINT ( 'NONE',  ( 13.57500000000000107, 6.123233995736764310E-16, -4.999999999999998224 ) ) ;
#63197 = CARTESIAN_POINT ( 'NONE',  ( 14.52187500061451608, 3.027376345333611329, 5.243569643749999010 ) ) ;
#63198 = CARTESIAN_POINT ( 'NONE',  ( 11.55000000122903181, 5.773502691896255534, 3.535250795749688894E-16 ) ) ;
#63199 = CARTESIAN_POINT ( 'NONE',  ( 18.04687500061451999, 6.054752690667223547, 3.707466751127219781E-16 ) ) ;
#63200 = CARTESIAN_POINT ( 'NONE',  ( 16.98750000000000426, -2.886751345948129988, 4.999999999999997335 ) ) ;
#63201 = CARTESIAN_POINT ( 'NONE',  ( 20.18437500061451573, 6.421520780324663323E-16, -5.243569643749999010 ) ) ;
#63202 = CARTESIAN_POINT ( 'NONE',  ( -4.243569643749999898, 11.21562500061451750, -32.45002607614398471 ) ) ;
#63203 = CYLINDRICAL_SURFACE ( 'NONE', #2926, 4.999999999999998224 ) ;
#63204 = CARTESIAN_POINT ( 'NONE',  ( 22.88437500061451502, 5.492252693125287522, 3.363034840372157021E-16 ) ) ;
#63205 = CARTESIAN_POINT ( 'NONE',  ( 1.999999999999998668, 11.75000000000000178, -33.46410161513775705 ) ) ;
#63206 = EDGE_CURVE ( 'NONE', #3601, #4240, #2631, .T. ) ;
#63207 = CARTESIAN_POINT ( 'NONE',  ( 24.51562500061451289, -6.054752690667223547, -1.112240025338166033E-15 ) ) ;
#63208 = CARTESIAN_POINT ( 'NONE',  ( 17.10000000122903430, -2.886751345948096681, 5.000000000000054179 ) ) ;
#63209 = CARTESIAN_POINT ( 'NONE',  ( 29.22187500061451715, 3.027376345333613106, -5.243569643749998122 ) ) ;
#63210 = CARTESIAN_POINT ( 'NONE',  ( 25.19999999999999929, -4.330127018922190985, -2.500000000000001332 ) ) ;
#63211 = CARTESIAN_POINT ( 'NONE',  ( 5.765625000614519102, 3.027376345333613106, -5.243569643749998122 ) ) ;
#63212 = CARTESIAN_POINT ( 'NONE',  ( 24.87187500061451217, -4.119189519843968306, 2.378215178124996054 ) ) ;
#63213 = CARTESIAN_POINT ( 'NONE',  ( 18.27187500061451431, -6.054752690667223547, -1.112240025338166033E-15 ) ) ;
#63214 = CARTESIAN_POINT ( 'NONE',  ( 11.18437500061451573, 5.492252693125287522, 3.363034840372157021E-16 ) ) ;
#63215 = AXIS2_PLACEMENT_3D ( 'NONE', #43754, #66279, #38943 ) ;
#63216 = CARTESIAN_POINT ( 'NONE',  ( 28.87500000122902932, -5.773502691896255534, -1.060575238724906372E-15 ) ) ;
#63217 = CARTESIAN_POINT ( 'NONE',  ( 8.184375000614515727, 4.541064518000418104, 2.621784821874999949 ) ) ;
#63218 = ORIENTED_EDGE ( 'NONE', *, *, #458, .F. ) ;
#63219 = CARTESIAN_POINT ( 'NONE',  ( 18.53437500061451715, 4.541064518000418104, 2.621784821874999949 ) ) ;
#63220 = CARTESIAN_POINT ( 'NONE',  ( 3.242103837493086330E-14, 12.80000000122903359, -34.00000000000000000 ) ) ;
#63221 = CARTESIAN_POINT ( 'NONE',  ( 25.50000000000000000, 0.000000000000000000, 4.999999999999998224 ) ) ;
#63222 = CARTESIAN_POINT ( 'NONE',  ( 29.33437500061451431, 4.541064518000418104, 2.621784821874999949 ) ) ;
#63223 = CARTESIAN_POINT ( 'NONE',  ( 19.27500000000000213, -4.330127018922194537, 2.499999999999995559 ) ) ;
#63224 = CARTESIAN_POINT ( 'NONE',  ( 10.68749999999999645, -2.886751345948063374, 5.000000000000112799 ) ) ;
#63225 = EDGE_LOOP ( 'NONE', ( #31832, #14981, #20372, #21900 ) ) ;
#63226 = CARTESIAN_POINT ( 'NONE',  ( 9.600000000000001421, 4.330127018922192761, -2.499999999999997780 ) ) ;
#63227 = CARTESIAN_POINT ( 'NONE',  ( 11.85937500061451821, -5.492252693125287522, -1.008910452111647106E-15 ) ) ;
#63228 = CARTESIAN_POINT ( 'NONE',  ( 24.74062500061451786, 6.054752690667223547, 3.707466751127219781E-16 ) ) ;
#63229 = CARTESIAN_POINT ( 'NONE',  ( 14.58750000000000036, 5.773502691896255534, 3.535250795749688894E-16 ) ) ;
#63230 = CARTESIAN_POINT ( 'NONE',  ( 10.35000000122903074, -2.886751345948129988, 4.999999999999997335 ) ) ;
#63231 = CARTESIAN_POINT ( 'NONE',  ( 8.390625000614518214, -3.027376345333610441, -5.243569643749999898 ) ) ;
#63232 = CARTESIAN_POINT ( 'NONE',  ( 21.26249999999999574, 2.886751345948129099, -4.999999999999998224 ) ) ;
#63233 = CARTESIAN_POINT ( 'NONE',  ( 21.96562500061451573, 3.027376345333613106, -5.243569643749998122 ) ) ;
#63234 = DIRECTION ( 'NONE',  ( -1.000000000000000000, -0.000000000000000000, -0.000000000000000000 ) ) ;
#63235 = CARTESIAN_POINT ( 'NONE',  ( 26.73750000122903003, 6.123233995736764310E-16, -4.999999999999998224 ) ) ;
#63236 = CARTESIAN_POINT ( 'NONE',  ( 2.655984681222220721E-16, 16.80312499938548498, 25.66244784525396483 ) ) ;
#63237 = CARTESIAN_POINT ( 'NONE',  ( 7.800000000000001599, 4.330127018922192761, -2.499999999999997780 ) ) ;
#63238 = ORIENTED_EDGE ( 'NONE', *, *, #18393, .T. ) ;
#63239 = CARTESIAN_POINT ( 'NONE',  ( 22.07812500061451644, 4.541064518000418104, 2.621784821874999949 ) ) ;
#63240 = CARTESIAN_POINT ( 'NONE',  ( 29.61562500061451431, 3.027376345333613106, -5.243569643749998122 ) ) ;
#63241 = CARTESIAN_POINT ( 'NONE',  ( 27.38437500061451857, 6.421520780324663323E-16, -5.243569643749999010 ) ) ;
#63242 = CARTESIAN_POINT ( 'NONE',  ( 19.95937500061451786, 0.000000000000000000, 5.243569643749999010 ) ) ;
#63243 = CARTESIAN_POINT ( 'NONE',  ( 15.32812500061451644, 4.541064518000418104, 2.621784821874999949 ) ) ;
#63244 = CARTESIAN_POINT ( 'NONE',  ( 29.84999999999999787, 4.330127018922192761, -2.499999999999997780 ) ) ;
#63245 = CARTESIAN_POINT ( 'NONE',  ( 25.46250000122903501, 4.330127018922192761, -2.499999999999997780 ) ) ;
#63246 = CARTESIAN_POINT ( 'NONE',  ( 21.72187500061451715, 2.746126346562643317, 4.756430356249998326 ) ) ;
#63247 = CARTESIAN_POINT ( 'NONE',  ( 17.39062500061451644, -3.027376345333610441, -5.243569643749999898 ) ) ;
#63248 = FACE_OUTER_BOUND ( 'NONE', #15702, .T. ) ;
#63249 = EDGE_CURVE ( 'NONE', #72719, #42898, #52263, .T. ) ;
#63250 =( BOUNDED_CURVE ( )  B_SPLINE_CURVE ( 2, ( #23715, #7461, #18160, #40728, #35889, #7102, #46626 ),
 .UNSPECIFIED., .F., .F. ) 
 B_SPLINE_CURVE_WITH_KNOTS ( ( 3, 2, 2, 3 ),
 ( 0.7700000000000001288, 0.7733333333333334281, 0.7766666666666667274, 0.7800000000000001377 ),
 .UNSPECIFIED. ) 
 CURVE ( )  GEOMETRIC_REPRESENTATION_ITEM ( )  RATIONAL_B_SPLINE_CURVE ( ( 0.9999999999999955591, 0.8660254037844431485, 1.000000000000000000, 0.8660254037844387076, 1.000000000000000000, 0.8660254037844342667, 1.000000000000004441 ) ) 
 REPRESENTATION_ITEM ( '' )  );
#63251 = CARTESIAN_POINT ( 'NONE',  ( 13.77187500061451786, -6.054752690667223547, -1.112240025338166033E-15 ) ) ;
#63252 = CARTESIAN_POINT ( 'NONE',  ( 11.97187500061451892, -6.054752690667223547, -1.112240025338166033E-15 ) ) ;
#63253 = CARTESIAN_POINT ( 'NONE',  ( 21.15937500061451715, 4.541064518000418104, -2.621784821874998173 ) ) ;
#63254 = ORIENTED_EDGE ( 'NONE', *, *, #62341, .F. ) ;
#63255 = LINE ( 'NONE', #23725, #14660 ) ;
#63256 = CARTESIAN_POINT ( 'NONE',  ( 23.42812500061451786, 4.541064518000418104, 2.621784821874999949 ) ) ;
#63257 = CARTESIAN_POINT ( 'NONE',  ( 19.32187500061451857, 3.027376345333613106, -5.243569643749998122 ) ) ;
#63258 = CARTESIAN_POINT ( 'NONE',  ( 24.40312500061451573, 0.000000000000000000, 5.243569643749999010 ) ) ;
#63259 = CARTESIAN_POINT ( 'NONE',  ( -3.999999999999999112, 9.725000001229036073, 27.69059892324149885 ) ) ;
#63260 = CARTESIAN_POINT ( 'NONE',  ( -3.999999999999999556, 13.66250000000000142, 27.69059892324149530 ) ) ;
#63261 = CARTESIAN_POINT ( 'NONE',  ( 3.309375000614518836, 0.000000000000000000, 5.243569643749999010 ) ) ;
#63262 = CARTESIAN_POINT ( 'NONE',  ( 9.112500001229033586, -4.330127018922190985, -2.500000000000001332 ) ) ;
#63263 = CARTESIAN_POINT ( 'NONE',  ( 4.912500001229034297, 0.000000000000000000, 4.999999999999998224 ) ) ;
#63264 = DIRECTION ( 'NONE',  ( -1.000000000000000000, -0.000000000000000000, -0.000000000000000000 ) ) ;
#63265 = CARTESIAN_POINT ( 'NONE',  ( 26.10000000122903430, -2.886751345948129988, 4.999999999999997335 ) ) ;
#63266 = CARTESIAN_POINT ( 'NONE',  ( 3.756430356249998770, 13.61562499938548498, 32.16877607737302469 ) ) ;
#63267 = CARTESIAN_POINT ( 'NONE',  ( 17.15625000122903288, -4.330127018922190985, -2.500000000000001332 ) ) ;
#63268 = CARTESIAN_POINT ( 'NONE',  ( 9.796875000614519990, -3.027376345333610441, -5.243569643749999898 ) ) ;
#63269 = CARTESIAN_POINT ( 'NONE',  ( 17.84999999999999787, 0.000000000000000000, 4.999999999999998224 ) ) ;
#63270 = CARTESIAN_POINT ( 'NONE',  ( 16.94062500061451715, -3.027376345333610441, -5.243569643749999898 ) ) ;
#63271 = CARTESIAN_POINT ( 'NONE',  ( 11.33437500061451608, 4.541064518000418104, 2.621784821874999949 ) ) ;
#63272 = CARTESIAN_POINT ( 'NONE',  ( 3.253125000614518036, 0.000000000000000000, 5.243569643749999010 ) ) ;
#63273 = CARTESIAN_POINT ( 'NONE',  ( 19.09687500061451360, -3.027376345333614438, 5.243569643749998122 ) ) ;
#63274 = CARTESIAN_POINT ( 'NONE',  ( 7.846875000614518036, -3.027376345333614438, 5.243569643749998122 ) ) ;
#63275 = CARTESIAN_POINT ( 'NONE',  ( 3.515625000614516882, 3.027376345333613106, -5.243569643749998122 ) ) ;
#63276 = LINE ( 'NONE', #14485, #43891 ) ;
#63277 = CARTESIAN_POINT ( 'NONE',  ( 7.115625000614516082, 3.027376345333613106, -5.243569643749998122 ) ) ;
#63278 = CARTESIAN_POINT ( 'NONE',  ( 17.80312500061451786, -4.541064518000417216, -2.621784821875001281 ) ) ;
#63279 = VERTEX_POINT ( 'NONE', #10296 ) ;
#63280 = CARTESIAN_POINT ( 'NONE',  ( 6.375000001229031987, -5.773502691896255534, -1.060575238724906372E-15 ) ) ;
#63281 = CARTESIAN_POINT ( 'NONE',  ( 14.01562500061451644, 3.027376345333611329, 5.243569643749999010 ) ) ;
#63282 = CARTESIAN_POINT ( 'NONE',  ( 12.17812500061451608, 4.541064518000418104, 2.621784821874999949 ) ) ;
#63283 = CARTESIAN_POINT ( 'NONE',  ( 24.42187500061451999, 2.746126346562643317, 4.756430356249998326 ) ) ;
#63284 = CARTESIAN_POINT ( 'NONE',  ( 12.67499999999999893, 6.123233995736764310E-16, -4.999999999999998224 ) ) ;
#63285 = CARTESIAN_POINT ( 'NONE',  ( 5.625000001229036428, 2.886751345948129099, -4.999999999999998224 ) ) ;
#63286 = CARTESIAN_POINT ( 'NONE',  ( 29.32499999999999929, 6.123233995736764310E-16, -4.999999999999998224 ) ) ;
#63287 = CARTESIAN_POINT ( 'NONE',  ( 18.11250000122903359, -4.330127018922190985, -2.500000000000001332 ) ) ;
#63288 = CARTESIAN_POINT ( 'NONE',  ( 24.26249999999999929, -5.773502691896255534, -1.060575238724906372E-15 ) ) ;
#63289 = CARTESIAN_POINT ( 'NONE',  ( 4.243569643749999898, 11.53437500061451892, -30.00000000000000000 ) ) ;
#63290 = CARTESIAN_POINT ( 'NONE',  ( -1.071796769724491671, 13.08259618943233704, 26.00000000000000355 ) ) ;
#63291 = FACE_OUTER_BOUND ( 'NONE', #35592, .T. ) ;
#63292 =( BOUNDED_CURVE ( )  B_SPLINE_CURVE ( 2, ( #27732, #1114, #749, #23621, #17704, #40265, #62786, #12178, #34706 ),
 .UNSPECIFIED., .F., .F. ) 
 B_SPLINE_CURVE_WITH_KNOTS ( ( 3, 2, 2, 2, 3 ),
 ( 0.5760869565217391353, 0.5797101449275362528, 0.5869565217391304879, 0.5942028985507246119, 0.5978260869565217295 ),
 .UNSPECIFIED. ) 
 CURVE ( )  GEOMETRIC_REPRESENTATION_ITEM ( )  RATIONAL_B_SPLINE_CURVE ( ( 0.9330127018922194093, 0.9330127018922194093, 1.000000000000000000, 0.8660254037844387076, 1.000000000000000000, 0.8660254037844387076, 1.000000000000000000, 0.9330127018922194093, 0.9330127018922194093 ) ) 
 REPRESENTATION_ITEM ( '' )  );
#63293 = CARTESIAN_POINT ( 'NONE',  ( 6.562500000000002665, 2.886751345948126879, 4.999999999999998224 ) ) ;
#63294 = CARTESIAN_POINT ( 'NONE',  ( 24.88125000122903074, 6.123233995736764310E-16, -4.999999999999998224 ) ) ;
#63295 = CARTESIAN_POINT ( 'NONE',  ( 18.49687500061452283, 6.054752690667223547, 3.707466751127219781E-16 ) ) ;
#63296 = CARTESIAN_POINT ( 'NONE',  ( -2.000000000000000000, 16.43750000122903643, 26.53589838486224650 ) ) ;
#63297 = CARTESIAN_POINT ( 'NONE',  ( 14.20312500061451644, -4.541064518000417216, -2.621784821875001281 ) ) ;
#63298 = CARTESIAN_POINT ( 'NONE',  ( 10.14375000122903536, 5.773502691896255534, 3.535250795749688894E-16 ) ) ;
#63299 = DIRECTION ( 'NONE',  ( -0.000000000000000000, -1.000000000000000000, -0.000000000000000000 ) ) ;
#63300 = CARTESIAN_POINT ( 'NONE',  ( 25.88437500061451502, -4.541064518000419881, 2.621784821874995952 ) ) ;
#63301 = CARTESIAN_POINT ( 'NONE',  ( 18.00937500061451502, 2.746126346562643317, 4.756430356249998326 ) ) ;
#63302 = CARTESIAN_POINT ( 'NONE',  ( 13.04062500061451502, 6.054752690667223547, 3.707466751127219781E-16 ) ) ;
#63303 = CARTESIAN_POINT ( 'NONE',  ( 15.27187500061451786, 3.027376345333613106, -5.243569643749998122 ) ) ;
#63304 = ORIENTED_EDGE ( 'NONE', *, *, #34144, .F. ) ;
#63305 = AXIS2_PLACEMENT_3D ( 'NONE', #67569, #33931, #56116 ) ;
#63306 = CARTESIAN_POINT ( 'NONE',  ( 26.80312500061451431, -4.541064518000417216, -2.621784821875001281 ) ) ;
#63307 = CARTESIAN_POINT ( 'NONE',  ( 21.25312500061451715, 0.000000000000000000, 5.243569643749999010 ) ) ;
#63308 = CARTESIAN_POINT ( 'NONE',  ( 29.12812500061451715, 6.421520780324663323E-16, -5.243569643749999010 ) ) ;
#63309 = CARTESIAN_POINT ( 'NONE',  ( 4.000000000000000000, 12.65000000122903323, -27.69059892324149885 ) ) ;
#63310 = CARTESIAN_POINT ( 'NONE',  ( 9.112500000000000711, 2.886751345948129099, -4.999999999999998224 ) ) ;
#63311 = CARTESIAN_POINT ( 'NONE',  ( 18.93750000122903288, -4.330127018922194537, 2.499999999999995559 ) ) ;
#63312 = CARTESIAN_POINT ( 'NONE',  ( 45.00000000000000000, 0.000000000000000000, 0.000000000000000000 ) ) ;
#63313 = CARTESIAN_POINT ( 'NONE',  ( 11.55937500061451573, 2.746126346562645981, -4.756430356249997438 ) ) ;
#63314 = EDGE_LOOP ( 'NONE', ( #12928, #51200, #59446, #67547 ) ) ;
#63315 = CARTESIAN_POINT ( 'NONE',  ( 17.51249999999999929, -5.773502691896255534, -1.060575238724906372E-15 ) ) ;
#63316 = CARTESIAN_POINT ( 'NONE',  ( 20.73750000000000071, -2.886751345948125991, -5.000000000000000000 ) ) ;
#63317 = CARTESIAN_POINT ( 'NONE',  ( 18.34687500061451715, -3.027376345333610441, -5.243569643749999898 ) ) ;
#63318 = CARTESIAN_POINT ( 'NONE',  ( 25.15312500061451217, 4.541064518000418104, -2.621784821874998173 ) ) ;
#63319 =( BOUNDED_CURVE ( )  B_SPLINE_CURVE ( 2, ( #64877, #37901, #20163, #14998, #20903, #65238, #70427 ),
 .UNSPECIFIED., .F., .F. ) 
 B_SPLINE_CURVE_WITH_KNOTS ( ( 3, 2, 2, 3 ),
 ( 0.6300000000000000044, 0.6333333333333333037, 0.6366666666666668251, 0.6400000000000001243 ),
 .UNSPECIFIED. ) 
 CURVE ( )  GEOMETRIC_REPRESENTATION_ITEM ( )  RATIONAL_B_SPLINE_CURVE ( ( 1.000000000000000000, 0.8660254037844387076, 1.000000000000000000, 0.8660254037844387076, 1.000000000000000000, 0.8660254037844342667, 1.000000000000004441 ) ) 
 REPRESENTATION_ITEM ( '' )  );
#63320 = ORIENTED_EDGE ( 'NONE', *, *, #7307, .F. ) ;
#63321 = EDGE_CURVE ( 'NONE', #12255, #18095, #32827, .T. ) ;
#63322 = CARTESIAN_POINT ( 'NONE',  ( 27.90000000122903145, -2.886751345948137981, 4.999999999999982236 ) ) ;
#63323 = CARTESIAN_POINT ( 'NONE',  ( 6.965625000614518392, -6.054752690667223547, -1.112240025338166033E-15 ) ) ;
#63324 = CARTESIAN_POINT ( 'NONE',  ( 30.00000000000000000, 0.000000000000000000, 0.000000000000000000 ) ) ;
#63325 = AXIS2_PLACEMENT_3D ( 'NONE', #64201, #57928, #35765 ) ;
#63326 = CARTESIAN_POINT ( 'NONE',  ( 14.36249999999999893, -5.773502691896255534, -1.060575238724906372E-15 ) ) ;
#63327 = CARTESIAN_POINT ( 'NONE',  ( -2.121784821874999949, 17.92812500061451786, 26.32496088578401938 ) ) ;
#63328 = CARTESIAN_POINT ( 'NONE',  ( 28.19062500061451715, -3.027376345333610441, -5.243569643749999898 ) ) ;
#63329 = CARTESIAN_POINT ( 'NONE',  ( 10.83750000000000036, -2.886751345948125991, -5.000000000000000000 ) ) ;
#63330 = CARTESIAN_POINT ( 'NONE',  ( 1.878215178124997609, 17.51562499938548356, 33.25316411605952993 ) ) ;
#63331 = CARTESIAN_POINT ( 'NONE',  ( 25.39687500061451431, -3.027376345333614438, 5.243569643749998122 ) ) ;
#63332 = EDGE_LOOP ( 'NONE', ( #11678, #13331, #21336, #5567 ) ) ;
#63333 = CARTESIAN_POINT ( 'NONE',  ( 21.32812500061451644, -4.541064518000419881, 2.621784821874995952 ) ) ;
#63334 = CARTESIAN_POINT ( 'NONE',  ( 22.50937500061451857, 4.541064518000418104, -2.621784821874998173 ) ) ;
#63335 = CARTESIAN_POINT ( 'NONE',  ( 9.001249775931846008E-16, 15.86562500061459247, -25.09994784771203058 ) ) ;
#63336 = CARTESIAN_POINT ( 'NONE',  ( 10.23750000000000071, -2.886751345948129988, 4.999999999999997335 ) ) ;
#63337 = EDGE_CURVE ( 'NONE', #55474, #38159, #22911, .T. ) ;
#63338 = CARTESIAN_POINT ( 'NONE',  ( 7.115625000614516082, 3.027376345333613106, -5.243569643749998122 ) ) ;
#63339 = CARTESIAN_POINT ( 'NONE',  ( 29.63437500061451502, 5.824947211148865298E-16, -4.756430356249998326 ) ) ;
#63340 = CARTESIAN_POINT ( 'NONE',  ( 22.90312500061451573, 4.541064518000418104, -2.621784821874998173 ) ) ;
#63341 = CARTESIAN_POINT ( 'NONE',  ( 27.60937500061450933, -5.492252693125287522, -1.008910452111647106E-15 ) ) ;
#63342 = CARTESIAN_POINT ( 'NONE',  ( 12.75937500061451857, 0.000000000000000000, 4.756430356249998326 ) ) ;
#63343 = CARTESIAN_POINT ( 'NONE',  ( 16.32187500061451502, 3.027376345333611329, 5.243569643749999010 ) ) ;
#63344 = CARTESIAN_POINT ( 'NONE',  ( 20.33437500061451786, 4.541064518000418104, 2.621784821874999949 ) ) ;
#63345 = CARTESIAN_POINT ( 'NONE',  ( 28.05937500061451573, 0.000000000000000000, 5.243569643749999010 ) ) ;
#63346 = CARTESIAN_POINT ( 'NONE',  ( -3.000416591977282496E-16, 15.69687500061451857, 25.09994784771203058 ) ) ;
#63347 = CARTESIAN_POINT ( 'NONE',  ( 8.653125000614515727, 0.000000000000000000, 5.243569643749999010 ) ) ;
#63348 = CARTESIAN_POINT ( 'NONE',  ( 1.071796769724491893, 10.34509619066136921, -26.00000000000000355 ) ) ;
#63349 = EDGE_CURVE ( 'NONE', #26800, #34969, #22460, .T. ) ;
#63350 = CARTESIAN_POINT ( 'NONE',  ( 3.984375000614517326, 6.421520780324663323E-16, -5.243569643749999010 ) ) ;
#63351 = CARTESIAN_POINT ( 'NONE',  ( 30.00000000000000000, 0.000000000000000000, 0.000000000000000000 ) ) ;
#63352 =( BOUNDED_CURVE ( )  B_SPLINE_CURVE ( 2, ( #38513, #32965, #56232, #39610, #4540, #10073, #61401 ),
 .UNSPECIFIED., .F., .F. ) 
 B_SPLINE_CURVE_WITH_KNOTS ( ( 3, 2, 2, 3 ),
 ( 0.5499999999999999334, 0.5533333333333332327, 0.5566666666666666430, 0.5600000000000000533 ),
 .UNSPECIFIED. ) 
 CURVE ( )  GEOMETRIC_REPRESENTATION_ITEM ( )  RATIONAL_B_SPLINE_CURVE ( ( 1.000000000000004441, 0.8660254037844342667, 1.000000000000000000, 0.8660254037844387076, 1.000000000000000000, 0.8660254037844387076, 1.000000000000000000 ) ) 
 REPRESENTATION_ITEM ( '' )  );
#63353 = CARTESIAN_POINT ( 'NONE',  ( 5.765625000614519102, 3.027376345333613106, -5.243569643749998122 ) ) ;
#63354 = CARTESIAN_POINT ( 'NONE',  ( 10.02187500061451964, 3.027376345333611329, 5.243569643749999010 ) ) ;
#63355 = SURFACE_SIDE_STYLE ('',( #51915 ) ) ;
#63356 = CARTESIAN_POINT ( 'NONE',  ( 15.78750000122903430, -4.330127018922194537, 2.499999999999995559 ) ) ;
#63357 = CARTESIAN_POINT ( 'NONE',  ( 5.034375000614519813, 4.541064518000418104, 2.621784821874999949 ) ) ;
#63358 = CARTESIAN_POINT ( 'NONE',  ( 7.078125000614516438, 6.421520780324663323E-16, -5.243569643749999010 ) ) ;
#63359 = CARTESIAN_POINT ( 'NONE',  ( -1.999999999999999112, 13.04374999877096641, 26.53589838486224650 ) ) ;
#63360 = CARTESIAN_POINT ( 'NONE',  ( 23.30625000122903145, 0.000000000000000000, 4.999999999999998224 ) ) ;
#63361 = CARTESIAN_POINT ( 'NONE',  ( 16.17187500061451644, 3.027376345333613106, -5.243569643749998122 ) ) ;
#63362 = CARTESIAN_POINT ( 'NONE',  ( 22.68750000000000000, 5.773502691896255534, 3.535250795749688401E-16 ) ) ;
#63363 = ORIENTED_EDGE ( 'NONE', *, *, #40617, .F. ) ;
#63364 = CARTESIAN_POINT ( 'NONE',  ( 24.29062500061451502, 6.054752690667223547, 3.707466751127219781E-16 ) ) ;
#63365 = CARTESIAN_POINT ( 'NONE',  ( 9.815625000614518925, 3.027376345333613106, -5.243569643749998122 ) ) ;
#63366 = CARTESIAN_POINT ( 'NONE',  ( 27.19687500061451857, -3.027376345333614438, 5.243569643749998122 ) ) ;
#63367 = CARTESIAN_POINT ( 'NONE',  ( 9.178125000614517859, -4.541064518000419881, 2.621784821874995952 ) ) ;
#63368 = CARTESIAN_POINT ( 'NONE',  ( -2.121784821874999949, 10.33437500061451786, -33.67503911421598417 ) ) ;
#63369 = EDGE_CURVE ( 'NONE', #25850, #68026, #30479, .T. ) ;
#63370 = CARTESIAN_POINT ( 'NONE',  ( 11.58750000122903501, 4.330127018922191873, 2.499999999999999556 ) ) ;
#63371 = CARTESIAN_POINT ( 'NONE',  ( 25.37812500061451715, -4.541064518000419881, 2.621784821874995952 ) ) ;
#63372 = CARTESIAN_POINT ( 'NONE',  ( -4.243569643749997233, 13.54062500061451679, -27.54997392385601174 ) ) ;
#63373 = CARTESIAN_POINT ( 'NONE',  ( 11.88750000122903216, 6.123233995736764310E-16, -4.999999999999998224 ) ) ;
#63374 = CARTESIAN_POINT ( 'NONE',  ( 23.01562500061451644, 3.027376345333611329, 5.243569643749999010 ) ) ;
#63375 = CARTESIAN_POINT ( 'NONE',  ( 11.62500000000000000, -4.330127018922194537, 2.499999999999995559 ) ) ;
#63376 = CARTESIAN_POINT ( 'NONE',  ( 20.57812500061451644, 6.421520780324663323E-16, -5.243569643749999010 ) ) ;
#63377 = CARTESIAN_POINT ( 'NONE',  ( 5.896875000614517859, 6.054752690667223547, 3.707466751127219781E-16 ) ) ;
#63378 = CARTESIAN_POINT ( 'NONE',  ( 19.38749999999999929, -2.886751345948125991, -5.000000000000000000 ) ) ;
#63379 = CARTESIAN_POINT ( 'NONE',  ( 15.07500000122903394, 2.886751345948129099, -4.999999999999998224 ) ) ;
#63380 = CARTESIAN_POINT ( 'NONE',  ( 13.64062500061451644, -3.027376345333614438, 5.243569643749998122 ) ) ;
#63381 = CARTESIAN_POINT ( 'NONE',  ( 16.94062500061451715, -3.027376345333610441, -5.243569643749999898 ) ) ;
#63382 = CARTESIAN_POINT ( 'NONE',  ( 25.42500000122903359, 2.886751345948129099, -4.999999999999998224 ) ) ;
#63383 = CARTESIAN_POINT ( 'NONE',  ( 19.46249999999999858, 2.886751345948129099, -4.999999999999998224 ) ) ;
#63384 = CARTESIAN_POINT ( 'NONE',  ( 23.70937500061451786, -4.541064518000417216, -2.621784821875001281 ) ) ;
#63385 = DIRECTION ( 'NONE',  ( -1.000000000000000000, -0.000000000000000000, -0.000000000000000000 ) ) ;
#63386 = CARTESIAN_POINT ( 'NONE',  ( 11.17500000122903536, 2.886751345948126879, 4.999999999999999112 ) ) ;
#63387 = CARTESIAN_POINT ( 'NONE',  ( 9.796875000614519990, -3.027376345333610441, -5.243569643749999898 ) ) ;
#63388 = CARTESIAN_POINT ( 'NONE',  ( 24.53437500061451715, -4.541064518000419881, 2.621784821874995952 ) ) ;
#63389 = CARTESIAN_POINT ( 'NONE',  ( 15.45000000122903216, -2.886751345948126435, -5.000000000000000000 ) ) ;
#63390 = CARTESIAN_POINT ( 'NONE',  ( 20.50312500061451715, -4.541064518000417216, -2.621784821875001281 ) ) ;
#63391 = CARTESIAN_POINT ( 'NONE',  ( 27.68437500061451573, -4.541064518000419881, 2.621784821874995952 ) ) ;
#63392 = CARTESIAN_POINT ( 'NONE',  ( -3.756430356250000102, 16.57812499938548356, 30.00000000000000000 ) ) ;
#63393 = CARTESIAN_POINT ( 'NONE',  ( 6.684375000614518392, 6.421520780324663323E-16, -5.243569643749999010 ) ) ;
#63394 = CARTESIAN_POINT ( 'NONE',  ( 19.11562500061451431, -6.054752690667223547, -1.112240025338166033E-15 ) ) ;
#63395 = ORIENTED_EDGE ( 'NONE', *, *, #35455, .F. ) ;
#63396 = CARTESIAN_POINT ( 'NONE',  ( 11.40000000000000036, 4.330127018922192761, -2.499999999999997780 ) ) ;
#63397 = CARTESIAN_POINT ( 'NONE',  ( 27.14062500061451644, -3.027376345333614438, 5.243569643749998122 ) ) ;
#63398 = CARTESIAN_POINT ( 'NONE',  ( 4.246875000614519280, -3.027376345333614438, 5.243569643749998122 ) ) ;
#63399 = LINE ( 'NONE', #1360, #50190 ) ;
#63400 = FACE_OUTER_BOUND ( 'NONE', #45879, .T. ) ;
#63401 = CARTESIAN_POINT ( 'NONE',  ( 16.08749999999999503, -2.886751345948129988, 4.999999999999997335 ) ) ;
#63402 = CARTESIAN_POINT ( 'NONE',  ( 21.74062500061451431, -3.027376345333614438, 5.243569643749998122 ) ) ;
#63403 = ORIENTED_EDGE ( 'NONE', *, *, #7149, .T. ) ;
#63404 = CARTESIAN_POINT ( 'NONE',  ( 24.18750000000000355, -2.886751345948129988, 4.999999999999997335 ) ) ;
#63405 = CARTESIAN_POINT ( 'NONE',  ( 27.23437500061451644, -4.541064518000419881, 2.621784821874995952 ) ) ;
#63406 = ORIENTED_EDGE ( 'NONE', *, *, #17177, .T. ) ;
#63407 = CARTESIAN_POINT ( 'NONE',  ( 14.57812500061451644, -4.541064518000419881, 2.621784821874995952 ) ) ;
#63408 = CARTESIAN_POINT ( 'NONE',  ( 5.128125000614516260, -4.541064518000419881, 2.621784821874995952 ) ) ;
#63409 = CARTESIAN_POINT ( 'NONE',  ( 18.23437500061451644, -2.746126346562642428, -4.756430356249999214 ) ) ;
#63410 = CARTESIAN_POINT ( 'NONE',  ( 29.61562500061451431, 3.027376345333613106, -5.243569643749998122 ) ) ;
#63411 = CARTESIAN_POINT ( 'NONE',  ( 14.21250000122903323, 4.330127018922192761, -2.499999999999997780 ) ) ;
#63412 = CARTESIAN_POINT ( 'NONE',  ( 21.07499999999999929, -4.330127018922194537, 2.499999999999995559 ) ) ;
#63413 = CARTESIAN_POINT ( 'NONE',  ( 29.36250000000000071, 2.886751345948129099, -4.999999999999998224 ) ) ;
#63414 = CARTESIAN_POINT ( 'NONE',  ( 4.434375000614519280, 6.421520780324663323E-16, -5.243569643749999010 ) ) ;
#63415 = CARTESIAN_POINT ( 'NONE',  ( 10.28437500061451715, 6.421520780324663323E-16, -5.243569643749999010 ) ) ;
#63416 = CARTESIAN_POINT ( 'NONE',  ( 19.99687500061451573, -3.027376345333614438, 5.243569643749998122 ) ) ;
#63417 = CARTESIAN_POINT ( 'NONE',  ( 9.900000001229033231, -2.886751345948130876, 4.999999999999996447 ) ) ;
#63418 = EDGE_LOOP ( 'NONE', ( #10813, #70972, #57549, #70153 ) ) ;
#63419 = CARTESIAN_POINT ( 'NONE',  ( 29.76562500061451644, 3.027376345333611329, 5.243569643749999010 ) ) ;
#63420 = CARTESIAN_POINT ( 'NONE',  ( 4.012500000000001954, -5.773502691896255534, -1.060575238724906372E-15 ) ) ;
#63421 = CARTESIAN_POINT ( 'NONE',  ( 5.671875000614519102, -6.054752690667223547, -1.112240025338166033E-15 ) ) ;
#63422 = CARTESIAN_POINT ( 'NONE',  ( 19.57500000000000284, 4.330127018922191873, 2.499999999999999556 ) ) ;
#63423 = CARTESIAN_POINT ( 'NONE',  ( 13.07812500061451821, 4.541064518000418104, 2.621784821874999949 ) ) ;
#63424 = CARTESIAN_POINT ( 'NONE',  ( 0.6945846161026939525, 20.50052346155192851, 33.93923243933046763 ) ) ;
#63425 = CARTESIAN_POINT ( 'NONE',  ( 45.00000000000000000, 4.500000000000000888, -5.500000000000000888 ) ) ;
#63426 = CARTESIAN_POINT ( 'NONE',  ( 11.23125000122903216, -4.330127018922194537, 2.499999999999995559 ) ) ;
#63427 = CARTESIAN_POINT ( 'NONE',  ( 20.78437500061451715, 4.119189519843966529, 2.378215178124999607 ) ) ;
#63428 = CARTESIAN_POINT ( 'NONE',  ( 7.790625000614518569, -3.027376345333614438, 5.243569643749998122 ) ) ;
#63429 = CARTESIAN_POINT ( 'NONE',  ( 23.97187500061451360, 3.027376345333611329, 5.243569643749999010 ) ) ;
#63430 = CARTESIAN_POINT ( 'NONE',  ( -3.000416591977282496E-16, 18.39687500061451786, 25.09994784771203058 ) ) ;
#63431 = CARTESIAN_POINT ( 'NONE',  ( 26.10937500061451644, 4.541064518000418104, -2.621784821874998173 ) ) ;
#63432 = CARTESIAN_POINT ( 'NONE',  ( 6.600000000000001421, 0.000000000000000000, 4.999999999999998224 ) ) ;
#63433 = CARTESIAN_POINT ( 'NONE',  ( 8.484601909799253346E-16, 13.92500000122903359, 34.61880215351700230 ) ) ;
#63434 = CARTESIAN_POINT ( 'NONE',  ( 14.27812500061451573, 6.421520780324663323E-16, -5.243569643749999010 ) ) ;
#63435 = CARTESIAN_POINT ( 'NONE',  ( 7.950000001229033053, 5.773502691896255534, 3.535250795749688894E-16 ) ) ;
#63436 = EDGE_CURVE ( 'NONE', #70720, #32936, #6931, .T. ) ;
#63437 = CARTESIAN_POINT ( 'NONE',  ( 17.18437500061451573, 4.541064518000418104, 2.621784821874999949 ) ) ;
#63438 = CARTESIAN_POINT ( 'NONE',  ( 12.49687500061451573, -3.027376345333610441, -5.243569643749999898 ) ) ;
#63439 = CARTESIAN_POINT ( 'NONE',  ( -3.942095835588579789, 3.076014195111399285, -29.30861973919568086 ) ) ;
#63440 = ORIENTED_EDGE ( 'NONE', *, *, #65759, .F. ) ;
#63441 = CARTESIAN_POINT ( 'NONE',  ( 11.99062500061451608, -3.027376345333610441, -5.243569643749999898 ) ) ;
#63442 = CARTESIAN_POINT ( 'NONE',  ( 13.87500000000000178, -4.330127018922194537, 2.499999999999995559 ) ) ;
#63443 = CARTESIAN_POINT ( 'NONE',  ( 23.96250000122903145, -4.330127018922190985, -2.500000000000001332 ) ) ;
#63444 = CARTESIAN_POINT ( 'NONE',  ( 13.47187500061451537, 3.027376345333613106, -5.243569643749998122 ) ) ;
#63445 = CARTESIAN_POINT ( 'NONE',  ( 3.390184931900214860, 3.675138926287994767, 3.390184931900133147 ) ) ;
#63446 = CARTESIAN_POINT ( 'NONE',  ( 14.99062500061451786, -3.027376345333614438, 5.243569643749998122 ) ) ;
#63447 = FACE_OUTER_BOUND ( 'NONE', #12711, .T. ) ;
#63448 = CARTESIAN_POINT ( 'NONE',  ( 24.27187500061452141, 3.027376345333613106, -5.243569643749998122 ) ) ;
#63449 = DIRECTION ( 'NONE',  ( -0.000000000000000000, -1.000000000000000000, -0.000000000000000000 ) ) ;
#63450 = CARTESIAN_POINT ( 'NONE',  ( 12.26250000122903394, -4.330127018922190985, -2.500000000000001332 ) ) ;
#63451 = CARTESIAN_POINT ( 'NONE',  ( 23.88749999999999929, -2.886751345948159742, -4.999999999999942268 ) ) ;
#63452 = CARTESIAN_POINT ( 'NONE',  ( 14.73749999999999893, -2.886751345948074920, 5.000000000000092371 ) ) ;
#63453 = CARTESIAN_POINT ( 'NONE',  ( 4.243569643749999898, 16.89687500061451786, -27.54997392385601529 ) ) ;
#63454 = CARTESIAN_POINT ( 'NONE',  ( 18.94687500061451502, 6.054752690667223547, 3.707466751127219781E-16 ) ) ;
#63455 = CARTESIAN_POINT ( 'NONE',  ( 18.75000000122903288, 5.773502691896255534, 3.535250795749688894E-16 ) ) ;
#63456 = CARTESIAN_POINT ( 'NONE',  ( 15.04687500061451644, -3.027376345333614438, 5.243569643749998122 ) ) ;
#63457 = DIRECTION ( 'NONE',  ( -1.000000000000000000, -0.000000000000000000, -0.000000000000000000 ) ) ;
#63458 = CARTESIAN_POINT ( 'NONE',  ( 20.96250000122903145, 4.330127018922192761, -2.499999999999997780 ) ) ;
#63459 = CARTESIAN_POINT ( 'NONE',  ( 15.55312500061451608, -4.541064518000417216, -2.621784821875001281 ) ) ;
#63460 = ORIENTED_EDGE ( 'NONE', *, *, #39769, .T. ) ;
#63461 = ORIENTED_EDGE ( 'NONE', *, *, #6614, .T. ) ;
#63462 = CARTESIAN_POINT ( 'NONE',  ( 17.88749999999999929, -2.886751345948129988, 4.999999999999997335 ) ) ;
#63463 = CARTESIAN_POINT ( 'NONE',  ( 4.000000000000000000, 15.63124999877096499, 27.69059892324149885 ) ) ;
#63464 = CARTESIAN_POINT ( 'NONE',  ( 24.82499999999999929, 6.123233995736764310E-16, -4.999999999999998224 ) ) ;
#63465 = CARTESIAN_POINT ( 'NONE',  ( 14.88750000122903394, -4.330127018922194537, 2.499999999999995559 ) ) ;
#63466 = CARTESIAN_POINT ( 'NONE',  ( 26.63437500061451857, 4.541064518000418104, 2.621784821874999949 ) ) ;
#63467 = CARTESIAN_POINT ( 'NONE',  ( 19.30312500061451786, 4.541064518000418104, -2.621784821874998173 ) ) ;
#63468 = CARTESIAN_POINT ( 'NONE',  ( 22.97812500061451857, 4.541064518000418104, 2.621784821874999949 ) ) ;
#63469 = CARTESIAN_POINT ( 'NONE',  ( 3.853125000614517681, -4.541064518000417216, -2.621784821875001281 ) ) ;
#63470 = CARTESIAN_POINT ( 'NONE',  ( 26.36249999999999716, 2.886751345948126879, 4.999999999999999112 ) ) ;
#63471 = CARTESIAN_POINT ( 'NONE',  ( 27.95625000122903359, -4.330127018922190985, -2.500000000000001332 ) ) ;
#63472 = CARTESIAN_POINT ( 'NONE',  ( 8.634375000614518569, 4.119189519843966529, 2.378215178124999607 ) ) ;
#63473 = DIRECTION ( 'NONE',  ( -1.000000000000000000, -0.000000000000000000, -0.000000000000000000 ) ) ;
#63474 = CARTESIAN_POINT ( 'NONE',  ( 3.965005778268202441, -3.046175387583509586, -4.212983158363885039 ) ) ;
#63475 = CARTESIAN_POINT ( 'NONE',  ( -3.000416591977282496E-16, 16.14687500061451431, -34.90005215228797653 ) ) ;
#63476 = CARTESIAN_POINT ( 'NONE',  ( 4.950000001229033941, -2.886751345948129988, 4.999999999999997335 ) ) ;
#63477 = CARTESIAN_POINT ( 'NONE',  ( 7.087499999999999467, -2.886751345948129988, 4.999999999999997335 ) ) ;
#63478 =( BOUNDED_CURVE ( )  B_SPLINE_CURVE ( 2, ( #37502, #31962, #70391, #42682, #3164, #49329, #9793, #48228, #14964 ),
 .UNSPECIFIED., .F., .F. ) 
 B_SPLINE_CURVE_WITH_KNOTS ( ( 3, 2, 2, 2, 3 ),
 ( 0.8152173913043478937, 0.8188405797101449002, 0.8260869565217391353, 0.8333333333333333703, 0.8369565217391304879 ),
 .UNSPECIFIED. ) 
 CURVE ( )  GEOMETRIC_REPRESENTATION_ITEM ( )  RATIONAL_B_SPLINE_CURVE ( ( 0.9330127018922192983, 0.9330127018922202975, 1.000000000000000000, 0.8660254037844387076, 1.000000000000000000, 0.8660254037844387076, 1.000000000000000000, 0.9330127018922182991, 0.9330127018922192983 ) ) 
 REPRESENTATION_ITEM ( '' )  );
#63479 = EDGE_CURVE ( 'NONE', #47310, #67390, #57005, .T. ) ;
#63480 = CARTESIAN_POINT ( 'NONE',  ( 9.721875000614517148, -6.054752690667223547, -1.112240025338166033E-15 ) ) ;
#63481 = CARTESIAN_POINT ( 'NONE',  ( 27.74062500061451431, -3.027376345333610441, -5.243569643749999898 ) ) ;
#63482 = CARTESIAN_POINT ( 'NONE',  ( 27.48750000122903359, -4.330127018922194537, 2.499999999999995559 ) ) ;
#63483 = CARTESIAN_POINT ( 'NONE',  ( 24.39375000122903359, -2.886751345948126435, -5.000000000000000000 ) ) ;
#63484 = CARTESIAN_POINT ( 'NONE',  ( 7.809375000614519280, 0.000000000000000000, 5.243569643749999010 ) ) ;
#63485 = CARTESIAN_POINT ( 'NONE',  ( 11.93437500061451573, -4.541064518000419881, 2.621784821874995952 ) ) ;
#63486 = CARTESIAN_POINT ( 'NONE',  ( 7.200000000000001954, -4.330127018922190985, -2.500000000000001332 ) ) ;
#63487 = CARTESIAN_POINT ( 'NONE',  ( -4.243569643749999898, 15.30312500061459424, 30.00000000000000000 ) ) ;
#63488 = CARTESIAN_POINT ( 'NONE',  ( 4.000109024101403676, 24.99997092690864520, 30.26059014310604312 ) ) ;
#63489 = CARTESIAN_POINT ( 'NONE',  ( 6.262500000000000178, -5.773502691896255534, -1.060575238724906372E-15 ) ) ;
#63490 = CARTESIAN_POINT ( 'NONE',  ( 26.70000000122903572, -2.886751345948125991, -5.000000000000000000 ) ) ;
#63491 = CARTESIAN_POINT ( 'NONE',  ( 18.42187500061451644, 4.119189519843966529, 2.378215178124999607 ) ) ;
#63492 = CARTESIAN_POINT ( 'NONE',  ( 22.41562500061451502, 3.027376345333613106, -5.243569643749998122 ) ) ;
#63493 = CARTESIAN_POINT ( 'NONE',  ( 13.00312500061451537, 4.541064518000418104, -2.621784821874998173 ) ) ;
#63494 = CARTESIAN_POINT ( 'NONE',  ( 25.54687500061451644, 4.119189519843966529, -2.378215178124998275 ) ) ;
#63495 = CARTESIAN_POINT ( 'NONE',  ( 8.746875000614515727, -3.027376345333614438, 5.243569643749998122 ) ) ;
#63496 = CARTESIAN_POINT ( 'NONE',  ( 26.55000000000000071, -4.330127018922190985, -2.500000000000001332 ) ) ;
#63497 = CARTESIAN_POINT ( 'NONE',  ( 21.45000000122903216, 5.773502691896255534, 3.535250795749688894E-16 ) ) ;
#63498 = CARTESIAN_POINT ( 'NONE',  ( 1.626862140677534273E-15, 12.46250000000000213, -26.00000000000000355 ) ) ;
#63499 = CARTESIAN_POINT ( 'NONE',  ( 11.89687500061451608, -3.027376345333614438, 5.243569643749998122 ) ) ;
#63500 = CARTESIAN_POINT ( 'NONE',  ( 26.63437500061451857, 4.541064518000418104, 2.621784821874999949 ) ) ;
#63501 = EDGE_CURVE ( 'NONE', #45031, #19466, #5840, .T. ) ;
#63502 = CARTESIAN_POINT ( 'NONE',  ( 3.309375000614518836, 0.000000000000000000, 5.243569643749999010 ) ) ;
#63503 = CARTESIAN_POINT ( 'NONE',  ( 1.626862140677534273E-15, 13.47500000122903252, -26.00000000000000355 ) ) ;
#63504 = CARTESIAN_POINT ( 'NONE',  ( 23.10937500061451644, 0.000000000000000000, 5.243569643749999010 ) ) ;
#63505 = CARTESIAN_POINT ( 'NONE',  ( 11.97187500061451892, -6.054752690667223547, -1.112240025338166033E-15 ) ) ;
#63506 = CARTESIAN_POINT ( 'NONE',  ( -1.878215178124999163, 19.20312499938548356, 26.74683588394047007 ) ) ;
#63507 = CARTESIAN_POINT ( 'NONE',  ( 24.78750000000000497, -2.886751345948125991, -5.000000000000000000 ) ) ;
#63508 = CARTESIAN_POINT ( 'NONE',  ( -2.000000000000001776, 13.70000000000000107, 33.46410161513775705 ) ) ;
#63509 = CARTESIAN_POINT ( 'NONE',  ( 9.001249775931846008E-16, 14.12187500061451750, -25.09994784771203058 ) ) ;
#63510 = CARTESIAN_POINT ( 'NONE',  ( 26.44687500061451502, -2.746126346562642428, -4.756430356249999214 ) ) ;
#63511 = CARTESIAN_POINT ( 'NONE',  ( 17.05312500061451786, 4.541064518000418104, -2.621784821874998173 ) ) ;
#63512 = CARTESIAN_POINT ( 'NONE',  ( 7.275000000000000355, 6.123233995736764310E-16, -4.999999999999998224 ) ) ;
#63513 = CARTESIAN_POINT ( 'NONE',  ( 19.42499999999999716, 6.123233995736764310E-16, -4.999999999999998224 ) ) ;
#63514 = CARTESIAN_POINT ( 'NONE',  ( 14.62500000000000000, 4.330127018922191873, 2.499999999999999556 ) ) ;
#63515 = CARTESIAN_POINT ( 'NONE',  ( -3.000416591977282496E-16, 11.59062500061451750, 25.09994784771203058 ) ) ;
#63516 = CARTESIAN_POINT ( 'NONE',  ( 13.72500000122903074, 2.886751345948129099, -4.999999999999998224 ) ) ;
#63517 = CARTESIAN_POINT ( 'NONE',  ( 25.05937500061451573, -4.541064518000417216, -2.621784821875001281 ) ) ;
#63518 = ORIENTED_EDGE ( 'NONE', *, *, #30034, .T. ) ;
#63519 = CARTESIAN_POINT ( 'NONE',  ( 20.46562500061451928, -6.054752690667223547, -1.112240025338166033E-15 ) ) ;
#63520 = CARTESIAN_POINT ( 'NONE',  ( 20.67187500061451289, 3.027376345333613106, -5.243569643749998122 ) ) ;
#63521 = CARTESIAN_POINT ( 'NONE',  ( 5.062500000000000888, 2.886751345948129099, -4.999999999999998224 ) ) ;
#63522 = CARTESIAN_POINT ( 'NONE',  ( 8.165625000614516793, 3.027376345333611329, 5.243569643749999010 ) ) ;
#63523 = CARTESIAN_POINT ( 'NONE',  ( 22.67812500061451431, -4.541064518000419881, 2.621784821874995952 ) ) ;
#63524 = CARTESIAN_POINT ( 'NONE',  ( 12.12187500061451573, 3.027376345333613106, -5.243569643749998122 ) ) ;
#63525 = CARTESIAN_POINT ( 'NONE',  ( 16.17187500061451644, 3.027376345333613106, -5.243569643749998122 ) ) ;
#63526 = CARTESIAN_POINT ( 'NONE',  ( -4.243569643749999898, 15.75312500061451537, 30.00000000000000000 ) ) ;
#63527 = CARTESIAN_POINT ( 'NONE',  ( 18.78750000122903430, 4.330127018922191873, 2.499999999999999556 ) ) ;
#63528 = CARTESIAN_POINT ( 'NONE',  ( 11.44687500061451679, -2.746126346562646425, 4.756430356249996549 ) ) ;
#63529 = CARTESIAN_POINT ( 'NONE',  ( 8.578125000614518214, 4.541064518000418104, 2.621784821874999949 ) ) ;
#63530 = CARTESIAN_POINT ( 'NONE',  ( 3.571875000614517237, 3.027376345333613106, -5.243569643749998122 ) ) ;
#63531 = CARTESIAN_POINT ( 'NONE',  ( 29.12812500061451715, 6.421520780324663323E-16, -5.243569643749999010 ) ) ;
#63532 = CARTESIAN_POINT ( 'NONE',  ( 25.13437500061451502, 6.421520780324663323E-16, -5.243569643749999010 ) ) ;
#63533 = CARTESIAN_POINT ( 'NONE',  ( 17.99062500061451786, 6.054752690667223547, 3.707466751127219781E-16 ) ) ;
#63534 = CARTESIAN_POINT ( 'NONE',  ( 24.82500000122902861, -5.773502691896255534, -1.060575238724906372E-15 ) ) ;
#63535 =( BOUNDED_CURVE ( )  B_SPLINE_CURVE ( 2, ( #45160, #102, #28173, #18504, #11535, #1183, #29607, #6351, #62496 ),
 .UNSPECIFIED., .F., .F. ) 
 B_SPLINE_CURVE_WITH_KNOTS ( ( 3, 2, 2, 2, 3 ),
 ( 0.3472222222222222654, 0.3518518518518518601, 0.3611111111111111049, 0.3703703703703703498, 0.3750000000000000000 ),
 .UNSPECIFIED. ) 
 CURVE ( )  GEOMETRIC_REPRESENTATION_ITEM ( )  RATIONAL_B_SPLINE_CURVE ( ( 0.9330127018922194093, 0.9330127018922197424, 1.000000000000000000, 0.8660254037844387076, 1.000000000000000000, 0.8660254037844387076, 1.000000000000000000, 0.9330127018922194093, 0.9330127018922194093 ) ) 
 REPRESENTATION_ITEM ( '' )  );
#63536 = CARTESIAN_POINT ( 'NONE',  ( 25.26562500061451289, 3.027376345333611329, 5.243569643749999010 ) ) ;
#63537 = CARTESIAN_POINT ( 'NONE',  ( 21.45937500061451786, -4.541064518000417216, -2.621784821875001281 ) ) ;
#63538 = CARTESIAN_POINT ( 'NONE',  ( 16.41562500061451857, -6.054752690667223547, -1.112240025338166033E-15 ) ) ;
#63539 = CARTESIAN_POINT ( 'NONE',  ( -4.243569643749997233, 17.19687500061451502, 32.45002607614398471 ) ) ;
#63540 = CARTESIAN_POINT ( 'NONE',  ( 22.30312500061451431, -4.541064518000417216, -2.621784821875001281 ) ) ;
#63541 = CARTESIAN_POINT ( 'NONE',  ( 22.05000000000000071, -4.330127018922190985, -2.500000000000001332 ) ) ;
#63542 = ORIENTED_EDGE ( 'NONE', *, *, #17977, .T. ) ;
#63543 = CARTESIAN_POINT ( 'NONE',  ( 25.98750000000000071, -2.886751345948129988, 4.999999999999997335 ) ) ;
#63544 = CARTESIAN_POINT ( 'NONE',  ( -2.828200636599751609E-16, 12.23750000000000249, -34.61880215351700230 ) ) ;
#63545 = CARTESIAN_POINT ( 'NONE',  ( -3.756430356250001434, 20.66562499938548569, 32.16877607737301048 ) ) ;
#63546 = CARTESIAN_POINT ( 'NONE',  ( 29.27812500061451573, 4.541064518000418104, 2.621784821874999949 ) ) ;
#63547 = CARTESIAN_POINT ( 'NONE',  ( 9.290625000614515017, -3.027376345333610441, -5.243569643749999898 ) ) ;
#63548 = CARTESIAN_POINT ( 'NONE',  ( 21.52500000122903145, 2.886751345948126879, 4.999999999999999112 ) ) ;
#63549 = CARTESIAN_POINT ( 'NONE',  ( 26.50312500061451360, 4.541064518000418104, -2.621784821874998173 ) ) ;
#63550 = CARTESIAN_POINT ( 'NONE',  ( 25.27499999999999858, 6.123233995736764310E-16, -4.999999999999998224 ) ) ;
#63551 = CARTESIAN_POINT ( 'NONE',  ( 8.484601909799253346E-16, 15.27500000122903501, -25.38119784648299770 ) ) ;
#63552 = CARTESIAN_POINT ( 'NONE',  ( 25.35000000122903074, -2.886751345948159742, -4.999999999999942268 ) ) ;
#63553 = CARTESIAN_POINT ( 'NONE',  ( 10.56562500061451715, -6.054752690667223547, -1.112240025338166033E-15 ) ) ;
#63554 = ORIENTED_EDGE ( 'NONE', *, *, #74, .T. ) ;
#63555 = CARTESIAN_POINT ( 'NONE',  ( 25.07812500061451644, 6.421520780324663323E-16, -5.243569643749999010 ) ) ;
#63556 = CARTESIAN_POINT ( 'NONE',  ( 7.940625000614518036, -3.027376345333610441, -5.243569643749999898 ) ) ;
#63557 = CARTESIAN_POINT ( 'NONE',  ( 2.840625000614518392, -3.027376345333614438, 5.243569643749998122 ) ) ;
#63558 = CARTESIAN_POINT ( 'NONE',  ( 15.23437500061451644, 5.824947211148865298E-16, -4.756430356249998326 ) ) ;
#63559 = CARTESIAN_POINT ( 'NONE',  ( 4.683223236373093457, -1.751405183929441556, 4.942428804804532838 ) ) ;
#63560 = CARTESIAN_POINT ( 'NONE',  ( 13.64999999999999858, 4.330127018922192761, -2.499999999999997780 ) ) ;
#63561 = CARTESIAN_POINT ( 'NONE',  ( 14.82187500061451679, 3.027376345333613106, -5.243569643749998122 ) ) ;
#63562 = CARTESIAN_POINT ( 'NONE',  ( 12.03750000122903430, 4.330127018922191873, 2.499999999999999556 ) ) ;
#63563 = CARTESIAN_POINT ( 'NONE',  ( 17.74687500061451928, -3.027376345333614438, 5.243569643749998122 ) ) ;
#63564 = CARTESIAN_POINT ( 'NONE',  ( 17.96250000000000213, -5.773502691896255534, -1.060575238724906372E-15 ) ) ;
#63565 = CARTESIAN_POINT ( 'NONE',  ( 7.509375000614517681, -4.541064518000417216, -2.621784821875001281 ) ) ;
#63566 = CARTESIAN_POINT ( 'NONE',  ( -3.000416591977282496E-16, 10.69062500061451715, -34.90005215228797653 ) ) ;
#63567 = DIRECTION ( 'NONE',  ( 0.000000000000000000, 0.000000000000000000, 1.000000000000000000 ) ) ;
#63568 = CARTESIAN_POINT ( 'NONE',  ( 23.82187500061451502, 4.119189519843966529, 2.378215178124999607 ) ) ;
#63569 = ORIENTED_EDGE ( 'NONE', *, *, #16122, .T. ) ;
#63570 = CARTESIAN_POINT ( 'NONE',  ( 23.95312500061451289, 0.000000000000000000, 5.243569643749999010 ) ) ;
#63571 = CARTESIAN_POINT ( 'NONE',  ( 11.25000000000000000, -4.330127018922190985, -2.500000000000001332 ) ) ;
#63572 = CARTESIAN_POINT ( 'NONE',  ( 27.53437500061451360, 4.541064518000418104, 2.621784821874999949 ) ) ;
#63573 = ADVANCED_FACE ( 'NONE', ( #57883 ), #62351, .T. ) ;
#63574 = CARTESIAN_POINT ( 'NONE',  ( 23.40000000000000213, -4.330127018922190985, -2.500000000000001332 ) ) ;
#63575 = CARTESIAN_POINT ( 'NONE',  ( 7.828125000614517326, -4.541064518000419881, 2.621784821874995952 ) ) ;
#63576 = CARTESIAN_POINT ( 'NONE',  ( 25.32187500061451502, -4.119189519843968306, 2.378215178124996054 ) ) ;
#63577 = CARTESIAN_POINT ( 'NONE',  ( 17.10937500061451999, 4.541064518000418104, -2.621784821874998173 ) ) ;
#63578 = CARTESIAN_POINT ( 'NONE',  ( 12.04687500061451821, 4.119189519843966529, -2.378215178124998275 ) ) ;
#63579 = CARTESIAN_POINT ( 'NONE',  ( 29.58750000122903501, 4.330127018922191873, 2.499999999999999556 ) ) ;
#63580 = CARTESIAN_POINT ( 'NONE',  ( 9.196875000614518569, -3.027376345333614438, 5.243569643749998122 ) ) ;
#63581 = VERTEX_POINT ( 'NONE', #46456 ) ;
#63582 = CARTESIAN_POINT ( 'NONE',  ( 19.80937500061451573, 4.541064518000418104, -2.621784821874998173 ) ) ;
#63583 = DIRECTION ( 'NONE',  ( -0.000000000000000000, -1.000000000000000000, -0.000000000000000000 ) ) ;
#63584 = CARTESIAN_POINT ( 'NONE',  ( 27.71250000000000568, 2.886751345948126879, 4.999999999999999112 ) ) ;
#63585 = CARTESIAN_POINT ( 'NONE',  ( 28.50937500061451502, 0.000000000000000000, 5.243569643749999010 ) ) ;
#63586 = CARTESIAN_POINT ( 'NONE',  ( 19.42499999999999716, 6.123233995736764310E-16, -4.999999999999998224 ) ) ;
#63587 = CARTESIAN_POINT ( 'NONE',  ( 3.310802318797580579, -3.746810377620464205, 3.668301323911666412 ) ) ;
#63588 = ORIENTED_EDGE ( 'NONE', *, *, #48710, .T. ) ;
#63589 = CARTESIAN_POINT ( 'NONE',  ( 10.12500000000000178, 4.330127018922191873, 2.499999999999999556 ) ) ;
#63590 = CARTESIAN_POINT ( 'NONE',  ( 11.03437500061451360, -2.746126346562642428, -4.756430356249999214 ) ) ;
#63591 = CARTESIAN_POINT ( 'NONE',  ( 23.46562500061451573, 3.027376345333611329, 5.243569643749999010 ) ) ;
#63592 = CARTESIAN_POINT ( 'NONE',  ( 15.22500000000000142, -4.330127018922194537, 2.499999999999995559 ) ) ;
#63593 = CARTESIAN_POINT ( 'NONE',  ( 8.775000001229033231, 2.886751345948129099, -4.999999999999998224 ) ) ;
#63594 = CARTESIAN_POINT ( 'NONE',  ( 7.603125000614517681, 4.541064518000418104, -2.621784821874998173 ) ) ;
#63595 = CARTESIAN_POINT ( 'NONE',  ( 22.34999999999999787, 0.000000000000000000, 4.999999999999998224 ) ) ;
#63596 = CARTESIAN_POINT ( 'NONE',  ( 21.06562500061451715, 3.027376345333613106, -5.243569643749998122 ) ) ;
#63597 = CARTESIAN_POINT ( 'NONE',  ( 24.82500000122902861, -5.773502691896255534, -1.060575238724906372E-15 ) ) ;
#63598 = CARTESIAN_POINT ( 'NONE',  ( 3.756430356250000102, 18.04062499938548214, 30.00000000000000000 ) ) ;
#63599 = CARTESIAN_POINT ( 'NONE',  ( 4.387500000000002842, -2.886751345948129988, 4.999999999999997335 ) ) ;
#63600 = ORIENTED_EDGE ( 'NONE', *, *, #19527, .T. ) ;
#63601 = CARTESIAN_POINT ( 'NONE',  ( 22.34062500061451573, -3.027376345333610441, -5.243569643749999898 ) ) ;
#63602 = CARTESIAN_POINT ( 'NONE',  ( 27.17812500061451786, -4.541064518000419881, 2.621784821874995952 ) ) ;
#63603 = CARTESIAN_POINT ( 'NONE',  ( 28.17187500061451644, -6.054752690667223547, -1.112240025338166033E-15 ) ) ;
#63604 = CARTESIAN_POINT ( 'NONE',  ( 15.02812500061451750, -4.541064518000419881, 2.621784821874995952 ) ) ;
#63605 = CARTESIAN_POINT ( 'NONE',  ( 4.844509297411972781, 1.237226603047926421, -5.095516945469514170 ) ) ;
#63606 = CARTESIAN_POINT ( 'NONE',  ( 26.70000000122903572, -2.886751345948125991, -5.000000000000000000 ) ) ;
#63607 = CARTESIAN_POINT ( 'NONE',  ( 22.20937500061451431, 0.000000000000000000, 4.756430356249998326 ) ) ;
#63608 = CARTESIAN_POINT ( 'NONE',  ( 17.76562500061451644, -6.054752690667223547, -1.112240025338166033E-15 ) ) ;
#63609 = CARTESIAN_POINT ( 'NONE',  ( 3.525000001229034119, 2.886751345948126879, 4.999999999999999112 ) ) ;
#63610 = CARTESIAN_POINT ( 'NONE',  ( 10.73437500061451644, 6.421520780324663323E-16, -5.243569643749999010 ) ) ;
#63611 = CARTESIAN_POINT ( 'NONE',  ( 10.62187500061451928, -6.054752690667223547, -1.112240025338166033E-15 ) ) ;
#63612 = CARTESIAN_POINT ( 'NONE',  ( 18.90937500061451360, 4.541064518000418104, -2.621784821874998173 ) ) ;
#63613 = ORIENTED_EDGE ( 'NONE', *, *, #22395, .T. ) ;
#63614 = DIRECTION ( 'NONE',  ( 0.000000000000000000, 0.000000000000000000, 1.000000000000000000 ) ) ;
#63615 = CARTESIAN_POINT ( 'NONE',  ( 24.17812500061451786, 6.421520780324663323E-16, -5.243569643749999010 ) ) ;
#63616 = CARTESIAN_POINT ( 'NONE',  ( 19.88437500061451857, 4.541064518000418104, 2.621784821874999949 ) ) ;
#63617 = CARTESIAN_POINT ( 'NONE',  ( 23.57812500061451289, -4.541064518000419881, 2.621784821874995952 ) ) ;
#63618 = CARTESIAN_POINT ( 'NONE',  ( 8.962500000000002132, -5.773502691896255534, -1.060575238724906372E-15 ) ) ;
#63619 = CARTESIAN_POINT ( 'NONE',  ( -3.999999999999999556, 14.11249999999999893, 27.69059892324149530 ) ) ;
#63620 = CARTESIAN_POINT ( 'NONE',  ( 29.09062500061451573, -3.027376345333610441, -5.243569643749999898 ) ) ;
#63621 = CARTESIAN_POINT ( 'NONE',  ( 10.46250000122903323, -4.330127018922190985, -2.500000000000001332 ) ) ;
#63622 = CARTESIAN_POINT ( 'NONE',  ( 4.500000001229034652, -2.886751345948129988, 4.999999999999997335 ) ) ;
#63623 = CARTESIAN_POINT ( 'NONE',  ( 28.80000000122903359, -2.886751345948092240, 5.000000000000060396 ) ) ;
#63624 = CARTESIAN_POINT ( 'NONE',  ( 26.92500000122903359, 2.886751345948126879, 4.999999999999999112 ) ) ;
#63625 = CARTESIAN_POINT ( 'NONE',  ( -1.999999999999999112, 20.24374999877096570, 26.53589838486224650 ) ) ;
#63626 = CARTESIAN_POINT ( 'NONE',  ( 10.05937500061451750, 0.000000000000000000, 5.243569643749999010 ) ) ;
#63627 = CARTESIAN_POINT ( 'NONE',  ( 9.449999999999999289, -4.330127018922190985, -2.500000000000001332 ) ) ;
#63628 = EDGE_CURVE ( 'NONE', #50439, #45851, #12472, .T. ) ;
#63629 = CARTESIAN_POINT ( 'NONE',  ( 18.36562500061451431, 3.027376345333613106, -5.243569643749998122 ) ) ;
#63630 = CARTESIAN_POINT ( 'NONE',  ( 11.29687500061451644, 6.054752690667223547, 3.707466751127219781E-16 ) ) ;
#63631 = CARTESIAN_POINT ( 'NONE',  ( 2.840625000614518392, -3.027376345333614438, 5.243569643749998122 ) ) ;
#63632 = ADVANCED_FACE ( 'NONE', ( #11747 ), #40192, .T. ) ;
#63633 = CARTESIAN_POINT ( 'NONE',  ( 20.67187500061451289, 3.027376345333612662, -5.243569643749998122 ) ) ;
#63634 = CARTESIAN_POINT ( 'NONE',  ( 8.446875000614518569, -3.027376345333610441, -5.243569643749999898 ) ) ;
#63635 = CARTESIAN_POINT ( 'NONE',  ( 3.057638380960218338, -3.956115207028108038, -3.345374717763163641 ) ) ;
#63636 = CARTESIAN_POINT ( 'NONE',  ( 6.853125000614516793, 0.000000000000000000, 5.243569643749999010 ) ) ;
#63637 = CARTESIAN_POINT ( 'NONE',  ( 18.85312500061451502, 4.541064518000418104, -2.621784821874998173 ) ) ;
#63638 = ORIENTED_EDGE ( 'NONE', *, *, #26043, .T. ) ;
#63639 = CARTESIAN_POINT ( 'NONE',  ( 6.562500001229032875, 4.330127018922192761, -2.499999999999997780 ) ) ;
#63640 = CARTESIAN_POINT ( 'NONE',  ( 15.89062500061451289, -3.027376345333614438, 5.243569643749998122 ) ) ;
#63641 = CARTESIAN_POINT ( 'NONE',  ( 11.99062500061451608, -3.027376345333610441, -5.243569643749999898 ) ) ;
#63642 = CARTESIAN_POINT ( 'NONE',  ( 23.33437500061451786, 5.824947211148865298E-16, -4.756430356249998326 ) ) ;
#63643 = CARTESIAN_POINT ( 'NONE',  ( 14.51250000000000107, 2.886751345948129099, -4.999999999999998224 ) ) ;
#63644 = CARTESIAN_POINT ( 'NONE',  ( 6.937500001229033764, 6.123233995736764310E-16, -4.999999999999998224 ) ) ;
#63645 = CARTESIAN_POINT ( 'NONE',  ( 14.74687500061451573, -3.027376345333610441, -5.243569643749999898 ) ) ;
#63646 = CARTESIAN_POINT ( 'NONE',  ( 18.67500000122903714, 2.886751345948129099, -4.999999999999998224 ) ) ;
#63647 = CARTESIAN_POINT ( 'NONE',  ( 25.46249999999999858, 2.886751345948126879, 4.999999999999999112 ) ) ;
#63648 = CARTESIAN_POINT ( 'NONE',  ( -4.243569643749999898, 18.00312500061451715, -30.00000000000000000 ) ) ;
#63649 = CYLINDRICAL_SURFACE ( 'NONE', #37118, 4.000000000000000000 ) ;
#63650 = CARTESIAN_POINT ( 'NONE',  ( 4.378670304180260153, -3.762209243454259333, -3.970801729131952396 ) ) ;
#63651 = CARTESIAN_POINT ( 'NONE',  ( 3.442799801882779231, -3.625940455515339167, 3.602703790535031203 ) ) ;
#63652 = CARTESIAN_POINT ( 'NONE',  ( 22.57499999999999929, 6.123233995736764310E-16, -4.999999999999998224 ) ) ;
#63653 = CARTESIAN_POINT ( 'NONE',  ( 17.44687500061451857, -3.027376345333610441, -5.243569643749999898 ) ) ;
#63654 = CARTESIAN_POINT ( 'NONE',  ( 22.93125000122903145, -4.330127018922194537, 2.499999999999995559 ) ) ;
#63655 = CARTESIAN_POINT ( 'NONE',  ( 14.12812500061451715, -4.541064518000419881, 2.621784821874995952 ) ) ;
#63656 = CARTESIAN_POINT ( 'NONE',  ( 9.131250001229034297, 6.123233995736764310E-16, -4.999999999999998224 ) ) ;
#63657 = CARTESIAN_POINT ( 'NONE',  ( 15.90000000122903501, -2.886751345948193048, -4.999999999999883649 ) ) ;
#63658 = CARTESIAN_POINT ( 'NONE',  ( 27.30937500061451573, -4.541064518000417216, -2.621784821875001281 ) ) ;
#63659 = CARTESIAN_POINT ( 'NONE',  ( 18.45937500061451431, 2.746126346562643317, 4.756430356249998326 ) ) ;
#63660 = CARTESIAN_POINT ( 'NONE',  ( 10.60312500061451679, -4.541064518000417216, -2.621784821875001281 ) ) ;
#63661 = CARTESIAN_POINT ( 'NONE',  ( 15.60937500061451644, -4.541064518000417216, -2.621784821875001281 ) ) ;
#63662 = VERTEX_POINT ( 'NONE', #28372 ) ;
#63663 = AXIS2_PLACEMENT_3D ( 'NONE', #51505, #30044, #11975 ) ;
#63664 = CARTESIAN_POINT ( 'NONE',  ( 26.57812500061451644, 4.541064518000418104, 2.621784821874999949 ) ) ;
#63665 = CARTESIAN_POINT ( 'NONE',  ( 19.97812500061451502, -4.541064518000419881, 2.621784821874995952 ) ) ;
#63666 = CARTESIAN_POINT ( 'NONE',  ( 29.20312500061451644, 4.541064518000418104, -2.621784821874998173 ) ) ;
#63667 = CARTESIAN_POINT ( 'NONE',  ( -5.810221930991193690E-16, 14.15000000122903145, -34.00000000000000000 ) ) ;
#63668 = CARTESIAN_POINT ( 'NONE',  ( 9.562500000000001776, 2.886751345948129099, -4.999999999999998224 ) ) ;
#63669 = CARTESIAN_POINT ( 'NONE',  ( 18.67500000122903714, 2.886751345948129099, -4.999999999999998224 ) ) ;
#63670 = CARTESIAN_POINT ( 'NONE',  ( 23.21250000122903501, 4.330127018922192761, -2.499999999999997780 ) ) ;
#63671 = CARTESIAN_POINT ( 'NONE',  ( 9.421875000614514661, 4.119189519843966529, 2.378215178124999607 ) ) ;
#63672 = EDGE_LOOP ( 'NONE', ( #54932, #56352, #18972, #27115 ) ) ;
#63673 = CARTESIAN_POINT ( 'NONE',  ( 16.42500000000000071, 4.330127018922191873, 2.499999999999999556 ) ) ;
#63674 = CARTESIAN_POINT ( 'NONE',  ( 20.43749999999999645, 5.773502691896255534, 3.535250795749688894E-16 ) ) ;
#63675 = CARTESIAN_POINT ( 'NONE',  ( 18.12187500061451573, 3.027376345333611329, 5.243569643749999010 ) ) ;
#63676 = CARTESIAN_POINT ( 'NONE',  ( 13.22812500061451502, -4.541064518000419881, 2.621784821874995952 ) ) ;
#63677 = ORIENTED_EDGE ( 'NONE', *, *, #1559, .T. ) ;
#63678 = CARTESIAN_POINT ( 'NONE',  ( 28.05000000122903003, -2.886751345948130432, -4.999999999999991118 ) ) ;
#63679 = CARTESIAN_POINT ( 'NONE',  ( 4.865625000614517859, 3.027376345333613106, -5.243569643749998122 ) ) ;
#63680 = CARTESIAN_POINT ( 'NONE',  ( 2.000000000000001332, 15.31250000122903465, 33.46410161513774995 ) ) ;
#63681 = CARTESIAN_POINT ( 'NONE',  ( 12.78749999999999964, 5.773502691896255534, 3.535250795749688894E-16 ) ) ;
#63682 = CARTESIAN_POINT ( 'NONE',  ( 27.75937500061451502, 2.746126346562645981, -4.756430356249997438 ) ) ;
#63683 = CARTESIAN_POINT ( 'NONE',  ( -2.121784821874999949, 17.47812500061451502, 26.32496088578401938 ) ) ;
#63684 = CARTESIAN_POINT ( 'NONE',  ( 3.309375000614518836, 0.000000000000000000, 5.243569643749999010 ) ) ;
#63685 = CARTESIAN_POINT ( 'NONE',  ( 11.58750000000000036, -2.886751345948129988, 4.999999999999997335 ) ) ;
#63686 = CARTESIAN_POINT ( 'NONE',  ( -3.756430356250001434, 16.50312499938548783, 32.16877607737301048 ) ) ;
#63687 = CARTESIAN_POINT ( 'NONE',  ( 26.93437500061451573, 6.421520780324663323E-16, -5.243569643749999010 ) ) ;
#63688 = ORIENTED_EDGE ( 'NONE', *, *, #5826, .F. ) ;
#63689 = CARTESIAN_POINT ( 'NONE',  ( 21.51562500061451644, 3.027376345333613106, -5.243569643749998122 ) ) ;
#63690 = CARTESIAN_POINT ( 'NONE',  ( 24.04687500061451644, -3.027376345333614438, 5.243569643749998122 ) ) ;
#63691 = CARTESIAN_POINT ( 'NONE',  ( 2.121784821874999061, 15.60312500061459495, -33.67503911421598417 ) ) ;
#63692 = CARTESIAN_POINT ( 'NONE',  ( 6.515625000614516438, -6.054752690667223547, -1.112240025338166033E-15 ) ) ;
#63693 = CARTESIAN_POINT ( 'NONE',  ( 28.39687500061451431, 5.492252693125287522, 3.363034840372157021E-16 ) ) ;
#63694 = CARTESIAN_POINT ( 'NONE',  ( 23.31562500061451004, 3.027376345333612662, -5.243569643749998122 ) ) ;
#63695 = CARTESIAN_POINT ( 'NONE',  ( 27.45937500061451431, 2.746126346562643317, 4.756430356249998326 ) ) ;
#63696 = CARTESIAN_POINT ( 'NONE',  ( 9.796875000614519990, -2.746126346562642428, -4.756430356249999214 ) ) ;
#63697 = CARTESIAN_POINT ( 'NONE',  ( 16.13437500061451502, 6.421520780324663323E-16, -5.243569643749999010 ) ) ;
#63698 = CARTESIAN_POINT ( 'NONE',  ( 18.75937500061451857, -4.541064518000417216, -2.621784821875001281 ) ) ;
#63699 = CARTESIAN_POINT ( 'NONE',  ( 28.09687500061451360, -3.027376345333614438, 5.243569643749998122 ) ) ;
#63700 = CARTESIAN_POINT ( 'NONE',  ( 4.243569643749999898, 17.38437500061451502, 30.00000000000000000 ) ) ;
#63701 = CARTESIAN_POINT ( 'NONE',  ( 7.190625000614518036, 6.054752690667223547, 3.707466751127219781E-16 ) ) ;
#63702 = CARTESIAN_POINT ( 'NONE',  ( 4.000000000000000000, 16.13749999999999929, 32.30940107675849760 ) ) ;
#63703 = CARTESIAN_POINT ( 'NONE',  ( 5.521875000614517859, 3.027376345333611329, 5.243569643749999010 ) ) ;
#63704 = CARTESIAN_POINT ( 'NONE',  ( 6.328125000614515550, 4.541064518000418104, 2.621784821874999949 ) ) ;
#63705 = CARTESIAN_POINT ( 'NONE',  ( 9.909375000614517148, 4.541064518000418104, -2.621784821874998173 ) ) ;
#63706 = CARTESIAN_POINT ( 'NONE',  ( 16.53750000122903430, 4.330127018922191873, 2.499999999999999556 ) ) ;
#63707 = CARTESIAN_POINT ( 'NONE',  ( 5.296875000614518214, -3.027376345333610441, -5.243569643749999898 ) ) ;
#63708 = CARTESIAN_POINT ( 'NONE',  ( 7.265625000614516438, 3.027376345333611329, 5.243569643749999010 ) ) ;
#63709 = CARTESIAN_POINT ( 'NONE',  ( 4.000000000000000000, 14.73124999877096819, 27.69059892324149530 ) ) ;
#63710 = CARTESIAN_POINT ( 'NONE',  ( 23.56875000122902719, 2.886751345948129099, -4.999999999999998224 ) ) ;
#63711 = CARTESIAN_POINT ( 'NONE',  ( 16.43437500061451573, -4.541064518000419881, 2.621784821874995952 ) ) ;
#63712 = CARTESIAN_POINT ( 'NONE',  ( 27.59999999999999787, 4.330127018922192761, -2.499999999999997780 ) ) ;
#63713 = ORIENTED_EDGE ( 'NONE', *, *, #66296, .F. ) ;
#63714 = CARTESIAN_POINT ( 'NONE',  ( 24.51562500061451289, -6.054752690667223547, -1.112240025338166033E-15 ) ) ;
#63715 = CARTESIAN_POINT ( 'NONE',  ( 8.540625000614518569, 6.054752690667223547, 3.707466751127219781E-16 ) ) ;
#63716 = CARTESIAN_POINT ( 'NONE',  ( 27.60937500061451644, 0.000000000000000000, 5.243569643749999010 ) ) ;
#63717 = CARTESIAN_POINT ( 'NONE',  ( 11.12812500061451715, 6.421520780324663323E-16, -5.243569643749999010 ) ) ;
#63718 = CARTESIAN_POINT ( 'NONE',  ( -0.7368805616696195715, 9.859898480082234684, -34.17910162106521454 ) ) ;
#63719 = CARTESIAN_POINT ( 'NONE',  ( 11.10000000122903252, 5.773502691896255534, 3.535250795749688894E-16 ) ) ;
#63720 = CARTESIAN_POINT ( 'NONE',  ( 25.71562500061451573, 3.027376345333611329, 5.243569643749999010 ) ) ;
#63721 = CARTESIAN_POINT ( 'NONE',  ( -3.000416591977282496E-16, 12.49062500061451608, -34.90005215228797653 ) ) ;
#63722 = CARTESIAN_POINT ( 'NONE',  ( 12.22500000122903430, -5.773502691896255534, -1.060575238724906372E-15 ) ) ;
#63723 = CARTESIAN_POINT ( 'NONE',  ( 21.44062500061452070, -3.027376345333610441, -5.243569643749999898 ) ) ;
#63724 = CARTESIAN_POINT ( 'NONE',  ( 11.25000000000000000, -4.330127018922190985, -2.500000000000001332 ) ) ;
#63725 = CARTESIAN_POINT ( 'NONE',  ( 19.52812500061451573, -4.541064518000419881, 2.621784821874995952 ) ) ;
#63726 = CARTESIAN_POINT ( 'NONE',  ( 6.459375000614518747, 0.000000000000000000, 5.243569643749999010 ) ) ;
#63727 = CARTESIAN_POINT ( 'NONE',  ( 20.21250000000000213, -5.773502691896255534, -1.060575238724906372E-15 ) ) ;
#63728 = CARTESIAN_POINT ( 'NONE',  ( 13.83750000122903323, 4.330127018922191873, 2.499999999999999556 ) ) ;
#63729 =( BOUNDED_CURVE ( )  B_SPLINE_CURVE ( 2, ( #11014, #53072, #35351, #8372, #52349, #35714, #40544 ),
 .UNSPECIFIED., .F., .T. ) 
 B_SPLINE_CURVE_WITH_KNOTS ( ( 3, 2, 2, 3 ),
 ( 0.3666666666666666408, 0.3694444444444444642, 0.3722222222222222321, 0.3750000000000000000 ),
 .UNSPECIFIED. ) 
 CURVE ( )  GEOMETRIC_REPRESENTATION_ITEM ( )  RATIONAL_B_SPLINE_CURVE ( ( 1.000000000000000000, 0.8660254037844387076, 1.000000000000000000, 0.8660254037844387076, 1.000000000000000000, 0.8660254037844387076, 1.000000000000000000 ) ) 
 REPRESENTATION_ITEM ( '' )  );
#63730 = CARTESIAN_POINT ( 'NONE',  ( 10.86562500061451431, 3.027376345333611329, 5.243569643749999010 ) ) ;
#63731 = CARTESIAN_POINT ( 'NONE',  ( 12.85312500061451502, -4.541064518000417216, -2.621784821875001281 ) ) ;
#63732 = CARTESIAN_POINT ( 'NONE',  ( 24.60000000122903430, 5.773502691896255534, 3.535250795749688894E-16 ) ) ;
#63733 = CARTESIAN_POINT ( 'NONE',  ( 20.25937500061451857, 4.541064518000418104, -2.621784821874998173 ) ) ;
#63734 = CARTESIAN_POINT ( 'NONE',  ( 22.25625000122903074, 4.330127018922192761, -2.499999999999997780 ) ) ;
#63735 = EDGE_CURVE ( 'NONE', #47420, #33656, #30951, .T. ) ;
#63736 = CARTESIAN_POINT ( 'NONE',  ( 7.275000001229035007, -5.773502691896255534, -1.060575238724906372E-15 ) ) ;
#63737 = CARTESIAN_POINT ( 'NONE',  ( 9.196875000614518569, -3.027376345333614438, 5.243569643749998122 ) ) ;
#63738 = CARTESIAN_POINT ( 'NONE',  ( 25.17187500061451644, 3.027376345333613106, -5.243569643749998122 ) ) ;
#63739 = ADVANCED_FACE ( 'NONE', ( #70803 ), #58244, .T. ) ;
#63740 =( BOUNDED_CURVE ( )  B_SPLINE_CURVE ( 2, ( #72658, #43857, #55303, #61202, #21303, #72290, #21668 ),
 .UNSPECIFIED., .F., .F. ) 
 B_SPLINE_CURVE_WITH_KNOTS ( ( 3, 2, 2, 3 ),
 ( 0.8500000000000001998, 0.8533333333333336101, 0.8566666666666669094, 0.8600000000000002087 ),
 .UNSPECIFIED. ) 
 CURVE ( )  GEOMETRIC_REPRESENTATION_ITEM ( )  RATIONAL_B_SPLINE_CURVE ( ( 0.9999999999999911182, 0.8660254037844475894, 1.000000000000000000, 0.8660254037844387076, 1.000000000000000000, 0.8660254037844298258, 1.000000000000008882 ) ) 
 REPRESENTATION_ITEM ( '' )  );
#63741 = CARTESIAN_POINT ( 'NONE',  ( 23.77499999999999858, -4.330127018922194537, 2.499999999999995559 ) ) ;
#63742 = CARTESIAN_POINT ( 'NONE',  ( 20.95312500061451999, -4.541064518000417216, -2.621784821875001281 ) ) ;
#63743 = CARTESIAN_POINT ( 'NONE',  ( 27.53437500061451360, 4.541064518000418104, 2.621784821874999949 ) ) ;
#63744 = CARTESIAN_POINT ( 'NONE',  ( 3.756430356249998770, 18.11562499938548143, 32.16877607737301759 ) ) ;
#63745 = CARTESIAN_POINT ( 'NONE',  ( 19.18125000122903501, 4.330127018922191873, 2.499999999999999556 ) ) ;
#63746 = CARTESIAN_POINT ( 'NONE',  ( 8.971875000614515372, 3.027376345333613106, -5.243569643749998122 ) ) ;
#63747 = CARTESIAN_POINT ( 'NONE',  ( 18.25312500061451715, -4.541064518000417216, -2.621784821875001281 ) ) ;
#63748 = ORIENTED_EDGE ( 'NONE', *, *, #61508, .F. ) ;
#63749 = CARTESIAN_POINT ( 'NONE',  ( -3.999999999999999112, 12.76250000000000107, -32.30940107675850470 ) ) ;
#63750 = CARTESIAN_POINT ( 'NONE',  ( 26.76562500061451644, -6.054752690667223547, -1.112240025338166033E-15 ) ) ;
#63751 = CARTESIAN_POINT ( 'NONE',  ( 4.809375000614516615, -4.541064518000417216, -2.621784821875001281 ) ) ;
#63752 = CARTESIAN_POINT ( 'NONE',  ( 10.23750000122903359, 4.330127018922191873, 2.499999999999999556 ) ) ;
#63753 = CARTESIAN_POINT ( 'NONE',  ( 3.727827348360245097, 3.332161949968362347, -3.727827348360304605 ) ) ;
#63754 = CARTESIAN_POINT ( 'NONE',  ( 18.14999999999999858, 4.330127018922192761, -2.499999999999997780 ) ) ;
#63755 = CARTESIAN_POINT ( 'NONE',  ( 21.89062500061451289, -3.027376345333610441, -5.243569643749999898 ) ) ;
#63756 = ORIENTED_EDGE ( 'NONE', *, *, #1804, .T. ) ;
#63757 = CARTESIAN_POINT ( 'NONE',  ( 24.63749999999999574, -2.886751345948129988, 4.999999999999997335 ) ) ;
#63758 = CARTESIAN_POINT ( 'NONE',  ( 25.62187500061451573, 3.027376345333613106, -5.243569643749998122 ) ) ;
#63759 = ORIENTED_EDGE ( 'NONE', *, *, #7133, .T. ) ;
#63760 = CARTESIAN_POINT ( 'NONE',  ( 14.27812500061451573, 6.421520780324663323E-16, -5.243569643749999010 ) ) ;
#63761 = CARTESIAN_POINT ( 'NONE',  ( 5.278125000614516615, 6.421520780324663323E-16, -5.243569643749999010 ) ) ;
#63762 = CARTESIAN_POINT ( 'NONE',  ( 17.10937500061451644, 2.746126346562643317, 4.756430356249998326 ) ) ;
#63763 = CARTESIAN_POINT ( 'NONE',  ( 29.24062500061451431, 6.054752690667223547, 3.707466751127219781E-16 ) ) ;
#63764 =( BOUNDED_SURFACE ( )  B_SPLINE_SURFACE ( 1, 2, ( 
 ( #6688, #1153, #23662, #24020, #68747, #24387, #18830, #18105, #7046, #63186, #29575, #69828, #52112, #63908, #35832, #46569, #18473, #41037, #12938, #35475, #58355, #59455, #42849, #48032, #8136, #42119, #14029, #54661, #71659, #36569, #64645, #70924, #70185, #15126, #20294, #65741, #53938, #4065, #36206, #36935, #37303, #8862, #14397, #41746, #26590, #8494, #30662, #26222, #48762, #49131, #31769, #9232, #25859, #31398, #65371, #3335, #48398, #14759, #59826, #54305, #3697, #71285, #64275, #60186, #19564, #20664, #25110, #43222, #25485, #42486, #37663, #47653, #2957, #31026, #59089, #53195, #70557, #9595, #13663, #58724, #2591, #53561, #32127, #19933, #65009, #38773, #50939, #55754, #9958, #22490, #4787, #21032, #21759, #5148, #32495, #15851, #55029, #27684, #4433, #55393, #33573, #60922, #61645, #66850, #10324, #27321, #26961, #38397, #61293, #72379, #16579, #72019, #50221, #44320, #11047, #43585, #5870, #38029, #10685, #16222, #33215, #33935, #72747, #49488, #21395, #43951, #45039, #22132, #44688, #28402, #73108, #66474, #60551, #32858, #66106, #67218, #49853, #39131, #56121, #5513, #28052, #50580, #15485, #11418, #67574, #16939, #39494, #62016, #56478, #12135, #63100, #41310, #23210, #18024, #1429, #6602, #39867, #701, #45763, #13212, #30215, #68299, #17659, #29490, #28760, #46851, #52027, #24304, #12501, #35751, #67933, #68660, #69024, #40581, #46123, #335, #58272, #40220, #62379, #57911, #7320, #7679, #63468, #40953, #57557, #18386, #22845, #12855, #11778, #35388, #6960, #18746, #23936, #62742, #34294, #45397, #29851, #17307, #56826, #6232, #51665, #1069, #46485, #63820, #69391, #51300, #34660, #57189, #29132, #23578, #52387, #35029, #1794, #70471, #20207, #14669, #13574, #64186, #36847, #42033, #36119, #37212, #64921, #8407, #59734, #59363, #58639, #8047, #41664, #24663, #9142, #30581, #71196, #42761, #69741, #65281, #43127, #31308, #47209, #25027, #47569, #53107, #2504, #59001, #26131, #48308, #70832, #2869, #19475, #37576, #31679, #54213, #20570, #70099, #2152, #15039, #42398, #36483, #25399, #25770, #19109, #64557, #14311, #30936, #47942, #53477, #3610, #13946, #19848, #8774, #53848, #3242, #52748, #48671, #65650, #60100, #9509, #50133, #44605, #21675, #55310, #50497, #3978, #33486, #43496, #4704, #38689, #27601, #66764, #49771, #49404, #72665, #10964, #26501, #5427, #66022, #32041, #27234, #67493, #39048, #10603, #15766, #71571, #15401, #16137, #20945, #4348, #61208, #71935, #72296, #26874, #10240, #44232, #67135, #21311, #22044, #33131, #43865, #38306, #37943, #66389, #55668, #32773, #16492, #9871, #5065, #61562, #56035, #61931, #16856, #49043, #27966, #73024, #22408, #44955, #39412, #60462, #32404, #54943, #54574, #60835, #63012, #69298, #63381, #62299, #28320, #56745, #41222, #46038, #619, #29407, #23850, #11695, #34575, #68216, #11337, #1699, #62655, #40864, #35301, #23127, #50857, #45682, #982, #52298, #33854, #24211, #255, #57103, #6149, #68574, #28678, #6513, #51218, #12051, #23491, #51941, #46763, #6875, #22763, #1338, #17934, #29761, #12409, #17577, #45315, #56398, #46398, #5788, #67850, #17222, #29047, #51583, #57470, #18660, #57823, #39783, #40139, #34211, #40496, #34943, #68934, #18291, #12766, #7232, #31214, #25679, #24574, #2064, #47849, #53019, #47119, #48215, #2778, #19379, #70736, #70377, #69651, #19015, #52656, #35662, #20114, #41576, #9056, #53755, #7587, #3151, #54126, #42303, #58183, #36025, #58542, #64093, #13476, #70010, #37116, #59274, #8682, #13853, #30491, #7954, #30123, #41937, #25302, #20481, #71108, #2413, #24935, #19755, #47478, #64829, #8319, #63731, #14219, #64462, #65193, #36395, #13123, #58909, #36755, #30848, #53383, #42669, #14583, #59643, #31587, #3521, #26042, #48582, #71849, #15314, #32315, #3888, #43409, #43773, #4258, #27148, #48951, #60742, #26783, #72211, #67047, #21956, #37491, #66298, #49316, #21221, #50045, #15677, #31951, #26408, #71480, #10517, #38214, #32684, #44513, #61120, #20856, #60011, #65934, #43035, #10152, #60373, #21589, #66669, #37853, #55224, #54849, #65563, #72570, #4618, #33044, #4978, #9781, #54487, #49682, #44142, #14952, #16046, #38594, #55584, #27511, #9422, #36265, #8190, #48818, #65802, #30717, #58780, #65065, #64331, #9291, #14456, #59885, #48087, #71348, #30361, #31082, #31456, #53622, #8555, #35888, #20723, #2648, #24805, #20355, #42906, #43281, #25916, #3395, #19986, #3014, #59512, #25544, #70613, #42539, #58413, #54363, #13724, #53998, #19247, #48456, #19619, #36625, #8926, #41802, #70247, #25167, #42175, #7826, #59146, #36990, #47348, #53250, #69882, #70980, #47708, #64701, #65430, #14085, #14820, #37363, #31824, #3757, #26281, #52891, #2288, #11567, #22279, #56274, #27841, #16364, #33367, #38919, #39651, #66626, #60697, #50372, #16003, #67366, #38173, #10831, #22636, #4576, #44100, #5663, #50728, #72897, #61438, #56622, #10110, #62170, #49639, #55903, #44831, #33728, #16729, #5295, #55541, #28199, #17090, #32640, #34082, #72165, #55181, #39284, #483, #45186, #61797, #21916, #27106, #51087, #21545, #11201, #10473, #131, #4937, #67718, #33002, #6017, #28552, #22992, #45553, #68083, #38552, #61075, #27471, #50003, #72528, #44472, #67002, #48366, #59058, #62523, #51447, #17451, #69796, #19162, #64613, #36904, #42455, #28909, #13264, #34445, #6377, #30270, #13999, #69442, #2560, #36175, #8463, #53531, #850, #23358, #25080, #7735, #46903, #2927, #30631, #47262, #25456, #47623, #18799, #41363, #63873, #11920, #48000, #35802, #59424, #30998, #56973, #70528, #8832, #70156, #58324, #52803, #19903, #2204, #24719, #36538, #64978, #8103, #41716, #31368, #64243, #14369, #13631, #58692, #19533, #53909, #53163, #42091, #3302, #25829, #40009, #65340, #44294, #9200, #70892, #66077, #33190 ),
 ( #14730, #15455, #66448, #38000, #43555, #27657, #55729, #37633, #59794, #55368, #4761, #10660, #60894, #38369, #55000, #60522, #21368, #9928, #32467, #4406, #5123, #16195, #26190, #15825, #54273, #10299, #54630, #71630, #43922, #3667, #32098, #60156, #48730, #37272, #4037, #26935, #20265, #42817, #31735, #71253, #49460, #20633, #71994, #32830, #43191, #27294, #65711, #72352, #26561, #15097, #21003, #49828, #9566, #49101, #21733, #66822, #38746, #61266, #62716, #16912, #17635, #22820, #39467, #56453, #56096, #45013, #57534, #51640, #12110, #5843, #56800, #310, #40195, #6934, #35004, #67192, #17278, #50912, #28375, #63073, #45372, #61621, #68634, #67549, #72721, #12475, #39840, #33909, #61990, #23548, #34267, #68273, #62354, #67908, #11750, #6205, #1041, #5487, #22104, #28733, #28026, #51274, #50196, #678, #34633, #16553, #50554, #57162, #6575, #23184, #45738, #17996, #44662, #46098, #11024, #29105, #40555, #39105, #33546, #73082, #11390, #22463, #8383, #23911, #2844, #40929, #29465, #24639, #64897, #36461, #8021, #13187, #52001, #42375, #46459, #2128, #1765, #64159, #46827, #47185, #24279, #7653, #19085, #47545, #14287, #25003, #18358, #70074, #36094, #47918, #30557, #69364, #63443, #59339, #19449, #1402, #12829, #68997, #30192, #52721, #2478, #70447, #53454, #35363, #18722, #57887, #7296, #41286, #42009, #29826, #13547, #69717, #64529, #13923, #52361, #63797, #58614, #35726, #58248, #58976, #41640, #53083, #30913, #25373, #19823, #36824, #70808, #53825, #66366, #37188, #27212, #49382, #25747, #71913, #72275, #60439, #3218, #54190, #3587, #14647, #59712, #15016, #55288, #4325, #26850, #32016, #48648, #66741, #21287, #38281, #54552, #15742, #48284, #9119, #43840, #60809, #71548, #3954, #49747, #20183, #10217, #42738, #26477, #15379, #32750, #43474, #49017, #26109, #4682, #21652, #65257, #44209, #31656, #8750, #20922, #16111, #38663, #9849, #65629, #31283, #71173, #20545, #65998, #43103, #37921, #37554, #32378, #60076, #9487, #54918, #6123, #958, #56721, #50110, #28654, #67825, #6486, #62276, #27941, #72639, #17908, #51193, #33108, #22022, #61186, #39388, #61907, #34187, #29021, #12025, #44579, #56011, #5042, #67111, #73000, #596, #39026, #45291, #5767, #23101, #45658, #16467, #61540, #17198, #50474, #10942, #68191, #233, #16834, #17554, #39759, #33464, #5404, #22384, #55646, #40115, #44933, #51557, #62631, #27578, #34550, #23467, #11670, #67471, #11312, #33833, #56375, #28298, #50833, #57078, #46013, #68550, #22741, #10581, #25275, #58518, #69986, #58885, #57798, #62986, #2755, #30098, #24184, #7207, #13830, #24550, #7928, #52633, #18634, #35636, #41198, #41913, #68907, #12381, #2039, #18265, #69628, #40471, #30466, #30825, #18990, #34917, #12740, #35276, #46373, #40838, #46738, #36369, #35999, #52995, #63706, #29736, #47822, #2391, #19356, #8295, #52273, #57444, #70352, #47096, #69272, #1675, #53358, #41552, #24910, #64069, #13098, #58158, #7562, #64438, #63356, #6848, #13451, #47453, #29382, #51916, #1313, #23822, #59250, #25653, #37828, #32291, #9397, #43011, #38190, #64803, #21196, #31189, #65540, #26385, #15289, #54464, #37467, #37093, #60348, #71825, #14193, #66273, #53731, #19729, #14927, #55200, #26760, #71456, #3499, #42279, #32659, #36728, #59987, #65169, #3862, #59618, #31927, #14560, #71083, #48926, #9757, #4593, #54825, #8658, #4233, #20832, #60716, #43385, #9032, #3124, #49657, #49292, #48189, #70713, #20088, #20457, #65909, #43748, #10127, #15651, #42645, #31562, #54101, #26018, #48557, #27123, #50021, #56289, #16745, #39667, #34100, #33020, #10492, #5679, #61455, #55558, #56639, #11219, #27857, #6035, #28215, #4954, #27487, #61094, #44118, #28569, #72545, #17467, #62186, #16022, #38570, #44847, #44489, #33744, #16382, #67383, #67022, #50388, #61815, #17107, #11937, #67735, #21933, #11583, #50744, #40027, #147, #38937, #10849, #28928, #51105, #66645, #33383, #72185, #72913, #22295, #45202, #62540, #23011, #55919, #5314, #39301, #22653, #502, #45570, #68101, #34462, #56990, #6397, #21564, #12292, #62897, #35549, #40746, #34826, #35907, #63621, #7119, #13365, #58068, #57354, #6759, #40378, #23375, #58431, #29293, #69899, #18903, #68455, #41464, #41819, #30005, #45923, #23732, #46281, #51823, #1226, #57714, #24821, #47009, #69544, #1588, #18178, #36283, #63983, #7842, #19265, #68821, #868, #13741, #41111, #35189, #63262, #47368, #7478, #30379, #13011, #29648, #46645, #52186, #52908, #12654, #17817, #52547, #24098, #1954, #51465, #69186, #2306, #18546, #24461, #64350, #58797, #8207, #54015, #49205, #2666, #32205, #42193, #3411, #37378, #26297, #65446, #48471, #48103, #48834, #9672, #25183, #4141, #64717, #30736, #25931, #66184, #37738, #9307, #14472, #53268, #43662, #59529, #65818, #14837, #14101, #36641, #19636, #47726, #15200, #59163, #71739, #71365, #70265, #20739, #21109, #31841, #8571, #3031, #25562, #31099, #53639, #37006, #26672, #43297, #60258, #70995, #70626, #15562, #54739, #38105, #60627, #20001, #42554, #65081, #20371, #8941, #31472, #42922, #59902, #54377, #3772, #61368, #5223, #10765, #11493, #38480, #32572, #72827, #61004, #39215, #10038, #55836, #67651, #49570, #15931, #28130, #22568, #22210, #33298, #28479, #55110, #34015, #21476, #27765, #16657, #5593, #44764, #50305, #27401, #50658, #62099, #4510, #56552, #44029, #27039, #67299, #45479, #17017, #61727, #66930, #72092, #22921, #66551, #11128, #55473, #33655, #49931, #56200, #4865, #62, #45116, #39576, #68011, #5946, #10403, #51016, #412, #17383, #39941, #72456, #32935, #21841, #44404, #16299, #38853, #62454, #40655, #63176, #35462, #7755, #13284, #779, #57265, #6309, #51377, #1140, #57984, #40293, #46558, #7034, #29922, #24375, #23288, #45836, #69100, #51741, #68373, #46923 ) ),
 .UNSPECIFIED., .F., .F., .F. ) 
 B_SPLINE_SURFACE_WITH_KNOTS ( ( 2, 2 ),
 ( 3, 2, 2, 2, 2, 2, 2, 2, 2, 2, 2, 2, 2, 2, 2, 2, 2, 2, 2, 2, 2, 2, 2, 2, 2, 2, 2, 2, 2, 2, 2, 2, 2, 2, 2, 2, 2, 2, 2, 2, 2, 2, 2, 2, 2, 2, 2, 2, 2, 2, 2, 2, 2, 2, 2, 2, 2, 2, 2, 2, 2, 2, 2, 2, 2, 2, 2, 2, 2, 2, 2, 2, 2, 2, 2, 2, 2, 2, 2, 2, 2, 2, 2, 2, 2, 2, 2, 2, 2, 2, 2, 2, 2, 2, 2, 2, 2, 2, 2, 2, 2, 2, 2, 2, 2, 2, 2, 2, 2, 2, 2, 2, 2, 2, 2, 2, 2, 2, 2, 2, 2, 2, 2, 2, 2, 2, 2, 2, 2, 2, 2, 2, 2, 2, 2, 2, 2, 2, 2, 2, 2, 2, 2, 2, 2, 2, 2, 2, 2, 2, 2, 2, 2, 2, 2, 2, 2, 2, 2, 2, 2, 2, 2, 2, 2, 2, 2, 2, 2, 2, 2, 2, 2, 2, 2, 2, 2, 2, 2, 2, 2, 2, 2, 2, 2, 2, 2, 2, 2, 2, 2, 2, 2, 2, 2, 2, 2, 2, 2, 2, 2, 2, 2, 2, 2, 2, 2, 2, 2, 2, 2, 2, 2, 2, 2, 2, 2, 2, 2, 2, 2, 2, 2, 2, 2, 2, 2, 2, 2, 2, 2, 2, 2, 2, 2, 2, 2, 2, 2, 2, 2, 2, 2, 2, 2, 2, 2, 2, 2, 2, 2, 2, 2, 2, 2, 2, 2, 2, 2, 2, 2, 2, 2, 2, 2, 2, 2, 2, 2, 2, 2, 2, 2, 2, 2, 2, 2, 2, 2, 2, 2, 2, 2, 2, 2, 2, 2, 2, 2, 2, 2, 2, 2, 2, 2, 2, 2, 2, 2, 2, 2, 2, 2, 2, 2, 2, 2, 2, 2, 2, 2, 2, 2, 2, 2, 2, 2, 2, 2, 2, 2, 2, 2, 2, 2, 2, 2, 2, 2, 2, 2, 2, 2, 2, 2, 2, 2, 2, 2, 2, 2, 2, 2, 2, 2, 2, 2, 2, 2, 2, 2, 2, 2, 2, 2, 2, 2, 2, 2, 2, 3 ),
 ( 0.000000000000000000, 1.000000000000000000 ),
 ( 0.000000000000000000, 0.002777777777777777884, 0.005555555555555555768, 0.008333333333333333218, 0.01111111111111111154, 0.01388888888888888812, 0.01666666666666666644, 0.01944444444444444475, 0.02222222222222222307, 0.02500000000000000139, 0.02777777777777777624, 0.03055555555555555455, 0.03333333333333333287, 0.03611111111111110772, 0.03888888888888888951, 0.04166666666666666435, 0.04444444444444444614, 0.04722222222222222099, 0.05000000000000000278, 0.05277777777777777762, 0.05555555555555555247, 0.05833333333333333426, 0.06111111111111110911, 0.06388888888888888395, 0.06666666666666666574, 0.06944444444444444753, 0.07222222222222221544, 0.07499999999999999722, 0.07777777777777777901, 0.08055555555555556080, 0.08333333333333332871, 0.08611111111111111049, 0.08888888888888889228, 0.09166666666666666019, 0.09444444444444444198, 0.09722222222222222376, 0.1000000000000000056, 0.1027777777777777735, 0.1055555555555555552, 0.1083333333333333370, 0.1111111111111111049, 0.1138888888888888867, 0.1166666666666666685, 0.1194444444444444503, 0.1222222222222222182, 0.1250000000000000000, 0.1277777777777777679, 0.1305555555555555636, 0.1333333333333333315, 0.1361111111111110994, 0.1388888888888888951, 0.1416666666666666630, 0.1444444444444444309, 0.1472222222222222265, 0.1499999999999999944, 0.1527777777777777901, 0.1555555555555555580, 0.1583333333333333259, 0.1611111111111111216, 0.1638888888888888895, 0.1666666666666666574, 0.1694444444444444531, 0.1722222222222222210, 0.1749999999999999889, 0.1777777777777777846, 0.1805555555555555525, 0.1833333333333333204, 0.1861111111111111160, 0.1888888888888888840, 0.1916666666666666796, 0.1944444444444444475, 0.1972222222222222154, 0.2000000000000000111, 0.2027777777777777790, 0.2055555555555555469, 0.2083333333333333426, 0.2111111111111111105, 0.2138888888888888784, 0.2166666666666666741, 0.2194444444444444420, 0.2222222222222222099, 0.2250000000000000056, 0.2277777777777777735, 0.2305555555555555691, 0.2333333333333333370, 0.2361111111111111049, 0.2388888888888889006, 0.2416666666666666685, 0.2444444444444444364, 0.2472222222222222321, 0.2500000000000000000, 0.2527777777777777679, 0.2555555555555555358, 0.2583333333333333592, 0.2611111111111111271, 0.2638888888888888951, 0.2666666666666666630, 0.2694444444444444309, 0.2722222222222221988, 0.2750000000000000222, 0.2777777777777777901, 0.2805555555555555580, 0.2833333333333333259, 0.2861111111111110938, 0.2888888888888888618, 0.2916666666666666852, 0.2944444444444444531, 0.2972222222222222210, 0.2999999999999999889, 0.3027777777777777568, 0.3055555555555555802, 0.3083333333333333481, 0.3111111111111111160, 0.3138888888888888840, 0.3166666666666666519, 0.3194444444444444198, 0.3222222222222222432, 0.3250000000000000111, 0.3277777777777777790, 0.3305555555555555469, 0.3333333333333333148, 0.3361111111111111382, 0.3388888888888889062, 0.3416666666666666741, 0.3444444444444444420, 0.3472222222222222099, 0.3499999999999999778, 0.3527777777777778012, 0.3555555555555555691, 0.3583333333333333370, 0.3611111111111111049, 0.3638888888888888729, 0.3666666666666666408, 0.3694444444444444642, 0.3722222222222222321, 0.3750000000000000000, 0.3777777777777777679, 0.3805555555555555358, 0.3833333333333333592, 0.3861111111111111271, 0.3888888888888888951, 0.3916666666666666630, 0.3944444444444444309, 0.3972222222222221988, 0.4000000000000000222, 0.4027777777777777901, 0.4055555555555555580, 0.4083333333333333259, 0.4111111111111110938, 0.4138888888888888618, 0.4166666666666666852, 0.4194444444444444531, 0.4222222222222222210, 0.4249999999999999889, 0.4277777777777777568, 0.4305555555555555802, 0.4333333333333333481, 0.4361111111111111160, 0.4388888888888888840, 0.4416666666666666519, 0.4444444444444444198, 0.4472222222222222432, 0.4500000000000000111, 0.4527777777777777790, 0.4555555555555555469, 0.4583333333333333148, 0.4611111111111111382, 0.4638888888888889062, 0.4666666666666666741, 0.4694444444444444420, 0.4722222222222222099, 0.4749999999999999778, 0.4777777777777778012, 0.4805555555555555691, 0.4833333333333333370, 0.4861111111111111049, 0.4888888888888888729, 0.4916666666666666408, 0.4944444444444444642, 0.4972222222222222321, 0.5000000000000000000, 0.5027777777777777679, 0.5055555555555555358, 0.5083333333333333037, 0.5111111111111110716, 0.5138888888888888395, 0.5166666666666667185, 0.5194444444444444864, 0.5222222222222222543, 0.5250000000000000222, 0.5277777777777777901, 0.5305555555555555580, 0.5333333333333333259, 0.5361111111111110938, 0.5388888888888888618, 0.5416666666666666297, 0.5444444444444443976, 0.5472222222222222765, 0.5500000000000000444, 0.5527777777777778123, 0.5555555555555555802, 0.5583333333333333481, 0.5611111111111111160, 0.5638888888888888840, 0.5666666666666666519, 0.5694444444444444198, 0.5722222222222221877, 0.5749999999999999556, 0.5777777777777777235, 0.5805555555555556024, 0.5833333333333333703, 0.5861111111111111382, 0.5888888888888889062, 0.5916666666666666741, 0.5944444444444444420, 0.5972222222222222099, 0.5999999999999999778, 0.6027777777777777457, 0.6055555555555555136, 0.6083333333333332815, 0.6111111111111111605, 0.6138888888888889284, 0.6166666666666666963, 0.6194444444444444642, 0.6222222222222222321, 0.6250000000000000000, 0.6277777777777777679, 0.6305555555555555358, 0.6333333333333333037, 0.6361111111111110716, 0.6388888888888888395, 0.6416666666666667185, 0.6444444444444444864, 0.6472222222222222543, 0.6500000000000000222, 0.6527777777777777901, 0.6555555555555555580, 0.6583333333333333259, 0.6611111111111110938, 0.6638888888888888618, 0.6666666666666666297, 0.6694444444444443976, 0.6722222222222222765, 0.6750000000000000444, 0.6777777777777778123, 0.6805555555555555802, 0.6833333333333333481, 0.6861111111111111160, 0.6888888888888888840, 0.6916666666666666519, 0.6944444444444444198, 0.6972222222222221877, 0.6999999999999999556, 0.7027777777777777235, 0.7055555555555556024, 0.7083333333333333703, 0.7111111111111111382, 0.7138888888888889062, 0.7166666666666666741, 0.7194444444444444420, 0.7222222222222222099, 0.7249999999999999778, 0.7277777777777777457, 0.7305555555555555136, 0.7333333333333332815, 0.7361111111111111605, 0.7388888888888889284, 0.7416666666666666963, 0.7444444444444444642, 0.7472222222222222321, 0.7500000000000000000, 0.7527777777777777679, 0.7555555555555555358, 0.7583333333333333037, 0.7611111111111110716, 0.7638888888888888395, 0.7666666666666667185, 0.7694444444444444864, 0.7722222222222222543, 0.7750000000000000222, 0.7777777777777777901, 0.7805555555555555580, 0.7833333333333333259, 0.7861111111111110938, 0.7888888888888888618, 0.7916666666666666297, 0.7944444444444443976, 0.7972222222222222765, 0.8000000000000000444, 0.8027777777777778123, 0.8055555555555555802, 0.8083333333333333481, 0.8111111111111111160, 0.8138888888888888840, 0.8166666666666666519, 0.8194444444444444198, 0.8222222222222221877, 0.8249999999999999556, 0.8277777777777777235, 0.8305555555555556024, 0.8333333333333333703, 0.8361111111111111382, 0.8388888888888889062, 0.8416666666666666741, 0.8444444444444444420, 0.8472222222222222099, 0.8499999999999999778, 0.8527777777777777457, 0.8555555555555555136, 0.8583333333333332815, 0.8611111111111111605, 0.8638888888888889284, 0.8666666666666666963, 0.8694444444444444642, 0.8722222222222222321, 0.8750000000000000000, 0.8777777777777777679, 0.8805555555555555358, 0.8833333333333333037, 0.8861111111111110716, 0.8888888888888888395, 0.8916666666666667185, 0.8944444444444444864, 0.8972222222222222543, 0.9000000000000000222, 0.9027777777777777901, 0.9055555555555555580, 0.9083333333333333259, 0.9111111111111110938, 0.9138888888888888618, 0.9166666666666666297, 0.9194444444444443976, 0.9222222222222222765, 0.9250000000000000444, 0.9277777777777778123, 0.9305555555555555802, 0.9333333333333333481, 0.9361111111111111160, 0.9388888888888888840, 0.9416666666666666519, 0.9444444444444444198, 0.9472222222222221877, 0.9499999999999999556, 0.9527777777777777235, 0.9555555555555556024, 0.9583333333333333703, 0.9611111111111111382, 0.9638888888888889062, 0.9666666666666666741, 0.9694444444444444420, 0.9722222222222222099, 0.9749999999999999778, 0.9777777777777777457, 0.9805555555555555136, 0.9833333333333332815, 0.9861111111111111605, 0.9888888888888889284, 0.9916666666666666963, 0.9944444444444444642, 0.9972222222222222321, 1.000000000000000000 ),
 .UNSPECIFIED. ) 
 GEOMETRIC_REPRESENTATION_ITEM ( )  RATIONAL_B_SPLINE_SURFACE ( (
 ( 1.000000000000000000, 0.8660254037844387076, 1.000000000000000000, 0.8660254037844387076, 1.000000000000000000, 0.8660254037844387076, 1.000000000000000000, 0.8660254037844387076, 1.000000000000000000, 0.8660254037844387076, 1.000000000000000000, 0.8660254037844387076, 1.000000000000000000, 0.8660254037844387076, 1.000000000000000000, 0.8660254037844387076, 1.000000000000000000, 0.8660254037844387076, 1.000000000000000000, 0.8660254037844387076, 1.000000000000000000, 0.8660254037844387076, 1.000000000000000000, 0.8660254037844387076, 1.000000000000000000, 0.8660254037844387076, 1.000000000000000000, 0.8660254037844387076, 1.000000000000000000, 0.8660254037844387076, 1.000000000000000000, 0.8660254037844387076, 1.000000000000000000, 0.8660254037844387076, 1.000000000000000000, 0.8660254037844387076, 1.000000000000000000, 0.8660254037844387076, 1.000000000000000000, 0.8660254037844387076, 1.000000000000000000, 0.8660254037844387076, 1.000000000000000000, 0.8660254037844387076, 1.000000000000000000, 0.8660254037844387076, 1.000000000000000000, 0.8660254037844387076, 1.000000000000000000, 0.8660254037844387076, 1.000000000000000000, 0.8660254037844387076, 1.000000000000000000, 0.8660254037844387076, 1.000000000000000000, 0.8660254037844387076, 1.000000000000000000, 0.8660254037844387076, 1.000000000000000000, 0.8660254037844387076, 1.000000000000000000, 0.8660254037844387076, 1.000000000000000000, 0.8660254037844387076, 1.000000000000000000, 0.8660254037844387076, 1.000000000000000000, 0.8660254037844387076, 1.000000000000000000, 0.8660254037844387076, 1.000000000000000000, 0.8660254037844387076, 1.000000000000000000, 0.8660254037844387076, 1.000000000000000000, 0.8660254037844387076, 1.000000000000000000, 0.8660254037844387076, 1.000000000000000000, 0.8660254037844387076, 1.000000000000000000, 0.8660254037844387076, 1.000000000000000000, 0.8660254037844387076, 1.000000000000000000, 0.8660254037844387076, 1.000000000000000000, 0.8660254037844387076, 1.000000000000000000, 0.8660254037844387076, 1.000000000000000000, 0.8660254037844387076, 1.000000000000000000, 0.8660254037844387076, 1.000000000000000000, 0.8660254037844387076, 1.000000000000000000, 0.8660254037844387076, 1.000000000000000000, 0.8660254037844387076, 1.000000000000000000, 0.8660254037844387076, 1.000000000000000000, 0.8660254037844387076, 1.000000000000000000, 0.8660254037844387076, 1.000000000000000000, 0.8660254037844387076, 1.000000000000000000, 0.8660254037844387076, 1.000000000000000000, 0.8660254037844387076, 1.000000000000000000, 0.8660254037844387076, 1.000000000000000000, 0.8660254037844387076, 1.000000000000000000, 0.8660254037844387076, 1.000000000000000000, 0.8660254037844387076, 1.000000000000000000, 0.8660254037844387076, 1.000000000000000000, 0.8660254037844387076, 1.000000000000000000, 0.8660254037844387076, 1.000000000000000000, 0.8660254037844387076, 1.000000000000000000, 0.8660254037844387076, 1.000000000000000000, 0.8660254037844387076, 1.000000000000000000, 0.8660254037844387076, 1.000000000000000000, 0.8660254037844387076, 1.000000000000000000, 0.8660254037844387076, 1.000000000000000000, 0.8660254037844387076, 1.000000000000000000, 0.8660254037844387076, 1.000000000000000000, 0.8660254037844387076, 1.000000000000000000, 0.8660254037844387076, 1.000000000000000000, 0.8660254037844387076, 1.000000000000000000, 0.8660254037844387076, 1.000000000000000000, 0.8660254037844387076, 1.000000000000000000, 0.8660254037844387076, 1.000000000000000000, 0.8660254037844387076, 1.000000000000000000, 0.8660254037844387076, 1.000000000000000000, 0.8660254037844387076, 1.000000000000000000, 0.8660254037844387076, 1.000000000000000000, 0.8660254037844387076, 1.000000000000000000, 0.8660254037844387076, 1.000000000000000000, 0.8660254037844387076, 1.000000000000000000, 0.8660254037844387076, 1.000000000000000000, 0.8660254037844387076, 1.000000000000000000, 0.8660254037844387076, 1.000000000000000000, 0.8660254037844387076, 1.000000000000000000, 0.8660254037844387076, 1.000000000000000000, 0.8660254037844387076, 1.000000000000000000, 0.8660254037844387076, 1.000000000000000000, 0.8660254037844387076, 1.000000000000000000, 0.8660254037844387076, 1.000000000000000000, 0.8660254037844387076, 1.000000000000000000, 0.8660254037844387076, 1.000000000000000000, 0.8660254037844387076, 1.000000000000000000, 0.8660254037844387076, 1.000000000000000000, 0.8660254037844387076, 1.000000000000000000, 0.8660254037844387076, 1.000000000000000000, 0.8660254037844387076, 1.000000000000000000, 0.8660254037844387076, 1.000000000000000000, 0.8660254037844387076, 1.000000000000000000, 0.8660254037844387076, 1.000000000000000000, 0.8660254037844387076, 1.000000000000000000, 0.8660254037844387076, 1.000000000000000000, 0.8660254037844387076, 1.000000000000000000, 0.8660254037844387076, 1.000000000000000000, 0.8660254037844387076, 1.000000000000000000, 0.8660254037844387076, 1.000000000000000000, 0.8660254037844387076, 1.000000000000000000, 0.8660254037844387076, 1.000000000000000000, 0.8660254037844387076, 1.000000000000000000, 0.8660254037844387076, 1.000000000000000000, 0.8660254037844387076, 1.000000000000000000, 0.8660254037844387076, 1.000000000000000000, 0.8660254037844387076, 1.000000000000000000, 0.8660254037844387076, 1.000000000000000000, 0.8660254037844387076, 1.000000000000000000, 0.8660254037844387076, 1.000000000000000000, 0.8660254037844387076, 1.000000000000000000, 0.8660254037844387076, 1.000000000000000000, 0.8660254037844387076, 1.000000000000000000, 0.8660254037844387076, 1.000000000000000000, 0.8660254037844387076, 1.000000000000000000, 0.8660254037844387076, 1.000000000000000000, 0.8660254037844387076, 1.000000000000000000, 0.8660254037844387076, 1.000000000000000000, 0.8660254037844387076, 1.000000000000000000, 0.8660254037844387076, 1.000000000000000000, 0.8660254037844387076, 1.000000000000000000, 0.8660254037844387076, 1.000000000000000000, 0.8660254037844387076, 1.000000000000000000, 0.8660254037844387076, 1.000000000000000000, 0.8660254037844387076, 1.000000000000000000, 0.8660254037844387076, 1.000000000000000000, 0.8660254037844387076, 1.000000000000000000, 0.8660254037844387076, 1.000000000000000000, 0.8660254037844387076, 1.000000000000000000, 0.8660254037844387076, 1.000000000000000000, 0.8660254037844387076, 1.000000000000000000, 0.8660254037844387076, 1.000000000000000000, 0.8660254037844387076, 1.000000000000000000, 0.8660254037844387076, 1.000000000000000000, 0.8660254037844387076, 1.000000000000000000, 0.8660254037844387076, 1.000000000000000000, 0.8660254037844387076, 1.000000000000000000, 0.8660254037844387076, 1.000000000000000000, 0.8660254037844387076, 1.000000000000000000, 0.8660254037844387076, 1.000000000000000000, 0.8660254037844387076, 1.000000000000000000, 0.8660254037844387076, 1.000000000000000000, 0.8660254037844387076, 1.000000000000000000, 0.8660254037844387076, 1.000000000000000000, 0.8660254037844387076, 1.000000000000000000, 0.8660254037844387076, 1.000000000000000000, 0.8660254037844387076, 1.000000000000000000, 0.8660254037844387076, 1.000000000000000000, 0.8660254037844387076, 1.000000000000000000, 0.8660254037844387076, 1.000000000000000000, 0.8660254037844387076, 1.000000000000000000, 0.8660254037844387076, 1.000000000000000000, 0.8660254037844387076, 1.000000000000000000, 0.8660254037844387076, 1.000000000000000000, 0.8660254037844387076, 1.000000000000000000, 0.8660254037844387076, 1.000000000000000000, 0.8660254037844387076, 1.000000000000000000, 0.8660254037844387076, 1.000000000000000000, 0.8660254037844387076, 1.000000000000000000, 0.8660254037844387076, 1.000000000000000000, 0.8660254037844387076, 1.000000000000000000, 0.8660254037844387076, 1.000000000000000000, 0.8660254037844387076, 1.000000000000000000, 0.8660254037844387076, 1.000000000000000000, 0.8660254037844387076, 1.000000000000000000, 0.8660254037844387076, 1.000000000000000000, 0.8660254037844387076, 1.000000000000000000, 0.8660254037844387076, 1.000000000000000000, 0.8660254037844387076, 1.000000000000000000, 0.8660254037844387076, 1.000000000000000000, 0.8660254037844387076, 1.000000000000000000, 0.8660254037844387076, 1.000000000000000000, 0.8660254037844387076, 1.000000000000000000, 0.8660254037844387076, 1.000000000000000000, 0.8660254037844387076, 1.000000000000000000, 0.8660254037844387076, 1.000000000000000000, 0.8660254037844387076, 1.000000000000000000, 0.8660254037844387076, 1.000000000000000000, 0.8660254037844387076, 1.000000000000000000, 0.8660254037844387076, 1.000000000000000000, 0.8660254037844387076, 1.000000000000000000, 0.8660254037844387076, 1.000000000000000000, 0.8660254037844387076, 1.000000000000000000, 0.8660254037844387076, 1.000000000000000000, 0.8660254037844387076, 1.000000000000000000, 0.8660254037844387076, 1.000000000000000000, 0.8660254037844387076, 1.000000000000000000, 0.8660254037844387076, 1.000000000000000000, 0.8660254037844387076, 1.000000000000000000, 0.8660254037844387076, 1.000000000000000000, 0.8660254037844387076, 1.000000000000000000, 0.8660254037844387076, 1.000000000000000000, 0.8660254037844387076, 1.000000000000000000, 0.8660254037844387076, 1.000000000000000000, 0.8660254037844387076, 1.000000000000000000, 0.8660254037844387076, 1.000000000000000000, 0.8660254037844387076, 1.000000000000000000, 0.8660254037844387076, 1.000000000000000000, 0.8660254037844387076, 1.000000000000000000, 0.8660254037844387076, 1.000000000000000000, 0.8660254037844387076, 1.000000000000000000, 0.8660254037844387076, 1.000000000000000000, 0.8660254037844387076, 1.000000000000000000, 0.8660254037844387076, 1.000000000000000000, 0.8660254037844387076, 1.000000000000000000, 0.8660254037844387076, 1.000000000000000000, 0.8660254037844387076, 1.000000000000000000, 0.8660254037844387076, 1.000000000000000000, 0.8660254037844387076, 1.000000000000000000, 0.8660254037844387076, 1.000000000000000000, 0.8660254037844387076, 1.000000000000000000, 0.8660254037844387076, 1.000000000000000000, 0.8660254037844387076, 1.000000000000000000, 0.8660254037844387076, 1.000000000000000000, 0.8660254037844387076, 1.000000000000000000, 0.8660254037844387076, 1.000000000000000000, 0.8660254037844387076, 1.000000000000000000, 0.8660254037844387076, 1.000000000000000000, 0.8660254037844387076, 1.000000000000000000, 0.8660254037844387076, 1.000000000000000000, 0.8660254037844387076, 1.000000000000000000, 0.8660254037844387076, 1.000000000000000000, 0.8660254037844387076, 1.000000000000000000, 0.8660254037844387076, 1.000000000000000000, 0.8660254037844387076, 1.000000000000000000, 0.8660254037844387076, 1.000000000000000000, 0.8660254037844387076, 1.000000000000000000, 0.8660254037844387076, 1.000000000000000000, 0.8660254037844387076, 1.000000000000000000, 0.8660254037844387076, 1.000000000000000000, 0.8660254037844387076, 1.000000000000000000, 0.8660254037844387076, 1.000000000000000000, 0.8660254037844387076, 1.000000000000000000, 0.8660254037844387076, 1.000000000000000000, 0.8660254037844387076, 1.000000000000000000, 0.8660254037844387076, 1.000000000000000000, 0.8660254037844387076, 1.000000000000000000, 0.8660254037844387076, 1.000000000000000000, 0.8660254037844387076, 1.000000000000000000, 0.8660254037844387076, 1.000000000000000000, 0.8660254037844387076, 1.000000000000000000, 0.8660254037844387076, 1.000000000000000000, 0.8660254037844387076, 1.000000000000000000, 0.8660254037844387076, 1.000000000000000000, 0.8660254037844387076, 1.000000000000000000, 0.8660254037844387076, 1.000000000000000000, 0.8660254037844387076, 1.000000000000000000, 0.8660254037844387076, 1.000000000000000000, 0.8660254037844387076, 1.000000000000000000, 0.8660254037844387076, 1.000000000000000000, 0.8660254037844387076, 1.000000000000000000, 0.8660254037844387076, 1.000000000000000000, 0.8660254037844387076, 1.000000000000000000, 0.8660254037844387076, 1.000000000000000000, 0.8660254037844387076, 1.000000000000000000, 0.8660254037844387076, 1.000000000000000000, 0.8660254037844387076, 1.000000000000000000, 0.8660254037844387076, 1.000000000000000000, 0.8660254037844387076, 1.000000000000000000, 0.8660254037844387076, 1.000000000000000000, 0.8660254037844387076, 1.000000000000000000, 0.8660254037844387076, 1.000000000000000000, 0.8660254037844387076, 1.000000000000000000, 0.8660254037844387076, 1.000000000000000000, 0.8660254037844387076, 1.000000000000000000, 0.8660254037844387076, 1.000000000000000000, 0.8660254037844387076, 1.000000000000000000, 0.8660254037844387076, 1.000000000000000000, 0.8660254037844387076, 1.000000000000000000, 0.8660254037844387076, 1.000000000000000000, 0.8660254037844387076, 1.000000000000000000, 0.8660254037844387076, 1.000000000000000000, 0.8660254037844387076, 1.000000000000000000, 0.8660254037844387076, 1.000000000000000000, 0.8660254037844387076, 1.000000000000000000, 0.8660254037844387076, 1.000000000000000000, 0.8660254037844387076, 1.000000000000000000, 0.8660254037844387076, 1.000000000000000000, 0.8660254037844387076, 1.000000000000000000, 0.8660254037844387076, 1.000000000000000000, 0.8660254037844387076, 1.000000000000000000, 0.8660254037844387076, 1.000000000000000000, 0.8660254037844387076, 1.000000000000000000, 0.8660254037844387076, 1.000000000000000000, 0.8660254037844387076, 1.000000000000000000, 0.8660254037844387076, 1.000000000000000000, 0.8660254037844387076, 1.000000000000000000, 0.8660254037844387076, 1.000000000000000000, 0.8660254037844387076, 1.000000000000000000, 0.8660254037844387076, 1.000000000000000000, 0.8660254037844387076, 1.000000000000000000, 0.8660254037844387076, 1.000000000000000000, 0.8660254037844387076, 1.000000000000000000, 0.8660254037844387076, 1.000000000000000000, 0.8660254037844387076, 1.000000000000000000, 0.8660254037844387076, 1.000000000000000000, 0.8660254037844387076, 1.000000000000000000, 0.8660254037844387076, 1.000000000000000000, 0.8660254037844387076, 1.000000000000000000, 0.8660254037844387076, 1.000000000000000000, 0.8660254037844387076, 1.000000000000000000, 0.8660254037844387076, 1.000000000000000000, 0.8660254037844387076, 1.000000000000000000, 0.8660254037844387076, 1.000000000000000000, 0.8660254037844387076, 1.000000000000000000, 0.8660254037844387076, 1.000000000000000000, 0.8660254037844387076, 1.000000000000000000, 0.8660254037844387076, 1.000000000000000000, 0.8660254037844387076, 1.000000000000000000, 0.8660254037844387076, 1.000000000000000000, 0.8660254037844387076, 1.000000000000000000, 0.8660254037844387076, 1.000000000000000000, 0.8660254037844387076, 1.000000000000000000, 0.8660254037844387076, 1.000000000000000000, 0.8660254037844387076, 1.000000000000000000, 0.8660254037844387076, 1.000000000000000000, 0.8660254037844387076, 1.000000000000000000, 0.8660254037844387076, 1.000000000000000000, 0.8660254037844387076, 1.000000000000000000, 0.8660254037844387076, 1.000000000000000000, 0.8660254037844387076, 1.000000000000000000, 0.8660254037844387076, 1.000000000000000000, 0.8660254037844387076, 1.000000000000000000, 0.8660254037844387076, 1.000000000000000000, 0.8660254037844387076, 1.000000000000000000, 0.8660254037844387076, 1.000000000000000000, 0.8660254037844387076, 1.000000000000000000, 0.8660254037844387076, 1.000000000000000000, 0.8660254037844387076, 1.000000000000000000, 0.8660254037844387076, 1.000000000000000000, 0.8660254037844387076, 1.000000000000000000, 0.8660254037844387076, 1.000000000000000000, 0.8660254037844387076, 1.000000000000000000, 0.8660254037844387076, 1.000000000000000000, 0.8660254037844387076, 1.000000000000000000, 0.8660254037844387076, 1.000000000000000000, 0.8660254037844387076, 1.000000000000000000, 0.8660254037844387076, 1.000000000000000000, 0.8660254037844387076, 1.000000000000000000, 0.8660254037844387076, 1.000000000000000000, 0.8660254037844387076, 1.000000000000000000, 0.8660254037844387076, 1.000000000000000000, 0.8660254037844387076, 1.000000000000000000, 0.8660254037844387076, 1.000000000000000000, 0.8660254037844387076, 1.000000000000000000, 0.8660254037844387076, 1.000000000000000000, 0.8660254037844387076, 1.000000000000000000, 0.8660254037844387076, 1.000000000000000000, 0.8660254037844387076, 1.000000000000000000, 0.8660254037844387076, 1.000000000000000000, 0.8660254037844387076, 1.000000000000000000),
 ( 1.000000000000000000, 0.8660254037844387076, 1.000000000000000000, 0.8660254037844387076, 1.000000000000000000, 0.8660254037844387076, 1.000000000000000000, 0.8660254037844387076, 1.000000000000000000, 0.8660254037844387076, 1.000000000000000000, 0.8660254037844387076, 1.000000000000000000, 0.8660254037844387076, 1.000000000000000000, 0.8660254037844387076, 1.000000000000000000, 0.8660254037844387076, 1.000000000000000000, 0.8660254037844387076, 1.000000000000000000, 0.8660254037844387076, 1.000000000000000000, 0.8660254037844387076, 1.000000000000000000, 0.8660254037844387076, 1.000000000000000000, 0.8660254037844387076, 1.000000000000000000, 0.8660254037844387076, 1.000000000000000000, 0.8660254037844387076, 1.000000000000000000, 0.8660254037844387076, 1.000000000000000000, 0.8660254037844387076, 1.000000000000000000, 0.8660254037844387076, 1.000000000000000000, 0.8660254037844387076, 1.000000000000000000, 0.8660254037844387076, 1.000000000000000000, 0.8660254037844387076, 1.000000000000000000, 0.8660254037844387076, 1.000000000000000000, 0.8660254037844387076, 1.000000000000000000, 0.8660254037844387076, 1.000000000000000000, 0.8660254037844387076, 1.000000000000000000, 0.8660254037844387076, 1.000000000000000000, 0.8660254037844387076, 1.000000000000000000, 0.8660254037844387076, 1.000000000000000000, 0.8660254037844387076, 1.000000000000000000, 0.8660254037844387076, 1.000000000000000000, 0.8660254037844387076, 1.000000000000000000, 0.8660254037844387076, 1.000000000000000000, 0.8660254037844387076, 1.000000000000000000, 0.8660254037844387076, 1.000000000000000000, 0.8660254037844387076, 1.000000000000000000, 0.8660254037844387076, 1.000000000000000000, 0.8660254037844387076, 1.000000000000000000, 0.8660254037844387076, 1.000000000000000000, 0.8660254037844387076, 1.000000000000000000, 0.8660254037844387076, 1.000000000000000000, 0.8660254037844387076, 1.000000000000000000, 0.8660254037844387076, 1.000000000000000000, 0.8660254037844387076, 1.000000000000000000, 0.8660254037844387076, 1.000000000000000000, 0.8660254037844387076, 1.000000000000000000, 0.8660254037844387076, 1.000000000000000000, 0.8660254037844387076, 1.000000000000000000, 0.8660254037844387076, 1.000000000000000000, 0.8660254037844387076, 1.000000000000000000, 0.8660254037844387076, 1.000000000000000000, 0.8660254037844387076, 1.000000000000000000, 0.8660254037844387076, 1.000000000000000000, 0.8660254037844387076, 1.000000000000000000, 0.8660254037844387076, 1.000000000000000000, 0.8660254037844387076, 1.000000000000000000, 0.8660254037844387076, 1.000000000000000000, 0.8660254037844387076, 1.000000000000000000, 0.8660254037844387076, 1.000000000000000000, 0.8660254037844387076, 1.000000000000000000, 0.8660254037844387076, 1.000000000000000000, 0.8660254037844387076, 1.000000000000000000, 0.8660254037844387076, 1.000000000000000000, 0.8660254037844387076, 1.000000000000000000, 0.8660254037844387076, 1.000000000000000000, 0.8660254037844387076, 1.000000000000000000, 0.8660254037844387076, 1.000000000000000000, 0.8660254037844387076, 1.000000000000000000, 0.8660254037844387076, 1.000000000000000000, 0.8660254037844387076, 1.000000000000000000, 0.8660254037844387076, 1.000000000000000000, 0.8660254037844387076, 1.000000000000000000, 0.8660254037844387076, 1.000000000000000000, 0.8660254037844387076, 1.000000000000000000, 0.8660254037844387076, 1.000000000000000000, 0.8660254037844387076, 1.000000000000000000, 0.8660254037844387076, 1.000000000000000000, 0.8660254037844387076, 1.000000000000000000, 0.8660254037844387076, 1.000000000000000000, 0.8660254037844387076, 1.000000000000000000, 0.8660254037844387076, 1.000000000000000000, 0.8660254037844387076, 1.000000000000000000, 0.8660254037844387076, 1.000000000000000000, 0.8660254037844387076, 1.000000000000000000, 0.8660254037844387076, 1.000000000000000000, 0.8660254037844387076, 1.000000000000000000, 0.8660254037844387076, 1.000000000000000000, 0.8660254037844387076, 1.000000000000000000, 0.8660254037844387076, 1.000000000000000000, 0.8660254037844387076, 1.000000000000000000, 0.8660254037844387076, 1.000000000000000000, 0.8660254037844387076, 1.000000000000000000, 0.8660254037844387076, 1.000000000000000000, 0.8660254037844387076, 1.000000000000000000, 0.8660254037844387076, 1.000000000000000000, 0.8660254037844387076, 1.000000000000000000, 0.8660254037844387076, 1.000000000000000000, 0.8660254037844387076, 1.000000000000000000, 0.8660254037844387076, 1.000000000000000000, 0.8660254037844387076, 1.000000000000000000, 0.8660254037844387076, 1.000000000000000000, 0.8660254037844387076, 1.000000000000000000, 0.8660254037844387076, 1.000000000000000000, 0.8660254037844387076, 1.000000000000000000, 0.8660254037844387076, 1.000000000000000000, 0.8660254037844387076, 1.000000000000000000, 0.8660254037844387076, 1.000000000000000000, 0.8660254037844387076, 1.000000000000000000, 0.8660254037844387076, 1.000000000000000000, 0.8660254037844387076, 1.000000000000000000, 0.8660254037844387076, 1.000000000000000000, 0.8660254037844387076, 1.000000000000000000, 0.8660254037844387076, 1.000000000000000000, 0.8660254037844387076, 1.000000000000000000, 0.8660254037844387076, 1.000000000000000000, 0.8660254037844387076, 1.000000000000000000, 0.8660254037844387076, 1.000000000000000000, 0.8660254037844387076, 1.000000000000000000, 0.8660254037844387076, 1.000000000000000000, 0.8660254037844387076, 1.000000000000000000, 0.8660254037844387076, 1.000000000000000000, 0.8660254037844387076, 1.000000000000000000, 0.8660254037844387076, 1.000000000000000000, 0.8660254037844387076, 1.000000000000000000, 0.8660254037844387076, 1.000000000000000000, 0.8660254037844387076, 1.000000000000000000, 0.8660254037844387076, 1.000000000000000000, 0.8660254037844387076, 1.000000000000000000, 0.8660254037844387076, 1.000000000000000000, 0.8660254037844387076, 1.000000000000000000, 0.8660254037844387076, 1.000000000000000000, 0.8660254037844387076, 1.000000000000000000, 0.8660254037844387076, 1.000000000000000000, 0.8660254037844387076, 1.000000000000000000, 0.8660254037844387076, 1.000000000000000000, 0.8660254037844387076, 1.000000000000000000, 0.8660254037844387076, 1.000000000000000000, 0.8660254037844387076, 1.000000000000000000, 0.8660254037844387076, 1.000000000000000000, 0.8660254037844387076, 1.000000000000000000, 0.8660254037844387076, 1.000000000000000000, 0.8660254037844387076, 1.000000000000000000, 0.8660254037844387076, 1.000000000000000000, 0.8660254037844387076, 1.000000000000000000, 0.8660254037844387076, 1.000000000000000000, 0.8660254037844387076, 1.000000000000000000, 0.8660254037844387076, 1.000000000000000000, 0.8660254037844387076, 1.000000000000000000, 0.8660254037844387076, 1.000000000000000000, 0.8660254037844387076, 1.000000000000000000, 0.8660254037844387076, 1.000000000000000000, 0.8660254037844387076, 1.000000000000000000, 0.8660254037844387076, 1.000000000000000000, 0.8660254037844387076, 1.000000000000000000, 0.8660254037844387076, 1.000000000000000000, 0.8660254037844387076, 1.000000000000000000, 0.8660254037844387076, 1.000000000000000000, 0.8660254037844387076, 1.000000000000000000, 0.8660254037844387076, 1.000000000000000000, 0.8660254037844387076, 1.000000000000000000, 0.8660254037844387076, 1.000000000000000000, 0.8660254037844387076, 1.000000000000000000, 0.8660254037844387076, 1.000000000000000000, 0.8660254037844387076, 1.000000000000000000, 0.8660254037844387076, 1.000000000000000000, 0.8660254037844387076, 1.000000000000000000, 0.8660254037844387076, 1.000000000000000000, 0.8660254037844387076, 1.000000000000000000, 0.8660254037844387076, 1.000000000000000000, 0.8660254037844387076, 1.000000000000000000, 0.8660254037844387076, 1.000000000000000000, 0.8660254037844387076, 1.000000000000000000, 0.8660254037844387076, 1.000000000000000000, 0.8660254037844387076, 1.000000000000000000, 0.8660254037844387076, 1.000000000000000000, 0.8660254037844387076, 1.000000000000000000, 0.8660254037844387076, 1.000000000000000000, 0.8660254037844387076, 1.000000000000000000, 0.8660254037844387076, 1.000000000000000000, 0.8660254037844387076, 1.000000000000000000, 0.8660254037844387076, 1.000000000000000000, 0.8660254037844387076, 1.000000000000000000, 0.8660254037844387076, 1.000000000000000000, 0.8660254037844387076, 1.000000000000000000, 0.8660254037844387076, 1.000000000000000000, 0.8660254037844387076, 1.000000000000000000, 0.8660254037844387076, 1.000000000000000000, 0.8660254037844387076, 1.000000000000000000, 0.8660254037844387076, 1.000000000000000000, 0.8660254037844387076, 1.000000000000000000, 0.8660254037844387076, 1.000000000000000000, 0.8660254037844387076, 1.000000000000000000, 0.8660254037844387076, 1.000000000000000000, 0.8660254037844387076, 1.000000000000000000, 0.8660254037844387076, 1.000000000000000000, 0.8660254037844387076, 1.000000000000000000, 0.8660254037844387076, 1.000000000000000000, 0.8660254037844387076, 1.000000000000000000, 0.8660254037844387076, 1.000000000000000000, 0.8660254037844387076, 1.000000000000000000, 0.8660254037844387076, 1.000000000000000000, 0.8660254037844387076, 1.000000000000000000, 0.8660254037844387076, 1.000000000000000000, 0.8660254037844387076, 1.000000000000000000, 0.8660254037844387076, 1.000000000000000000, 0.8660254037844387076, 1.000000000000000000, 0.8660254037844387076, 1.000000000000000000, 0.8660254037844387076, 1.000000000000000000, 0.8660254037844387076, 1.000000000000000000, 0.8660254037844387076, 1.000000000000000000, 0.8660254037844387076, 1.000000000000000000, 0.8660254037844387076, 1.000000000000000000, 0.8660254037844387076, 1.000000000000000000, 0.8660254037844387076, 1.000000000000000000, 0.8660254037844387076, 1.000000000000000000, 0.8660254037844387076, 1.000000000000000000, 0.8660254037844387076, 1.000000000000000000, 0.8660254037844387076, 1.000000000000000000, 0.8660254037844387076, 1.000000000000000000, 0.8660254037844387076, 1.000000000000000000, 0.8660254037844387076, 1.000000000000000000, 0.8660254037844387076, 1.000000000000000000, 0.8660254037844387076, 1.000000000000000000, 0.8660254037844387076, 1.000000000000000000, 0.8660254037844387076, 1.000000000000000000, 0.8660254037844387076, 1.000000000000000000, 0.8660254037844387076, 1.000000000000000000, 0.8660254037844387076, 1.000000000000000000, 0.8660254037844387076, 1.000000000000000000, 0.8660254037844387076, 1.000000000000000000, 0.8660254037844387076, 1.000000000000000000, 0.8660254037844387076, 1.000000000000000000, 0.8660254037844387076, 1.000000000000000000, 0.8660254037844387076, 1.000000000000000000, 0.8660254037844387076, 1.000000000000000000, 0.8660254037844387076, 1.000000000000000000, 0.8660254037844387076, 1.000000000000000000, 0.8660254037844387076, 1.000000000000000000, 0.8660254037844387076, 1.000000000000000000, 0.8660254037844387076, 1.000000000000000000, 0.8660254037844387076, 1.000000000000000000, 0.8660254037844387076, 1.000000000000000000, 0.8660254037844387076, 1.000000000000000000, 0.8660254037844387076, 1.000000000000000000, 0.8660254037844387076, 1.000000000000000000, 0.8660254037844387076, 1.000000000000000000, 0.8660254037844387076, 1.000000000000000000, 0.8660254037844387076, 1.000000000000000000, 0.8660254037844387076, 1.000000000000000000, 0.8660254037844387076, 1.000000000000000000, 0.8660254037844387076, 1.000000000000000000, 0.8660254037844387076, 1.000000000000000000, 0.8660254037844387076, 1.000000000000000000, 0.8660254037844387076, 1.000000000000000000, 0.8660254037844387076, 1.000000000000000000, 0.8660254037844387076, 1.000000000000000000, 0.8660254037844387076, 1.000000000000000000, 0.8660254037844387076, 1.000000000000000000, 0.8660254037844387076, 1.000000000000000000, 0.8660254037844387076, 1.000000000000000000, 0.8660254037844387076, 1.000000000000000000, 0.8660254037844387076, 1.000000000000000000, 0.8660254037844387076, 1.000000000000000000, 0.8660254037844387076, 1.000000000000000000, 0.8660254037844387076, 1.000000000000000000, 0.8660254037844387076, 1.000000000000000000, 0.8660254037844387076, 1.000000000000000000, 0.8660254037844387076, 1.000000000000000000, 0.8660254037844387076, 1.000000000000000000, 0.8660254037844387076, 1.000000000000000000, 0.8660254037844387076, 1.000000000000000000, 0.8660254037844387076, 1.000000000000000000, 0.8660254037844387076, 1.000000000000000000, 0.8660254037844387076, 1.000000000000000000, 0.8660254037844387076, 1.000000000000000000, 0.8660254037844387076, 1.000000000000000000, 0.8660254037844387076, 1.000000000000000000, 0.8660254037844387076, 1.000000000000000000, 0.8660254037844387076, 1.000000000000000000, 0.8660254037844387076, 1.000000000000000000, 0.8660254037844387076, 1.000000000000000000, 0.8660254037844387076, 1.000000000000000000, 0.8660254037844387076, 1.000000000000000000, 0.8660254037844387076, 1.000000000000000000, 0.8660254037844387076, 1.000000000000000000, 0.8660254037844387076, 1.000000000000000000, 0.8660254037844387076, 1.000000000000000000, 0.8660254037844387076, 1.000000000000000000, 0.8660254037844387076, 1.000000000000000000, 0.8660254037844387076, 1.000000000000000000, 0.8660254037844387076, 1.000000000000000000, 0.8660254037844387076, 1.000000000000000000, 0.8660254037844387076, 1.000000000000000000, 0.8660254037844387076, 1.000000000000000000, 0.8660254037844387076, 1.000000000000000000, 0.8660254037844387076, 1.000000000000000000, 0.8660254037844387076, 1.000000000000000000, 0.8660254037844387076, 1.000000000000000000, 0.8660254037844387076, 1.000000000000000000, 0.8660254037844387076, 1.000000000000000000, 0.8660254037844387076, 1.000000000000000000, 0.8660254037844387076, 1.000000000000000000, 0.8660254037844387076, 1.000000000000000000, 0.8660254037844387076, 1.000000000000000000, 0.8660254037844387076, 1.000000000000000000, 0.8660254037844387076, 1.000000000000000000, 0.8660254037844387076, 1.000000000000000000, 0.8660254037844387076, 1.000000000000000000, 0.8660254037844387076, 1.000000000000000000, 0.8660254037844387076, 1.000000000000000000, 0.8660254037844387076, 1.000000000000000000, 0.8660254037844387076, 1.000000000000000000, 0.8660254037844387076, 1.000000000000000000, 0.8660254037844387076, 1.000000000000000000, 0.8660254037844387076, 1.000000000000000000, 0.8660254037844387076, 1.000000000000000000, 0.8660254037844387076, 1.000000000000000000, 0.8660254037844387076, 1.000000000000000000, 0.8660254037844387076, 1.000000000000000000, 0.8660254037844387076, 1.000000000000000000, 0.8660254037844387076, 1.000000000000000000, 0.8660254037844387076, 1.000000000000000000, 0.8660254037844387076, 1.000000000000000000, 0.8660254037844387076, 1.000000000000000000, 0.8660254037844387076, 1.000000000000000000, 0.8660254037844387076, 1.000000000000000000, 0.8660254037844387076, 1.000000000000000000, 0.8660254037844387076, 1.000000000000000000, 0.8660254037844387076, 1.000000000000000000, 0.8660254037844387076, 1.000000000000000000, 0.8660254037844387076, 1.000000000000000000, 0.8660254037844387076, 1.000000000000000000, 0.8660254037844387076, 1.000000000000000000, 0.8660254037844387076, 1.000000000000000000, 0.8660254037844387076, 1.000000000000000000, 0.8660254037844387076, 1.000000000000000000, 0.8660254037844387076, 1.000000000000000000, 0.8660254037844387076, 1.000000000000000000, 0.8660254037844387076, 1.000000000000000000, 0.8660254037844387076, 1.000000000000000000, 0.8660254037844387076, 1.000000000000000000, 0.8660254037844387076, 1.000000000000000000, 0.8660254037844387076, 1.000000000000000000, 0.8660254037844387076, 1.000000000000000000, 0.8660254037844387076, 1.000000000000000000, 0.8660254037844387076, 1.000000000000000000, 0.8660254037844387076, 1.000000000000000000, 0.8660254037844387076, 1.000000000000000000, 0.8660254037844387076, 1.000000000000000000, 0.8660254037844387076, 1.000000000000000000, 0.8660254037844387076, 1.000000000000000000, 0.8660254037844387076, 1.000000000000000000, 0.8660254037844387076, 1.000000000000000000, 0.8660254037844387076, 1.000000000000000000, 0.8660254037844387076, 1.000000000000000000, 0.8660254037844387076, 1.000000000000000000, 0.8660254037844387076, 1.000000000000000000, 0.8660254037844387076, 1.000000000000000000, 0.8660254037844387076, 1.000000000000000000, 0.8660254037844387076, 1.000000000000000000) ) ) 
 REPRESENTATION_ITEM ( '' )  SURFACE ( )  );
#63765 = CARTESIAN_POINT ( 'NONE',  ( 15.18750000122903465, 4.330127018922191873, 2.499999999999999556 ) ) ;
#63766 = CARTESIAN_POINT ( 'NONE',  ( 18.30000000000000071, 0.000000000000000000, 4.999999999999998224 ) ) ;
#63767 = CARTESIAN_POINT ( 'NONE',  ( 28.12499999999999645, 4.330127018922191873, 2.499999999999999556 ) ) ;
#63768 = CARTESIAN_POINT ( 'NONE',  ( 4.021875000614516082, 3.027376345333613106, -5.243569643749998122 ) ) ;
#63769 = CARTESIAN_POINT ( 'NONE',  ( 8.896875000614517859, -3.027376345333610441, -5.243569643749999898 ) ) ;
#63770 = CARTESIAN_POINT ( 'NONE',  ( 19.05937500061451928, 0.000000000000000000, 5.243569643749999010 ) ) ;
#63771 = DIRECTION ( 'NONE',  ( 0.000000000000000000, 0.000000000000000000, 1.000000000000000000 ) ) ;
#63772 = ORIENTED_EDGE ( 'NONE', *, *, #2473, .F. ) ;
#63773 = CARTESIAN_POINT ( 'NONE',  ( 28.86562500061451786, 3.027376345333611329, 5.243569643749999010 ) ) ;
#63774 = CARTESIAN_POINT ( 'NONE',  ( 3.412500000000002309, 2.886751345948126879, 4.999999999999999112 ) ) ;
#63775 = CARTESIAN_POINT ( 'NONE',  ( 4.809375000614516615, -4.541064518000417216, -2.621784821875001281 ) ) ;
#63776 = CARTESIAN_POINT ( 'NONE',  ( 16.12500000000000000, -4.330127018922194537, 2.499999999999995559 ) ) ;
#63777 = CARTESIAN_POINT ( 'NONE',  ( 14.42812500061451786, 4.541064518000418104, 2.621784821874999949 ) ) ;
#63778 = CARTESIAN_POINT ( 'NONE',  ( 2.828200636599751609E-16, 18.91249999999999787, 25.38119784648299415 ) ) ;
#63779 = CARTESIAN_POINT ( 'NONE',  ( 18.11250000000000071, 2.886751345948129099, -4.999999999999997335 ) ) ;
#63780 = CARTESIAN_POINT ( 'NONE',  ( 17.55000000122903359, -2.886751345948129988, 4.999999999999997335 ) ) ;
#63781 = CARTESIAN_POINT ( 'NONE',  ( 4.898587196589411843E-16, 20.00000000000000000, -26.00000000000000000 ) ) ;
#63782 = CARTESIAN_POINT ( 'NONE',  ( 20.93437500061451573, -4.119189519843968306, 2.378215178124996054 ) ) ;
#63783 = CARTESIAN_POINT ( 'NONE',  ( 6.590625000614518392, -3.027376345333610441, -5.243569643749999898 ) ) ;
#63784 = CARTESIAN_POINT ( 'NONE',  ( 24.90937500061451715, 0.000000000000000000, 5.243569643749999010 ) ) ;
#63785 = CARTESIAN_POINT ( 'NONE',  ( 4.243569643749999898, 18.73437500061451644, 30.00000000000000000 ) ) ;
#63786 = CARTESIAN_POINT ( 'NONE',  ( 27.60937500061451644, 0.000000000000000000, 5.243569643749999010 ) ) ;
#63787 = CARTESIAN_POINT ( 'NONE',  ( 8.287499999999999645, 5.773502691896255534, 3.535250795749688894E-16 ) ) ;
#63788 = CARTESIAN_POINT ( 'NONE',  ( 4.000000000000000000, 12.65000000122903501, 32.30940107675849049 ) ) ;
#63789 = CARTESIAN_POINT ( 'NONE',  ( 14.76562500061451821, 3.027376345333613106, -5.243569643749998122 ) ) ;
#63790 = CARTESIAN_POINT ( 'NONE',  ( 5.925000001229033586, -5.773502691896255534, -1.060575238724906372E-15 ) ) ;
#63791 = CARTESIAN_POINT ( 'NONE',  ( 16.77187500061451786, 3.027376345333611329, 5.243569643749999010 ) ) ;
#63792 = CARTESIAN_POINT ( 'NONE',  ( 12.00937500061451857, -4.541064518000417216, -2.621784821875001281 ) ) ;
#63793 = DIRECTION ( 'NONE',  ( 0.000000000000000000, 0.000000000000000000, 1.000000000000000000 ) ) ;
#63794 = ORIENTED_EDGE ( 'NONE', *, *, #55505, .F. ) ;
#63795 = CARTESIAN_POINT ( 'NONE',  ( 11.42812500061451608, -4.541064518000419881, 2.621784821874995952 ) ) ;
#63796 = CARTESIAN_POINT ( 'NONE',  ( 0.000000000000000000, 27.50000000000000000, 26.00000000000000000 ) ) ;
#63797 = CARTESIAN_POINT ( 'NONE',  ( 23.10000000122903074, -2.886751345948125991, -5.000000000000000000 ) ) ;
#63798 = CARTESIAN_POINT ( 'NONE',  ( 12.23437500061451821, 4.541064518000418104, 2.621784821874999949 ) ) ;
#63799 = CARTESIAN_POINT ( 'NONE',  ( 15.02812500061451750, -4.541064518000419881, 2.621784821874995952 ) ) ;
#63800 = CARTESIAN_POINT ( 'NONE',  ( 4.898587196589412829E-16, 27.50000000000000000, 34.00000000000000000 ) ) ;
#63801 = CARTESIAN_POINT ( 'NONE',  ( 23.40937500061451715, 4.541064518000418104, -2.621784821874998173 ) ) ;
#63802 = DIRECTION ( 'NONE',  ( 0.000000000000000000, 0.000000000000000000, -1.000000000000000000 ) ) ;
#63803 = DIRECTION ( 'NONE',  ( -1.000000000000000000, -0.000000000000000000, -0.000000000000000000 ) ) ;
#63804 = CARTESIAN_POINT ( 'NONE',  ( -2.121784821874999949, 17.53437500061451715, -33.67503911421598417 ) ) ;
#63805 = CARTESIAN_POINT ( 'NONE',  ( 14.70937500061451786, -4.541064518000417216, -2.621784821875001281 ) ) ;
#63806 = CARTESIAN_POINT ( 'NONE',  ( 17.92500000122903359, 2.886751345948126879, 4.999999999999999112 ) ) ;
#63807 = CARTESIAN_POINT ( 'NONE',  ( 12.42187500061451821, -6.054752690667223547, -1.112240025338166033E-15 ) ) ;
#63808 = CARTESIAN_POINT ( 'NONE',  ( 9.001249775931846008E-16, 10.07187500061451857, 34.90005215228797653 ) ) ;
#63809 = CARTESIAN_POINT ( 'NONE',  ( 18.90000000122902790, -2.886751345948129988, 4.999999999999997335 ) ) ;
#63810 = CARTESIAN_POINT ( 'NONE',  ( 12.06562500061451537, 3.027376345333613106, -5.243569643749998122 ) ) ;
#63811 = ORIENTED_EDGE ( 'NONE', *, *, #53665, .F. ) ;
#63812 = ORIENTED_EDGE ( 'NONE', *, *, #22708, .T. ) ;
#63813 = CARTESIAN_POINT ( 'NONE',  ( 18.71249999999999858, 2.886751345948126879, 4.999999999999999112 ) ) ;
#63814 = CARTESIAN_POINT ( 'NONE',  ( -4.243569643749999898, 19.80312500061451786, 30.00000000000000000 ) ) ;
#63815 = CARTESIAN_POINT ( 'NONE',  ( 12.08437500061451608, 6.421520780324663323E-16, -5.243569643749999010 ) ) ;
#63816 = CARTESIAN_POINT ( 'NONE',  ( 4.077828214794575246, 2.893468368387148271, 4.305173067005224397 ) ) ;
#63817 = CARTESIAN_POINT ( 'NONE',  ( 11.77500000122903501, -5.773502691896255534, -1.060575238724906372E-15 ) ) ;
#63818 = CARTESIAN_POINT ( 'NONE',  ( 20.85000000122903430, -2.886751345948125991, -5.000000000000000000 ) ) ;
#63819 = CARTESIAN_POINT ( 'NONE',  ( 17.05312500061451786, 4.541064518000418104, -2.621784821874998173 ) ) ;
#63820 = CARTESIAN_POINT ( 'NONE',  ( 22.19062500061451715, -3.027376345333614438, 5.243569643749998122 ) ) ;
#63821 = CARTESIAN_POINT ( 'NONE',  ( 29.21250000122903145, 0.000000000000000000, 4.999999999999998224 ) ) ;
#63822 = CARTESIAN_POINT ( 'NONE',  ( 27.22499999999999787, 4.330127018922191873, 2.499999999999999556 ) ) ;
#63823 = CARTESIAN_POINT ( 'NONE',  ( 4.615116929606795537, 1.923719243043608307, 4.877942894581709155 ) ) ;
#63824 = CARTESIAN_POINT ( 'NONE',  ( 29.21249999999999858, -5.773502691896255534, -1.060575238724906372E-15 ) ) ;
#63825 = DIRECTION ( 'NONE',  ( 0.000000000000000000, 0.000000000000000000, -1.000000000000000000 ) ) ;
#63826 = CARTESIAN_POINT ( 'NONE',  ( 4.000000000000000000, 9.950000001229035718, -27.69059892324149530 ) ) ;
#63827 = CARTESIAN_POINT ( 'NONE',  ( -4.243569643749999898, 15.32187500061451679, -32.45002607614398471 ) ) ;
#63828 = CARTESIAN_POINT ( 'NONE',  ( 4.912500001229034297, 0.000000000000000000, 4.999999999999998224 ) ) ;
#63829 = CARTESIAN_POINT ( 'NONE',  ( 6.675000000000000711, -4.330127018922194537, 2.499999999999995559 ) ) ;
#63830 = EDGE_CURVE ( 'NONE', #39550, #72150, #69713, .T. ) ;
#63831 = CARTESIAN_POINT ( 'NONE',  ( 3.609375000614516882, 4.541064518000418104, -2.621784821874998173 ) ) ;
#63832 = CARTESIAN_POINT ( 'NONE',  ( 10.28437500061451715, 6.421520780324663323E-16, -5.243569643749999010 ) ) ;
#63833 = CARTESIAN_POINT ( 'NONE',  ( 29.57812500061451644, 6.421520780324663323E-16, -5.243569643749999010 ) ) ;
#63834 = CARTESIAN_POINT ( 'NONE',  ( 1.071796769724489895, 10.86740381056766758, 26.00000000000000355 ) ) ;
#63835 = CARTESIAN_POINT ( 'NONE',  ( -5.948681673321859265, 8.038272906428572284, -30.80841975699791746 ) ) ;
#63836 = CARTESIAN_POINT ( 'NONE',  ( 29.83125000061451715, 0.000000000000000000, 4.999999999999998224 ) ) ;
#63837 = CARTESIAN_POINT ( 'NONE',  ( 7.509375000614517681, -4.541064518000417216, -2.621784821875001281 ) ) ;
#63838 = CARTESIAN_POINT ( 'NONE',  ( 12.00937500061451857, -4.541064518000417216, -2.621784821875001281 ) ) ;
#63839 = CARTESIAN_POINT ( 'NONE',  ( 5.437500000000001776, -2.886751345948125991, -5.000000000000000000 ) ) ;
#63840 = CARTESIAN_POINT ( 'NONE',  ( -2.121784821874996840, 14.92812500061459424, 33.67503911421598417 ) ) ;
#63841 = MECHANICAL_DESIGN_GEOMETRIC_PRESENTATION_REPRESENTATION (  '', ( #33226 ), #59152 ) ;
#63842 = CARTESIAN_POINT ( 'NONE',  ( 2.007161504316465894, 25.40607256557218108, 26.53021119236196412 ) ) ;
#63843 = CARTESIAN_POINT ( 'NONE',  ( 6.487499999999999822, 5.773502691896255534, 3.535250795749688894E-16 ) ) ;
#63844 = CARTESIAN_POINT ( 'NONE',  ( 15.98437500061451644, -2.746126346562642428, -4.756430356249999214 ) ) ;
#63845 = CARTESIAN_POINT ( 'NONE',  ( 19.49062500061451431, -3.027376345333614438, 5.243569643749998122 ) ) ;
#63846 = CARTESIAN_POINT ( 'NONE',  ( 12.66562500061451502, 3.027376345333611329, 5.243569643749999010 ) ) ;
#63847 = CARTESIAN_POINT ( 'NONE',  ( 27.12187500061451573, -4.119189519843968306, 2.378215178124996054 ) ) ;
#63848 = CARTESIAN_POINT ( 'NONE',  ( 8.334375000614516082, -4.541064518000419881, 2.621784821874995952 ) ) ;
#63849 = CARTESIAN_POINT ( 'NONE',  ( 26.28749999999999432, 5.773502691896255534, 3.535250795749688894E-16 ) ) ;
#63850 = CARTESIAN_POINT ( 'NONE',  ( 23.62500000122902932, 2.886751345948129099, -4.999999999999998224 ) ) ;
#63851 = CARTESIAN_POINT ( 'NONE',  ( 28.80000000000000071, -4.330127018922190985, -2.500000000000001332 ) ) ;
#63852 = CARTESIAN_POINT ( 'NONE',  ( 12.34687500061452070, -3.027376345333614438, 5.243569643749998122 ) ) ;
#63853 = CARTESIAN_POINT ( 'NONE',  ( 25.69687500061451502, 6.054752690667223547, 3.707466751127219781E-16 ) ) ;
#63854 = CARTESIAN_POINT ( 'NONE',  ( 28.14375000122903359, 5.773502691896255534, 3.535250795749688401E-16 ) ) ;
#63855 = DIRECTION ( 'NONE',  ( 0.000000000000000000, 0.000000000000000000, 1.000000000000000000 ) ) ;
#63856 = CARTESIAN_POINT ( 'NONE',  ( 19.43437500061451928, 4.541064518000418104, 2.621784821874999949 ) ) ;
#63857 = CARTESIAN_POINT ( 'NONE',  ( 12.64687500061451608, 6.054752690667223547, 3.707466751127219781E-16 ) ) ;
#63858 = CARTESIAN_POINT ( 'NONE',  ( 1.878215178125000495, 17.32812499938548356, 26.74683588394047007 ) ) ;
#63859 = CARTESIAN_POINT ( 'NONE',  ( 26.66250000000000142, 2.886751345948129099, -4.999999999999998224 ) ) ;
#63860 = CARTESIAN_POINT ( 'NONE',  ( 2.655984681222220721E-16, 20.40312499938548285, 25.66244784525396483 ) ) ;
#63861 = CARTESIAN_POINT ( 'NONE',  ( -4.243569643749997233, 12.69687500061451857, -27.54997392385601174 ) ) ;
#63862 = CARTESIAN_POINT ( 'NONE',  ( 26.89687500061451431, -2.746126346562642428, -4.756430356249999214 ) ) ;
#63863 = CARTESIAN_POINT ( 'NONE',  ( 14.50312500061451537, 0.000000000000000000, 5.243569643749999010 ) ) ;
#63864 = CARTESIAN_POINT ( 'NONE',  ( 4.537500000000000533, -2.886751345948125991, -5.000000000000000000 ) ) ;
#63865 = CARTESIAN_POINT ( 'NONE',  ( 25.23750000000000071, -2.886751345948153968, -4.999999999999952038 ) ) ;
#63866 = DIRECTION ( 'NONE',  ( -1.000000000000000000, -0.000000000000000000, -0.000000000000000000 ) ) ;
#63867 = CARTESIAN_POINT ( 'NONE',  ( 13.76250000000000107, 2.886751345948126879, 4.999999999999999112 ) ) ;
#63868 = CARTESIAN_POINT ( 'NONE',  ( -2.121784821874999949, 9.828125000614516438, 26.32496088578401938 ) ) ;
#63869 = CARTESIAN_POINT ( 'NONE',  ( 14.02500000122903323, -5.773502691896255534, -1.060575238724906372E-15 ) ) ;
#63870 = CARTESIAN_POINT ( 'NONE',  ( 23.82187500061451502, 3.027376345333613106, -5.243569643749998122 ) ) ;
#63871 = ORIENTED_EDGE ( 'NONE', *, *, #24336, .F. ) ;
#63872 = CARTESIAN_POINT ( 'NONE',  ( 19.56562500061451715, -6.054752690667223547, -1.112240025338166033E-15 ) ) ;
#63873 = CARTESIAN_POINT ( 'NONE',  ( 4.153125000614515727, 0.000000000000000000, 5.243569643749999010 ) ) ;
#63874 = CARTESIAN_POINT ( 'NONE',  ( 19.35937500061451644, 4.541064518000418104, -2.621784821874998173 ) ) ;
#63875 = CARTESIAN_POINT ( 'NONE',  ( 4.087500000000001243, -2.886751345948125991, -5.000000000000000000 ) ) ;
#63876 = CARTESIAN_POINT ( 'NONE',  ( 7.828125000614517326, -4.541064518000419881, 2.621784821874995952 ) ) ;
#63877 = CARTESIAN_POINT ( 'NONE',  ( 21.21562500061451573, 3.027376345333611329, 5.243569643749999010 ) ) ;
#63878 = CARTESIAN_POINT ( 'NONE',  ( 2.121784821874999061, 14.25312500061451715, 26.32496088578401583 ) ) ;
#63879 = CARTESIAN_POINT ( 'NONE',  ( 19.16250000122903430, 4.330127018922192761, -2.499999999999997780 ) ) ;
#63880 = CARTESIAN_POINT ( 'NONE',  ( 12.15937500061451892, 4.119189519843966529, -2.378215178124998275 ) ) ;
#63881 = CARTESIAN_POINT ( 'NONE',  ( 9.590625000614517504, -3.027376345333614438, 5.243569643749998122 ) ) ;
#63882 = CARTESIAN_POINT ( 'NONE',  ( 3.609375000614516882, 4.541064518000418104, -2.621784821874998173 ) ) ;
#63883 = CARTESIAN_POINT ( 'NONE',  ( 3.009375000614516793, -4.541064518000417216, -2.621784821875001281 ) ) ;
#63884 = CARTESIAN_POINT ( 'NONE',  ( 22.13437500061451502, 4.541064518000418104, 2.621784821874999949 ) ) ;
#63885 = CARTESIAN_POINT ( 'NONE',  ( 13.56562500061451892, 3.027376345333611329, 5.243569643749999010 ) ) ;
#63886 = CARTESIAN_POINT ( 'NONE',  ( 25.20000000122903216, -2.886751345948129988, 4.999999999999997335 ) ) ;
#63887 = EDGE_CURVE ( 'NONE', #60322, #4907, #20343, .T. ) ;
#63888 = CARTESIAN_POINT ( 'NONE',  ( 26.24062500061451431, -3.027376345333614438, 5.243569643749998122 ) ) ;
#63889 = CARTESIAN_POINT ( 'NONE',  ( 19.65937500061451360, -4.541064518000417216, -2.621784821875001281 ) ) ;
#63890 = CARTESIAN_POINT ( 'NONE',  ( 15.36562500061451608, 3.027376345333611329, 5.243569643749999010 ) ) ;
#63891 = CARTESIAN_POINT ( 'NONE',  ( -4.243569643749999898, 16.25937500061451857, 30.00000000000000000 ) ) ;
#63892 = ADVANCED_FACE ( 'NONE', ( #58610 ), #53820, .F. ) ;
#63893 = CARTESIAN_POINT ( 'NONE',  ( 21.14062500061451289, 6.054752690667223547, 3.707466751127219781E-16 ) ) ;
#63894 = CARTESIAN_POINT ( 'NONE',  ( 23.49375000122903501, -2.886751345948153968, -4.999999999999952038 ) ) ;
#63895 = ORIENTED_EDGE ( 'NONE', *, *, #60122, .F. ) ;
#63896 = CARTESIAN_POINT ( 'NONE',  ( 25.05000000000000071, 0.000000000000000000, 4.999999999999998224 ) ) ;
#63897 = CARTESIAN_POINT ( 'NONE',  ( 1.999999999999998668, 10.85000000000000142, -33.46410161513775705 ) ) ;
#63898 = CARTESIAN_POINT ( 'NONE',  ( 0.6522905807966048464, 20.75364847883808395, 33.69936292076899065 ) ) ;
#63899 = CARTESIAN_POINT ( 'NONE',  ( 25.75312500061451715, 0.000000000000000000, 5.243569643749999010 ) ) ;
#63900 = CARTESIAN_POINT ( 'NONE',  ( 6.740625000614516082, 6.054752690667223547, 3.707466751127219781E-16 ) ) ;
#63901 = CARTESIAN_POINT ( 'NONE',  ( 22.83750000122903501, 4.330127018922191873, 2.499999999999999556 ) ) ;
#63902 = CARTESIAN_POINT ( 'NONE',  ( 27.47812500061451502, 4.541064518000418104, 2.621784821874999949 ) ) ;
#63904 = CARTESIAN_POINT ( 'NONE',  ( 24.29999999999999716, -4.330127018922190985, -2.500000000000001332 ) ) ;
#63903 =( GEOMETRIC_REPRESENTATION_CONTEXT ( 3 ) GLOBAL_UNCERTAINTY_ASSIGNED_CONTEXT ( ( #3340 ) ) GLOBAL_UNIT_ASSIGNED_CONTEXT ( ( #12739, #3861, #71824 ) ) REPRESENTATION_CONTEXT ( 'NONE', 'WORKASPACE' ) );
#63905 = CARTESIAN_POINT ( 'NONE',  ( -1.999999999999997113, 16.58750000122903501, -26.53589838486224295 ) ) ;
#63906 = EDGE_CURVE ( 'NONE', #29785, #18820, #11276, .T. ) ;
#63907 =( BOUNDED_CURVE ( )  B_SPLINE_CURVE ( 3, ( #22060, #67148, #23139, #55323 ),
 .UNSPECIFIED., .F., .F. ) 
 B_SPLINE_CURVE_WITH_KNOTS ( ( 4, 4 ),
 ( 5.853026561459537369, 5.913091855019096066 ),
 .UNSPECIFIED. ) 
 CURVE ( )  GEOMETRIC_REPRESENTATION_ITEM ( )  RATIONAL_B_SPLINE_CURVE ( ( 1.000000000000000000, 0.9996993693065544528, 0.9996993693065544528, 1.000000000000000000 ) ) 
 REPRESENTATION_ITEM ( '' )  );
#63908 = CARTESIAN_POINT ( 'NONE',  ( 29.31562500061451715, 3.027376345333611329, 5.243569643749999010 ) ) ;
#63909 = CARTESIAN_POINT ( 'NONE',  ( 11.69062500061451360, 6.054752690667223547, 3.707466751127219781E-16 ) ) ;
#63910 = VERTEX_POINT ( 'NONE', #8379 ) ;
#63911 = CARTESIAN_POINT ( 'NONE',  ( 24.85312500061451502, 0.000000000000000000, 5.243569643749999010 ) ) ;
#63912 = CARTESIAN_POINT ( 'NONE',  ( 6.665625000614515905, 3.027376345333613106, -5.243569643749998122 ) ) ;
#63913 = UNCERTAINTY_MEASURE_WITH_UNIT (LENGTH_MEASURE( 1.000000000000000082E-05 ), #46737, 'distance_accuracy_value', 'NONE');
#63914 = CARTESIAN_POINT ( 'NONE',  ( 3.778125000614519280, -4.541064518000419881, 2.621784821874995952 ) ) ;
#63915 = CARTESIAN_POINT ( 'NONE',  ( 15.45937500061451608, 0.000000000000000000, 4.756430356249998326 ) ) ;
#63916 = ADVANCED_FACE ( 'NONE', ( #14643 ), #48644, .T. ) ;
#63917 = CARTESIAN_POINT ( 'NONE',  ( 13.40625000122903288, 0.000000000000000000, 4.999999999999998224 ) ) ;
#63918 = CARTESIAN_POINT ( 'NONE',  ( 13.42499999999999893, -4.330127018922194537, 2.499999999999995559 ) ) ;
#63919 = CARTESIAN_POINT ( 'NONE',  ( 12.57187500061451857, 3.027376345333613106, -5.243569643749998122 ) ) ;
#63920 = CARTESIAN_POINT ( 'NONE',  ( 8.587500001229035007, -4.330127018922194537, 2.499999999999995559 ) ) ;
#63921 = CARTESIAN_POINT ( 'NONE',  ( 17.29687500061451999, -3.027376345333614438, 5.243569643749998122 ) ) ;
#63922 = CARTESIAN_POINT ( 'NONE',  ( 18.07499999999999929, 6.123233995736764310E-16, -4.999999999999998224 ) ) ;
#63923 = CARTESIAN_POINT ( 'NONE',  ( 7.884375000614517681, -4.541064518000419881, 2.621784821874995952 ) ) ;
#63924 = CARTESIAN_POINT ( 'NONE',  ( 2.121784821874999061, 10.65312500061451750, -33.67503911421598417 ) ) ;
#63925 = FACE_OUTER_BOUND ( 'NONE', #22225, .T. ) ;
#63926 = CARTESIAN_POINT ( 'NONE',  ( 22.47187500061451360, 4.119189519843966529, 2.378215178124999607 ) ) ;
#63927 = EDGE_LOOP ( 'NONE', ( #32847, #61601 ) ) ;
#63928 = CARTESIAN_POINT ( 'NONE',  ( 23.84062500061451928, 6.054752690667223547, 3.707466751127219781E-16 ) ) ;
#63929 = CARTESIAN_POINT ( 'NONE',  ( 1.071796769724479237, 20.63615380933863364, 25.99999999999999645 ) ) ;
#63930 = CARTESIAN_POINT ( 'NONE',  ( 26.89687500061451431, -3.027376345333610441, -5.243569643749999898 ) ) ;
#63931 = CARTESIAN_POINT ( 'NONE',  ( 29.22187500061451715, 3.027376345333613106, -5.243569643749998122 ) ) ;
#63932 = CARTESIAN_POINT ( 'NONE',  ( 22.23750000000000071, 5.773502691896255534, 3.535250795749688894E-16 ) ) ;
#63933 = CARTESIAN_POINT ( 'NONE',  ( 7.753125000614518036, 0.000000000000000000, 5.243569643749999010 ) ) ;
#63934 = CARTESIAN_POINT ( 'NONE',  ( 23.67187500061451289, 5.824947211148865298E-16, -4.756430356249998326 ) ) ;
#63935 = CARTESIAN_POINT ( 'NONE',  ( 16.50937500061451502, -4.541064518000417216, -2.621784821875001281 ) ) ;
#63936 = CARTESIAN_POINT ( 'NONE',  ( 8.934375000614517504, 5.492252693125287522, 3.363034840372157021E-16 ) ) ;
#63937 = CARTESIAN_POINT ( 'NONE',  ( 3.103125000614517237, 4.541064518000418104, -2.621784821874998173 ) ) ;
#63938 = CARTESIAN_POINT ( 'NONE',  ( 7.621875000614519280, 3.027376345333613106, -5.243569643749998122 ) ) ;
#63939 = VERTEX_POINT ( 'NONE', #59708 ) ;
#63940 = CARTESIAN_POINT ( 'NONE',  ( 19.88437500061451857, 4.541064518000418104, 2.621784821874999949 ) ) ;
#63941 = CARTESIAN_POINT ( 'NONE',  ( 9.806250001229033231, 0.000000000000000000, 4.999999999999998224 ) ) ;
#63942 = CARTESIAN_POINT ( 'NONE',  ( 26.81250000000000000, 2.886751345948126879, 4.999999999999999112 ) ) ;
#63943 = CARTESIAN_POINT ( 'NONE',  ( 26.48437500061451644, 6.421520780324663323E-16, -5.243569643749999010 ) ) ;
#63944 = LINE ( 'NONE', #23694, #19508 ) ;
#63945 = CARTESIAN_POINT ( 'NONE',  ( 17.81250000000000355, 2.886751345948182834, 4.999999999999902300 ) ) ;
#63946 = ORIENTED_EDGE ( 'NONE', *, *, #34637, .T. ) ;
#63947 = CARTESIAN_POINT ( 'NONE',  ( 10.20000000000000107, 0.000000000000000000, 4.999999999999998224 ) ) ;
#63948 = CARTESIAN_POINT ( 'NONE',  ( 12.79687500061451466, -4.119189519843965641, -2.378215178125001383 ) ) ;
#63949 = CARTESIAN_POINT ( 'NONE',  ( 21.44062500061452070, -3.027376345333610441, -5.243569643749999898 ) ) ;
#63950 = CARTESIAN_POINT ( 'NONE',  ( 11.28749999999999787, -2.886751345948125991, -5.000000000000000000 ) ) ;
#63951 = CARTESIAN_POINT ( 'NONE',  ( 8.662500001229034297, -4.330127018922190985, -2.500000000000001332 ) ) ;
#63952 = CARTESIAN_POINT ( 'NONE',  ( 5.728125000614515905, 6.421520780324663323E-16, -5.243569643749999010 ) ) ;
#63953 =( BOUNDED_CURVE ( )  B_SPLINE_CURVE ( 2, ( #9540, #4011, #31342, #53883, #26535, #49074, #3275 ),
 .UNSPECIFIED., .F., .F. ) 
 B_SPLINE_CURVE_WITH_KNOTS ( ( 3, 2, 2, 3 ),
 ( 0.5999999999999999778, 0.6033333333333334991, 0.6066666666666667984, 0.6100000000000002087 ),
 .UNSPECIFIED. ) 
 CURVE ( )  GEOMETRIC_REPRESENTATION_ITEM ( )  RATIONAL_B_SPLINE_CURVE ( ( 1.000000000000000000, 0.8660254037844387076, 1.000000000000000000, 0.8660254037844387076, 1.000000000000000000, 0.8660254037844298258, 1.000000000000008882 ) ) 
 REPRESENTATION_ITEM ( '' )  );
#63954 = CARTESIAN_POINT ( 'NONE',  ( 22.57499999999999929, 6.123233995736764310E-16, -4.999999999999998224 ) ) ;
#63955 = CARTESIAN_POINT ( 'NONE',  ( 20.61562500061451431, 3.027376345333613106, -5.243569643749998122 ) ) ;
#63956 = CARTESIAN_POINT ( 'NONE',  ( 23.51249999999999929, 2.886751345948101122, -5.000000000000046185 ) ) ;
#63957 = AXIS2_PLACEMENT_3D ( 'NONE', #8354, #14988, #64131 ) ;
#63958 = CARTESIAN_POINT ( 'NONE',  ( 25.50000000122903288, 5.773502691896255534, 3.535250795749688894E-16 ) ) ;
#63959 = CARTESIAN_POINT ( 'NONE',  ( 3.756430356249998770, 19.35312499938548214, 32.16877607737301759 ) ) ;
#63960 = CARTESIAN_POINT ( 'NONE',  ( 5.175000000000002487, 4.330127018922191873, 2.499999999999999556 ) ) ;
#63961 = VERTEX_POINT ( 'NONE', #9115 ) ;
#63962 = CARTESIAN_POINT ( 'NONE',  ( 18.47812500061451857, 4.541064518000418104, 2.621784821874999949 ) ) ;
#63963 = CARTESIAN_POINT ( 'NONE',  ( 27.29062500061451502, -3.027376345333610441, -5.243569643749999898 ) ) ;
#63964 = CARTESIAN_POINT ( 'NONE',  ( 26.85937500061451644, -4.541064518000417216, -2.621784821875001281 ) ) ;
#63965 = CARTESIAN_POINT ( 'NONE',  ( 14.27812500061451573, 6.421520780324663323E-16, -5.243569643749999010 ) ) ;
#63966 = FACE_OUTER_BOUND ( 'NONE', #66108, .T. ) ;
#63967 = CARTESIAN_POINT ( 'NONE',  ( 25.91250000122903074, 4.330127018922192761, -2.499999999999997780 ) ) ;
#63968 = CARTESIAN_POINT ( 'NONE',  ( 18.90937500061451360, 4.119189519843966529, -2.378215178124998275 ) ) ;
#63969 = CARTESIAN_POINT ( 'NONE',  ( 17.31562500061451715, -6.054752690667223547, -1.112240025338166033E-15 ) ) ;
#63970 = CARTESIAN_POINT ( 'NONE',  ( 28.48125000122902861, 6.123233995736764310E-16, -4.999999999999998224 ) ) ;
#63971 = CARTESIAN_POINT ( 'NONE',  ( 28.54687500061451644, -3.027376345333614438, 5.243569643749998122 ) ) ;
#63972 = CARTESIAN_POINT ( 'NONE',  ( 10.13437500061451679, -4.541064518000419881, 2.621784821874995952 ) ) ;
#63973 = CARTESIAN_POINT ( 'NONE',  ( 9.759375000614516793, -4.541064518000417216, -2.621784821875001281 ) ) ;
#63974 = CARTESIAN_POINT ( 'NONE',  ( 17.97187500061451715, 3.027376345333613106, -5.243569643749998122 ) ) ;
#63975 = ORIENTED_EDGE ( 'NONE', *, *, #48303, .T. ) ;
#63976 = CARTESIAN_POINT ( 'NONE',  ( -5.918438294331348715, 8.060677219855273634, 28.99413606184803527 ) ) ;
#63977 = CARTESIAN_POINT ( 'NONE',  ( 21.51562500061451644, 3.027376345333613106, -5.243569643749998122 ) ) ;
#63978 = ADVANCED_FACE ( 'NONE', ( #3583 ), #31653, .T. ) ;
#63979 = CARTESIAN_POINT ( 'NONE',  ( 18.57187500061451857, 3.027376345333611329, 5.243569643749999010 ) ) ;
#63980 = CARTESIAN_POINT ( 'NONE',  ( 22.26562500061451644, -6.054752690667223547, -1.112240025338166033E-15 ) ) ;
#63981 = CARTESIAN_POINT ( 'NONE',  ( -2.000000000000000000, 15.42500000000000071, 26.53589838486224650 ) ) ;
#63982 = CARTESIAN_POINT ( 'NONE',  ( 29.65312500061451573, 4.541064518000418104, -2.621784821874998173 ) ) ;
#63983 = CARTESIAN_POINT ( 'NONE',  ( 9.412500001229034297, 0.000000000000000000, 4.999999999999998224 ) ) ;
#63984 = VERTEX_POINT ( 'NONE', #13183 ) ;
#63985 = CARTESIAN_POINT ( 'NONE',  ( 3.937500001229034208, 4.330127018922191873, 2.499999999999999556 ) ) ;
#63986 = CARTESIAN_POINT ( 'NONE',  ( -3.999999999999999556, 19.96250000000000213, -32.30940107675850470 ) ) ;
#63987 = CARTESIAN_POINT ( 'NONE',  ( 25.08750000122903145, 4.330127018922191873, 2.499999999999999556 ) ) ;
#63988 = CARTESIAN_POINT ( 'NONE',  ( 3.756430356250000102, 12.75312499938548427, 30.00000000000000000 ) ) ;
#63989 = ADVANCED_FACE ( 'NONE', ( #35722 ), #7648, .T. ) ;
#63990 = CARTESIAN_POINT ( 'NONE',  ( 9.309375000614517504, -4.541064518000417216, -2.621784821875001281 ) ) ;
#63991 = CARTESIAN_POINT ( 'NONE',  ( 30.00000000000000000, 0.000000000000000000, 0.000000000000000000 ) ) ;
#63992 = CARTESIAN_POINT ( 'NONE',  ( 15.70312500061451644, 4.541064518000418104, -2.621784821874998173 ) ) ;
#63993 = CARTESIAN_POINT ( 'NONE',  ( 9.834375000614517859, 6.421520780324663323E-16, -5.243569643749999010 ) ) ;
#63994 = CARTESIAN_POINT ( 'NONE',  ( 28.72500000122903074, 2.886751345948126879, 4.999999999999999112 ) ) ;
#63995 = CARTESIAN_POINT ( 'NONE',  ( 20.37187500061451573, 3.027376345333611329, 5.243569643749999010 ) ) ;
#63996 = CARTESIAN_POINT ( 'NONE',  ( 6.684375000614518392, 6.421520780324663323E-16, -5.243569643749999010 ) ) ;
#63997 = CARTESIAN_POINT ( 'NONE',  ( 4.818692141996693046, -1.334243621178544226, 4.818692141997074074 ) ) ;
#63998 = ADVANCED_FACE ( 'NONE', ( #16107 ), #27937, .F. ) ;
#63999 = CARTESIAN_POINT ( 'NONE',  ( 7.753125000614518036, 0.000000000000000000, 5.243569643749999010 ) ) ;
#64000 = CARTESIAN_POINT ( 'NONE',  ( 17.27812500061451217, -4.541064518000419881, 2.621784821874995952 ) ) ;
#64001 = VERTEX_POINT ( 'NONE', #49379 ) ;
#64002 = CARTESIAN_POINT ( 'NONE',  ( 15.92812500061451608, -4.541064518000419881, 2.621784821874995952 ) ) ;
#64003 = CARTESIAN_POINT ( 'NONE',  ( 9.928125000614517859, 4.541064518000418104, 2.621784821874999949 ) ) ;
#64004 = CARTESIAN_POINT ( 'NONE',  ( 22.99687500061451573, 5.492252693125287522, 3.363034840372157021E-16 ) ) ;
#64005 = CARTESIAN_POINT ( 'NONE',  ( 10.87500000000000000, 6.123233995736764310E-16, -4.999999999999998224 ) ) ;
#64006 = CARTESIAN_POINT ( 'NONE',  ( 6.525000001229033231, 2.886751345948129099, -4.999999999999998224 ) ) ;
#64007 = CARTESIAN_POINT ( 'NONE',  ( 15.34687500061451537, 6.054752690667223547, 3.707466751127219781E-16 ) ) ;
#64008 = AXIS2_PLACEMENT_3D ( 'NONE', #25324, #47869, #70398 ) ;
#64009 = CARTESIAN_POINT ( 'NONE',  ( 16.83750000122903145, 6.123233995736764310E-16, -4.999999999999998224 ) ) ;
#64010 = CARTESIAN_POINT ( 'NONE',  ( 23.73749999999999716, -2.886751345948129988, 4.999999999999997335 ) ) ;
#64011 = CARTESIAN_POINT ( 'NONE',  ( -4.243569643749999898, 19.35312500061451857, -30.00000000000000000 ) ) ;
#64012 = CARTESIAN_POINT ( 'NONE',  ( 16.35000000122903430, -2.886751345948126435, -5.000000000000000000 ) ) ;
#64013 = CARTESIAN_POINT ( 'NONE',  ( 30.00000000000000000, 0.000000000000000000, 0.000000000000000000 ) ) ;
#64014 = ADVANCED_FACE ( 'NONE', ( #55643 ), #72271, .F. ) ;
#64015 = CARTESIAN_POINT ( 'NONE',  ( 1.626862140677534273E-15, 10.77500000122903323, -26.00000000000000355 ) ) ;
#64016 = CYLINDRICAL_SURFACE ( 'NONE', #26699, 4.999999999999998224 ) ;
#64017 = CARTESIAN_POINT ( 'NONE',  ( 17.78437500061451715, -4.541064518000419881, 2.621784821874995952 ) ) ;
#64018 = FACE_OUTER_BOUND ( 'NONE', #71992, .T. ) ;
#64019 = CARTESIAN_POINT ( 'NONE',  ( 13.79062500061451502, -3.027376345333610441, -5.243569643749999898 ) ) ;
#64020 = CARTESIAN_POINT ( 'NONE',  ( 10.44375000122903074, -2.886751345948125991, -5.000000000000000000 ) ) ;
#64021 = CARTESIAN_POINT ( 'NONE',  ( 23.25937500061451857, -4.541064518000417216, -2.621784821875001281 ) ) ;
#64022 = CARTESIAN_POINT ( 'NONE',  ( 16.09687500061451715, 4.119189519843966529, -2.378215178124998275 ) ) ;
#64023 = CARTESIAN_POINT ( 'NONE',  ( 10.56562500061451715, -6.054752690667223547, -1.112240025338166033E-15 ) ) ;
#64024 = CARTESIAN_POINT ( 'NONE',  ( 15.68437500061451573, 6.421520780324663323E-16, -5.243569643749999010 ) ) ;
#64025 = EDGE_LOOP ( 'NONE', ( #35822, #35981, #45091, #9732 ) ) ;
#64026 = CARTESIAN_POINT ( 'NONE',  ( 26.07187500061451857, 3.027376345333613106, -5.243569643749998122 ) ) ;
#64027 = CARTESIAN_POINT ( 'NONE',  ( 27.66562500061451146, -6.054752690667223547, -1.112240025338166033E-15 ) ) ;
#64028 = CARTESIAN_POINT ( 'NONE',  ( 18.36562500061451431, 3.027376345333613106, -5.243569643749998122 ) ) ;
#64029 = CARTESIAN_POINT ( 'NONE',  ( 18.97499999999999787, 6.123233995736764310E-16, -4.999999999999998224 ) ) ;
#64030 = CARTESIAN_POINT ( 'NONE',  ( 45.00000000000000000, -2.499999999999999556, 3.499999999999999556 ) ) ;
#64031 = CARTESIAN_POINT ( 'NONE',  ( 8.737500000000002487, 5.773502691896255534, 3.535250795749688894E-16 ) ) ;
#64032 = CARTESIAN_POINT ( 'NONE',  ( 19.08750000122903145, 6.123233995736764310E-16, -4.999999999999998224 ) ) ;
#64033 = CARTESIAN_POINT ( 'NONE',  ( 1.626862140677534273E-15, 10.21250000000000036, 34.00000000000000000 ) ) ;
#64034 = CARTESIAN_POINT ( 'NONE',  ( 9.759375000614516793, 2.746126346562645981, -4.756430356249997438 ) ) ;
#64035 = ORIENTED_EDGE ( 'NONE', *, *, #44978, .T. ) ;
#64036 = CARTESIAN_POINT ( 'NONE',  ( 16.76249999999999929, 2.886751345948129099, -4.999999999999998224 ) ) ;
#64037 = CARTESIAN_POINT ( 'NONE',  ( 22.12500000000000000, 6.123233995736764310E-16, -4.999999999999998224 ) ) ;
#64038 = CARTESIAN_POINT ( 'NONE',  ( 18.83437500061451431, 6.421520780324663323E-16, -5.243569643749999010 ) ) ;
#64039 = CARTESIAN_POINT ( 'NONE',  ( 14.24062500061451608, -3.027376345333610441, -5.243569643749999898 ) ) ;
#64040 = ORIENTED_EDGE ( 'NONE', *, *, #35090, .F. ) ;
#64041 = CARTESIAN_POINT ( 'NONE',  ( 28.53749999999999787, 5.773502691896255534, 3.535250795749688401E-16 ) ) ;
#64042 = CARTESIAN_POINT ( 'NONE',  ( 6.065625000614516260, -6.054752690667223547, -1.112240025338166033E-15 ) ) ;
#64043 = CARTESIAN_POINT ( 'NONE',  ( 34.99999999999999289, -2.499999999999999556, 3.499999999999999556 ) ) ;
#64044 = CARTESIAN_POINT ( 'NONE',  ( 12.82499999999999929, 4.330127018922191873, 2.499999999999999556 ) ) ;
#64045 = CARTESIAN_POINT ( 'NONE',  ( 27.72187500061451715, 5.824947211148865298E-16, -4.756430356249998326 ) ) ;
#64046 = CARTESIAN_POINT ( 'NONE',  ( -3.000416591977282496E-16, 15.64062500061451644, 25.09994784771203058 ) ) ;
#64047 = CARTESIAN_POINT ( 'NONE',  ( 28.64062500061451289, -3.027376345333610441, -5.243569643749999898 ) ) ;
#64048 = CARTESIAN_POINT ( 'NONE',  ( 8.474999999999999645, -4.330127018922194537, 2.499999999999995559 ) ) ;
#64049 = CARTESIAN_POINT ( 'NONE',  ( 2.655984681222220721E-16, 16.80312499938548143, 25.66244784525396483 ) ) ;
#64050 = CARTESIAN_POINT ( 'NONE',  ( 24.68437500061451573, 6.421520780324663323E-16, -5.243569643749999010 ) ) ;
#64051 = ORIENTED_EDGE ( 'NONE', *, *, #50505, .F. ) ;
#64052 = CARTESIAN_POINT ( 'NONE',  ( 22.56562500061451715, 3.027376345333611329, 5.243569643749999010 ) ) ;
#64053 = CARTESIAN_POINT ( 'NONE',  ( 24.00937500061451502, 0.000000000000000000, 5.243569643749999010 ) ) ;
#64054 = CARTESIAN_POINT ( 'NONE',  ( 4.243569643749999010, 15.56562500061459531, -32.45002607614398471 ) ) ;
#64055 = CARTESIAN_POINT ( 'NONE',  ( 6.440625000614517148, -3.027376345333614438, 5.243569643749998122 ) ) ;
#64056 = CARTESIAN_POINT ( 'NONE',  ( 27.60937500061451644, 0.000000000000000000, 4.756430356249998326 ) ) ;
#64057 = CARTESIAN_POINT ( 'NONE',  ( 23.84062500061451573, 6.054752690667223547, 3.707466751127219781E-16 ) ) ;
#64058 = CARTESIAN_POINT ( 'NONE',  ( 26.85937500061450933, 2.746126346562645981, -4.756430356249997438 ) ) ;
#64059 = CARTESIAN_POINT ( 'NONE',  ( 9.984375000614518214, 4.119189519843966529, 2.378215178124999607 ) ) ;
#64060 = CARTESIAN_POINT ( 'NONE',  ( 16.05937500061451573, -4.541064518000417216, -2.621784821875001281 ) ) ;
#64061 = CARTESIAN_POINT ( 'NONE',  ( 27.04687500061451644, 6.054752690667223547, 3.707466751127219781E-16 ) ) ;
#64062 = CARTESIAN_POINT ( 'NONE',  ( -3.000416591977282496E-16, 14.34687500061451715, 25.09994784771203058 ) ) ;
#64063 = CARTESIAN_POINT ( 'NONE',  ( 6.328125000614515550, 4.541064518000418104, 2.621784821874999949 ) ) ;
#64064 = DIRECTION ( 'NONE',  ( -1.000000000000000000, -0.000000000000000000, -0.000000000000000000 ) ) ;
#64065 = CARTESIAN_POINT ( 'NONE',  ( 29.12812500061451715, 6.421520780324663323E-16, -5.243569643749999010 ) ) ;
#64066 = CARTESIAN_POINT ( 'NONE',  ( 45.00000000000000000, 0.000000000000000000, 0.000000000000000000 ) ) ;
#64067 = CARTESIAN_POINT ( 'NONE',  ( 4.865625000614517859, 3.027376345333613106, -5.243569643749998122 ) ) ;
#64068 = CARTESIAN_POINT ( 'NONE',  ( 8.634375000614518569, 4.541064518000418104, 2.621784821874999949 ) ) ;
#64069 = CARTESIAN_POINT ( 'NONE',  ( 15.97500000122903430, 2.886751345948129099, -4.999999999999998224 ) ) ;
#64070 = CARTESIAN_POINT ( 'NONE',  ( 4.171875000614517326, 3.027376345333611329, 5.243569643749999010 ) ) ;
#64071 = CARTESIAN_POINT ( 'NONE',  ( 7.153125000614518392, 4.541064518000418104, -2.621784821874998173 ) ) ;
#64072 = LINE ( 'NONE', #25657, #26896 ) ;
#64073 = CARTESIAN_POINT ( 'NONE',  ( 20.86875000122903145, 2.886751345948129099, -4.999999999999998224 ) ) ;
#64074 = CARTESIAN_POINT ( 'NONE',  ( 17.52187500061451431, 3.027376345333613106, -5.243569643749998122 ) ) ;
#64075 = CARTESIAN_POINT ( 'NONE',  ( 22.64999999999999858, 4.330127018922192761, -2.499999999999997780 ) ) ;
#64076 = ORIENTED_EDGE ( 'NONE', *, *, #57166, .F. ) ;
#64077 = CARTESIAN_POINT ( 'NONE',  ( 25.64062500061451644, 6.054752690667223547, 3.707466751127219781E-16 ) ) ;
#64078 = CARTESIAN_POINT ( 'NONE',  ( 9.928125000614517859, 4.541064518000418104, 2.621784821874999949 ) ) ;
#64079 = CARTESIAN_POINT ( 'NONE',  ( 25.95937500061451431, -4.541064518000417216, -2.621784821875001281 ) ) ;
#64080 = CARTESIAN_POINT ( 'NONE',  ( 10.86562500061451431, 3.027376345333611329, 5.243569643749999010 ) ) ;
#64081 = CARTESIAN_POINT ( 'NONE',  ( 10.87500000000000000, 6.123233995736764310E-16, -4.999999999999998224 ) ) ;
#64082 = CARTESIAN_POINT ( 'NONE',  ( 9.675000001229035362, 2.886751345948129099, -4.999999999999998224 ) ) ;
#64083 = EDGE_CURVE ( 'NONE', #57497, #71040, #39542, .T. ) ;
#64084 = CARTESIAN_POINT ( 'NONE',  ( 24.32812500061451289, 4.541064518000418104, 2.621784821874999949 ) ) ;
#64085 = CARTESIAN_POINT ( 'NONE',  ( 4.243569643749999010, 10.16562500061451857, -32.45002607614398471 ) ) ;
#64086 = CARTESIAN_POINT ( 'NONE',  ( 13.87500000122903465, 2.886751345948126879, 4.999999999999999112 ) ) ;
#64087 = CARTESIAN_POINT ( 'NONE',  ( 21.25312500061451715, 0.000000000000000000, 5.243569643749999010 ) ) ;
#64088 = CARTESIAN_POINT ( 'NONE',  ( 18.10312500061451502, 0.000000000000000000, 5.243569643749999010 ) ) ;
#64089 = CARTESIAN_POINT ( 'NONE',  ( 5.034375000614519813, 4.541064518000418104, 2.621784821874999949 ) ) ;
#64090 = CARTESIAN_POINT ( 'NONE',  ( 18.67500000000000071, 4.330127018922191873, 2.499999999999999556 ) ) ;
#64091 = CARTESIAN_POINT ( 'NONE',  ( 13.57500000122903572, -5.773502691896255534, -1.060575238724906372E-15 ) ) ;
#64092 = CARTESIAN_POINT ( 'NONE',  ( 10.79062500061451679, 6.054752690667223547, 3.707466751127219781E-16 ) ) ;
#64093 = CARTESIAN_POINT ( 'NONE',  ( 13.60312500061451679, 0.000000000000000000, 5.243569643749999010 ) ) ;
#64094 = CARTESIAN_POINT ( 'NONE',  ( 26.21250000122903501, -4.330127018922190985, -2.500000000000001332 ) ) ;
#64095 = CARTESIAN_POINT ( 'NONE',  ( 20.97187500061451715, -6.054752690667223547, -1.112240025338166033E-15 ) ) ;
#64096 = CARTESIAN_POINT ( 'NONE',  ( 22.09687500061451715, 6.054752690667223547, 3.707466751127219781E-16 ) ) ;
#64097 = CARTESIAN_POINT ( 'NONE',  ( 4.809916128174254624, -1.365542690628744449, -5.062639209831853115 ) ) ;
#64098 = CARTESIAN_POINT ( 'NONE',  ( 6.787500001229032520, -4.330127018922194537, 2.499999999999995559 ) ) ;
#64099 = CARTESIAN_POINT ( 'NONE',  ( 6.646875000614518747, -3.027376345333610441, -5.243569643749999898 ) ) ;
#64100 = CARTESIAN_POINT ( 'NONE',  ( 26.67187500061451644, 3.027376345333611329, 5.243569643749999010 ) ) ;
#64101 =( BOUNDED_CURVE ( )  B_SPLINE_CURVE ( 2, ( #18987, #37090, #35633, #65164, #41195, #41549, #13095, #58154, #7559 ),
 .UNSPECIFIED., .F., .F. ) 
 B_SPLINE_CURVE_WITH_KNOTS ( ( 3, 2, 2, 2, 3 ),
 ( 0.5972222222222222099, 0.6018518518518518601, 0.6111111111111111605, 0.6203703703703703498, 0.6250000000000000000 ),
 .UNSPECIFIED. ) 
 CURVE ( )  GEOMETRIC_REPRESENTATION_ITEM ( )  RATIONAL_B_SPLINE_CURVE ( ( 0.9330127018922194093, 0.9330127018922194093, 1.000000000000000000, 0.8660254037844387076, 1.000000000000000000, 0.8660254037844387076, 1.000000000000000000, 0.9330127018922194093, 0.9330127018922194093 ) ) 
 REPRESENTATION_ITEM ( '' )  );
#64102 = CARTESIAN_POINT ( 'NONE',  ( 3.684375000614518836, 4.541064518000418104, 2.621784821874999949 ) ) ;
#64103 = CARTESIAN_POINT ( 'NONE',  ( 20.72812500061451502, 4.541064518000418104, 2.621784821874999949 ) ) ;
#64104 = CARTESIAN_POINT ( 'NONE',  ( 26.37187500061451217, -6.054752690667223547, -1.112240025338166033E-15 ) ) ;
#64105 = CARTESIAN_POINT ( 'NONE',  ( -3.756430356249999214, 16.99062499938548498, 27.83122392262697176 ) ) ;
#64106 = CARTESIAN_POINT ( 'NONE',  ( 3.282867099560692559, -3.771354186041921075, 3.570299421950303032 ) ) ;
#64107 = FACE_OUTER_BOUND ( 'NONE', #40792, .T. ) ;
#64108 = CARTESIAN_POINT ( 'NONE',  ( 7.209375000614519635, 4.541064518000418104, -2.621784821874998173 ) ) ;
#64109 = CARTESIAN_POINT ( 'NONE',  ( 17.80312500061451786, -4.541064518000417216, -2.621784821875001281 ) ) ;
#64110 = VERTEX_POINT ( 'NONE', #5038 ) ;
#64111 = CARTESIAN_POINT ( 'NONE',  ( 23.02499999999999858, 6.123233995736764310E-16, -4.999999999999998224 ) ) ;
#64112 = CARTESIAN_POINT ( 'NONE',  ( 26.50312500061451360, 4.541064518000418104, -2.621784821874998173 ) ) ;
#64113 = CARTESIAN_POINT ( 'NONE',  ( 4.734375000614518214, -4.541064518000419881, 2.621784821874995952 ) ) ;
#64114 = CARTESIAN_POINT ( 'NONE',  ( 4.652363956030752590, 1.832484597013495531, 4.879388851549410155 ) ) ;
#64115 = EDGE_CURVE ( 'NONE', #6077, #38121, #16864, .T. ) ;
#64116 = CARTESIAN_POINT ( 'NONE',  ( 4.898587196589412829E-16, 27.50000000000000000, 34.00000000000000000 ) ) ;
#64117 = CARTESIAN_POINT ( 'NONE',  ( 16.80000000000000071, 4.330127018922192761, -2.499999999999997780 ) ) ;
#64118 = CARTESIAN_POINT ( 'NONE',  ( 22.00312500061451360, 4.541064518000418104, -2.621784821874998173 ) ) ;
#64119 = EDGE_LOOP ( 'NONE', ( #63320, #49762, #28880, #54599 ) ) ;
#64120 = CARTESIAN_POINT ( 'NONE',  ( 24.29999999999999716, -4.330127018922190985, -2.500000000000001332 ) ) ;
#64121 = CARTESIAN_POINT ( 'NONE',  ( 25.32187500061451857, 3.027376345333611329, 5.243569643749999010 ) ) ;
#64122 = ORIENTED_EDGE ( 'NONE', *, *, #57411, .T. ) ;
#64123 = DIRECTION ( 'NONE',  ( 0.000000000000000000, 0.000000000000000000, 1.000000000000000000 ) ) ;
#64124 = CARTESIAN_POINT ( 'NONE',  ( 13.94062500061451892, 6.054752690667223547, 3.707466751127219781E-16 ) ) ;
#64125 = CARTESIAN_POINT ( 'NONE',  ( 4.790625000614518569, -3.027376345333610441, -5.243569643749999898 ) ) ;
#64126 = CARTESIAN_POINT ( 'NONE',  ( 17.40937500061451360, 2.746126346562645981, -4.756430356249997438 ) ) ;
#64127 = CARTESIAN_POINT ( 'NONE',  ( 29.05312500061451431, -4.541064518000417216, -2.621784821875001281 ) ) ;
#64128 = CARTESIAN_POINT ( 'NONE',  ( 15.11250000122903359, 4.330127018922192761, -2.499999999999997780 ) ) ;
#64129 = CARTESIAN_POINT ( 'NONE',  ( 20.10000000000000142, 0.000000000000000000, 4.999999999999998224 ) ) ;
#64130 = CARTESIAN_POINT ( 'NONE',  ( 25.53750000000000142, -2.886751345948129988, 4.999999999999997335 ) ) ;
#64131 = DIRECTION ( 'NONE',  ( 0.000000000000000000, 0.000000000000000000, -1.000000000000000000 ) ) ;
#64132 = CARTESIAN_POINT ( 'NONE',  ( 8.634375000614518569, 4.541064518000418104, 2.621784821874999949 ) ) ;
#64133 = CARTESIAN_POINT ( 'NONE',  ( 19.54687500061451644, -3.027376345333614438, 5.243569643749998122 ) ) ;
#64134 = CARTESIAN_POINT ( 'NONE',  ( 4.000000000000000000, 11.30000000122903536, 32.30940107675849760 ) ) ;
#64135 = VERTEX_POINT ( 'NONE', #21648 ) ;
#64136 = CARTESIAN_POINT ( 'NONE',  ( 28.00312500061451715, 0.000000000000000000, 5.243569643749999010 ) ) ;
#64137 = CARTESIAN_POINT ( 'NONE',  ( 28.92187500061451644, 3.027376345333611329, 5.243569643749999010 ) ) ;
#64138 = CARTESIAN_POINT ( 'NONE',  ( 5.221875000614519813, -6.054752690667223547, -1.112240025338166033E-15 ) ) ;
#64139 = CARTESIAN_POINT ( 'NONE',  ( 16.83749999999999858, 5.773502691896255534, 3.535250795749688894E-16 ) ) ;
#64140 = CARTESIAN_POINT ( 'NONE',  ( 13.19062500061451537, -3.027376345333614438, 5.243569643749998122 ) ) ;
#64141 = CARTESIAN_POINT ( 'NONE',  ( -8.484601909799255319E-16, 18.68750000000000000, 34.61880215351700940 ) ) ;
#64142 = FACE_OUTER_BOUND ( 'NONE', #52148, .T. ) ;
#64143 = CARTESIAN_POINT ( 'NONE',  ( 18.67500000122903714, 2.886751345948129099, -4.999999999999998224 ) ) ;
#64144 = CARTESIAN_POINT ( 'NONE',  ( 3.680627977383748473, 9.304151242747314754, 25.24598017873988098 ) ) ;
#64145 = CARTESIAN_POINT ( 'NONE',  ( 16.95937500061451786, -4.119189519843965641, -2.378215178125001383 ) ) ;
#64146 = CARTESIAN_POINT ( 'NONE',  ( 7.678125000614516082, 4.541064518000418104, 2.621784821874999949 ) ) ;
#64147 = CARTESIAN_POINT ( 'NONE',  ( 24.04687500061451644, -3.027376345333614438, 5.243569643749998122 ) ) ;
#64148 = CARTESIAN_POINT ( 'NONE',  ( 2.121784821874999061, 19.70937500061451786, 26.32496088578401583 ) ) ;
#64149 = CARTESIAN_POINT ( 'NONE',  ( 23.78437500061451360, 6.421520780324663323E-16, -5.243569643749999010 ) ) ;
#64150 = CARTESIAN_POINT ( 'NONE',  ( 6.750000000000002665, -4.330127018922190985, -2.500000000000001332 ) ) ;
#64151 = CARTESIAN_POINT ( 'NONE',  ( 1.999999999999998668, 12.31250000122903465, 26.53589838486224650 ) ) ;
#64152 = CARTESIAN_POINT ( 'NONE',  ( 15.81562500061451537, 3.027376345333611329, 5.243569643749999010 ) ) ;
#64153 = CARTESIAN_POINT ( 'NONE',  ( 7.012500001229035718, 4.330127018922192761, -2.499999999999997780 ) ) ;
#64154 = CARTESIAN_POINT ( 'NONE',  ( 12.60937500061451821, 4.541064518000418104, -2.621784821874998173 ) ) ;
#64155 = CARTESIAN_POINT ( 'NONE',  ( 3.921850648269007422, -3.101535241682955579, 3.979058954293606565 ) ) ;
#64156 = ORIENTED_EDGE ( 'NONE', *, *, #14379, .T. ) ;
#64157 = CARTESIAN_POINT ( 'NONE',  ( 12.81562500061451537, -6.054752690667223547, -1.112240025338166033E-15 ) ) ;
#64158 = DIRECTION ( 'NONE',  ( -1.000000000000000000, -0.000000000000000000, -0.000000000000000000 ) ) ;
#64159 = CARTESIAN_POINT ( 'NONE',  ( 24.52500000122903145, 2.886751345948129099, -4.999999999999998224 ) ) ;
#64160 = CARTESIAN_POINT ( 'NONE',  ( 11.70937500061451608, 4.541064518000418104, -2.621784821874998173 ) ) ;
#64161 = CARTESIAN_POINT ( 'NONE',  ( 14.09062500061451750, -3.027376345333614438, 5.243569643749998122 ) ) ;
#64162 = CARTESIAN_POINT ( 'NONE',  ( 27.58125000122903359, 6.123233995736764310E-16, -4.999999999999998224 ) ) ;
#64163 = CARTESIAN_POINT ( 'NONE',  ( 23.03437500061451715, 4.541064518000418104, 2.621784821874999949 ) ) ;
#64164 = CARTESIAN_POINT ( 'NONE',  ( 1.071796769724497445, 15.92990381179669868, 26.00000000000000355 ) ) ;
#64165 =( BOUNDED_CURVE ( )  B_SPLINE_CURVE ( 2, ( #39796, #34960, #61577, #17950, #27982, #62312, #12066 ),
 .UNSPECIFIED., .F., .F. ) 
 B_SPLINE_CURVE_WITH_KNOTS ( ( 3, 2, 2, 3 ),
 ( 0.9343878867307400249, 0.9361111111111111160, 0.9388888888888888840, 0.9404282932007268503 ),
 .UNSPECIFIED. ) 
 CURVE ( )  GEOMETRIC_REPRESENTATION_ITEM ( )  RATIONAL_B_SPLINE_CURVE ( ( 0.9368944059126143031, 0.9168874154023497480, 1.000000000000000000, 0.8660254037844387076, 1.000000000000000000, 0.9257532144072448954, 0.9337994205692392580 ) ) 
 REPRESENTATION_ITEM ( '' )  );
#64166 = CARTESIAN_POINT ( 'NONE',  ( 7.687499999999997335, -2.886751345948237457, -4.999999999999807265 ) ) ;
#64167 = CARTESIAN_POINT ( 'NONE',  ( -1.999999999999997113, 19.62500000000000000, 33.46410161513775705 ) ) ;
#64168 = CARTESIAN_POINT ( 'NONE',  ( 4.243569643749999898, 15.09687500061451715, -27.54997392385601529 ) ) ;
#64169 = CARTESIAN_POINT ( 'NONE',  ( 15.00937500061451679, 0.000000000000000000, 5.243569643749999010 ) ) ;
#64170 = CARTESIAN_POINT ( 'NONE',  ( 17.55000000122903359, -2.886751345948129988, 4.999999999999997335 ) ) ;
#64171 = ADVANCED_FACE ( 'NONE', ( #20541 ), #66736, .F. ) ;
#64172 = CARTESIAN_POINT ( 'NONE',  ( 12.08437500061451608, 6.421520780324663323E-16, -5.243569643749999010 ) ) ;
#64173 = CARTESIAN_POINT ( 'NONE',  ( 2.121784821874999061, 10.70937500061451964, 26.32496088578401583 ) ) ;
#64174 = CARTESIAN_POINT ( 'NONE',  ( 19.08750000122903145, 6.123233995736764310E-16, -4.999999999999998224 ) ) ;
#64175 = CARTESIAN_POINT ( 'NONE',  ( 13.07812500061451821, 4.541064518000418104, 2.621784821874999949 ) ) ;
#64176 = AXIS2_PLACEMENT_3D ( 'NONE', #22688, #66312, #15689 ) ;
#64177 = EDGE_LOOP ( 'NONE', ( #49721, #4373, #32798, #48400 ) ) ;
#64178 = ORIENTED_EDGE ( 'NONE', *, *, #67328, .T. ) ;
#64179 = CARTESIAN_POINT ( 'NONE',  ( 17.06250000000000000, -5.773502691896255534, -1.060575238724906372E-15 ) ) ;
#64180 = CARTESIAN_POINT ( 'NONE',  ( 3.999999999999998668, 18.25624999877096855, 32.30940107675850470 ) ) ;
#64181 = CARTESIAN_POINT ( 'NONE',  ( 11.67187500061451821, 3.027376345333612662, -5.243569643749998122 ) ) ;
#64182 = CARTESIAN_POINT ( 'NONE',  ( 2.067223061484673163, 4.558648060312520123, 26.56624252461168822 ) ) ;
#64183 = CARTESIAN_POINT ( 'NONE',  ( 12.67500000122903536, -5.773502691896255534, -1.060575238724906372E-15 ) ) ;
#64184 = CARTESIAN_POINT ( 'NONE',  ( 20.62500000122903288, 2.886751345948126879, 4.999999999999999112 ) ) ;
#64185 = CARTESIAN_POINT ( 'NONE',  ( 17.27812500061451217, -4.541064518000419881, 2.621784821874995952 ) ) ;
#64186 = CARTESIAN_POINT ( 'NONE',  ( 21.66562500061451502, 3.027376345333611329, 5.243569643749999010 ) ) ;
#64187 = CARTESIAN_POINT ( 'NONE',  ( 4.265625000614517326, -6.054752690667223547, -1.112240025338166033E-15 ) ) ;
#64188 =( BOUNDED_CURVE ( )  B_SPLINE_CURVE ( 2, ( #3467, #25987, #48526, #37436, #30067, #43717, #50358 ),
 .UNSPECIFIED., .F., .F. ) 
 B_SPLINE_CURVE_WITH_KNOTS ( ( 3, 2, 2, 3 ),
 ( 0.9602520150385847053, 0.9611111111111111382, 0.9638888888888889062, 0.9646572887058436629 ),
 .UNSPECIFIED. ) 
 CURVE ( )  GEOMETRIC_REPRESENTATION_ITEM ( )  RATIONAL_B_SPLINE_CURVE ( ( 0.9427596708857610697, 0.9585650622062426018, 1.000000000000000000, 0.8660254037844387076, 1.000000000000000000, 0.9629394201248949736, 0.9463825270602228557 ) ) 
 REPRESENTATION_ITEM ( '' )  );
#64189 = CARTESIAN_POINT ( 'NONE',  ( 26.77499999999999858, 4.330127018922191873, 2.499999999999999556 ) ) ;
#64190 = CARTESIAN_POINT ( 'NONE',  ( 28.35000000000000142, -4.330127018922190985, -2.500000000000001332 ) ) ;
#64191 = CARTESIAN_POINT ( 'NONE',  ( 30.00000000000000000, 0.000000000000000000, 4.999999999999998224 ) ) ;
#64192 = CARTESIAN_POINT ( 'NONE',  ( 29.18437500061451573, 6.421520780324663323E-16, -5.243569643749999010 ) ) ;
#64193 = CARTESIAN_POINT ( 'NONE',  ( 20.23125000122902861, -4.330127018922194537, 2.499999999999995559 ) ) ;
#64194 = CARTESIAN_POINT ( 'NONE',  ( 2.121784821875001281, 15.50937500061451857, -26.32496088578401938 ) ) ;
#64195 = CARTESIAN_POINT ( 'NONE',  ( 4.612500001229032698, -4.330127018922190985, -2.500000000000001332 ) ) ;
#64196 = CARTESIAN_POINT ( 'NONE',  ( 5.924999999999999822, 6.123233995736764310E-16, -4.999999999999998224 ) ) ;
#64197 = CARTESIAN_POINT ( 'NONE',  ( 12.00000000000000000, 0.000000000000000000, 4.999999999999998224 ) ) ;
#64198 = CARTESIAN_POINT ( 'NONE',  ( 9.571875000614518569, 3.027376345333611329, 5.243569643749999010 ) ) ;
#64199 = CARTESIAN_POINT ( 'NONE',  ( 28.56562500061451715, -6.054752690667223547, -1.112240025338166033E-15 ) ) ;
#64200 = CARTESIAN_POINT ( 'NONE',  ( 65.00000000000000000, 0.000000000000000000, 0.000000000000000000 ) ) ;
#64201 = CARTESIAN_POINT ( 'NONE',  ( 45.00000000000000000, 0.000000000000000000, 0.000000000000000000 ) ) ;
#64202 = CARTESIAN_POINT ( 'NONE',  ( 7.320879633048903241E-15, 17.75000000122903288, -34.00000000000000000 ) ) ;
#64203 = CARTESIAN_POINT ( 'NONE',  ( 7.321875000614516793, 3.027376345333611329, 5.243569643749999010 ) ) ;
#64204 = CARTESIAN_POINT ( 'NONE',  ( 12.30937500061451573, 0.000000000000000000, 5.243569643749999010 ) ) ;
#64205 = CARTESIAN_POINT ( 'NONE',  ( 4.837500000000001243, -2.886751345948129988, 4.999999999999997335 ) ) ;
#64206 = CARTESIAN_POINT ( 'NONE',  ( -2.121784821874999949, 14.77812500061459389, 26.32496088578401938 ) ) ;
#64207 = CARTESIAN_POINT ( 'NONE',  ( 3.999999999999998668, 13.36250000000000071, 32.30940107675850470 ) ) ;
#64208 = CARTESIAN_POINT ( 'NONE',  ( 5.437500000000001776, -2.886751345948125991, -5.000000000000000000 ) ) ;
#64209 = CARTESIAN_POINT ( 'NONE',  ( 14.22187500061451537, 5.824947211148865298E-16, -4.756430356249998326 ) ) ;
#64210 = CARTESIAN_POINT ( 'NONE',  ( 19.82812500061451644, 4.541064518000418104, 2.621784821874999949 ) ) ;
#64211 = CARTESIAN_POINT ( 'NONE',  ( 12.62812500061451537, 4.541064518000418104, 2.621784821874999949 ) ) ;
#64212 = CARTESIAN_POINT ( 'NONE',  ( 24.79687500061451644, 0.000000000000000000, 4.756430356249998326 ) ) ;
#64213 = CARTESIAN_POINT ( 'NONE',  ( 8.859375000614518214, -4.541064518000417216, -2.621784821875001281 ) ) ;
#64214 = CARTESIAN_POINT ( 'NONE',  ( 27.07499999999999929, 6.123233995736764310E-16, -4.999999999999998224 ) ) ;
#64215 = CARTESIAN_POINT ( 'NONE',  ( 23.28750000122903430, 4.330127018922191873, 2.499999999999999556 ) ) ;
#64216 = VECTOR ( 'NONE', #59649, 1000.000000000000000 ) ;
#64217 = CARTESIAN_POINT ( 'NONE',  ( 17.02499999999999858, -4.330127018922194537, 2.499999999999995559 ) ) ;
#64218 = CARTESIAN_POINT ( 'NONE',  ( 11.03437500061451715, -4.541064518000419881, 2.621784821874995952 ) ) ;
#64219 = CARTESIAN_POINT ( 'NONE',  ( 25.50937500061451502, -4.541064518000417216, -2.621784821875001281 ) ) ;
#64220 = CARTESIAN_POINT ( 'NONE',  ( 3.759375000614517681, 0.000000000000000000, 5.243569643749999010 ) ) ;
#64221 = CARTESIAN_POINT ( 'NONE',  ( 20.78732959644809952, 2.500000000000000444, 3.499999999999999112 ) ) ;
#64222 = CARTESIAN_POINT ( 'NONE',  ( 19.62187500061451573, -6.054752690667223547, -1.112240025338166033E-15 ) ) ;
#64223 = CARTESIAN_POINT ( 'NONE',  ( 11.07187500061451679, -6.054752690667223547, -1.112240025338166033E-15 ) ) ;
#64224 = CARTESIAN_POINT ( 'NONE',  ( -3.756430356250000102, 13.76562499938548356, 30.00000000000000000 ) ) ;
#64225 = CARTESIAN_POINT ( 'NONE',  ( 22.83749999999999858, -2.886751345948129988, 4.999999999999997335 ) ) ;
#64226 = CARTESIAN_POINT ( 'NONE',  ( 4.000000000000000000, 12.95000000000000107, 30.00000000000000000 ) ) ;
#64227 = CARTESIAN_POINT ( 'NONE',  ( -2.121784821874996840, 11.38437500061451679, -26.32496088578401583 ) ) ;
#64228 = CARTESIAN_POINT ( 'NONE',  ( 25.17187500061451644, 2.746126346562645981, -4.756430356249997438 ) ) ;
#64229 = CARTESIAN_POINT ( 'NONE',  ( 14.05312500061451431, 0.000000000000000000, 5.243569643749999010 ) ) ;
#64230 = CARTESIAN_POINT ( 'NONE',  ( 4.125000000000000000, 6.123233995736764310E-16, -4.999999999999998224 ) ) ;
#64231 = CARTESIAN_POINT ( 'NONE',  ( 12.26250000122903394, -4.330127018922190985, -2.500000000000001332 ) ) ;
#64232 = CARTESIAN_POINT ( 'NONE',  ( 18.82500000000000284, -4.330127018922194537, 2.499999999999995559 ) ) ;
#64233 = CARTESIAN_POINT ( 'NONE',  ( 13.72500000000000142, 4.330127018922191873, 2.499999999999999556 ) ) ;
#64234 = CARTESIAN_POINT ( 'NONE',  ( -2.121784821874996840, 9.978125000614518569, 33.67503911421598417 ) ) ;
#64235 = CARTESIAN_POINT ( 'NONE',  ( 15.07500000122903394, 2.886751345948129099, -4.999999999999998224 ) ) ;
#64236 = VECTOR ( 'NONE', #68413, 1000.000000000000000 ) ;
#64237 = EDGE_CURVE ( 'NONE', #51755, #40213, #10937, .T. ) ;
#64238 = CARTESIAN_POINT ( 'NONE',  ( 24.34687500061451715, 6.054752690667223547, 3.707466751127219781E-16 ) ) ;
#64239 = LINE ( 'NONE', #8100, #38339 ) ;
#64240 = ORIENTED_EDGE ( 'NONE', *, *, #61190, .F. ) ;
#64241 = CARTESIAN_POINT ( 'NONE',  ( 19.75312500061451360, 4.541064518000418104, -2.621784821874998173 ) ) ;
#64242 = AXIS2_PLACEMENT_3D ( 'NONE', #29865, #52402, #30232 ) ;
#64243 = CARTESIAN_POINT ( 'NONE',  ( 3.403125000614518836, -4.541064518000417216, -2.621784821875001281 ) ) ;
#64244 = CARTESIAN_POINT ( 'NONE',  ( 18.90937500061451360, 4.541064518000418104, -2.621784821874998173 ) ) ;
#64245 = CARTESIAN_POINT ( 'NONE',  ( 29.18437500061451573, 6.421520780324663323E-16, -5.243569643749999010 ) ) ;
#64246 = CARTESIAN_POINT ( 'NONE',  ( 6.103125000614515905, -4.541064518000417216, -2.621784821875001281 ) ) ;
#64247 = CARTESIAN_POINT ( 'NONE',  ( 22.37812500061451360, 6.421520780324663323E-16, -5.243569643749999010 ) ) ;
#64248 = CARTESIAN_POINT ( 'NONE',  ( -2.121784821874999949, 16.12812500061451715, 26.32496088578401938 ) ) ;
#64249 = CARTESIAN_POINT ( 'NONE',  ( 17.81250000122903288, 4.330127018922192761, -2.499999999999997780 ) ) ;
#64250 = CARTESIAN_POINT ( 'NONE',  ( 12.57187500061452035, 2.746126346562645981, -4.756430356249997438 ) ) ;
#64251 = CARTESIAN_POINT ( 'NONE',  ( 8.728125000614518569, -4.541064518000419881, 2.621784821874995952 ) ) ;
#64252 = CARTESIAN_POINT ( 'NONE',  ( 3.534375000614518036, 6.421520780324663323E-16, -5.243569643749999010 ) ) ;
#64253 = CARTESIAN_POINT ( 'NONE',  ( 3.196875000614516793, 6.054752690667223547, 3.707466751127219781E-16 ) ) ;
#64254 = CARTESIAN_POINT ( 'NONE',  ( 22.58437500061451431, 4.541064518000418104, 2.621784821874999949 ) ) ;
#64255 = CARTESIAN_POINT ( 'NONE',  ( 14.84062500061451750, 6.054752690667223547, 3.707466751127219781E-16 ) ) ;
#64256 = CARTESIAN_POINT ( 'NONE',  ( 24.71250000122903145, 0.000000000000000000, 4.999999999999998224 ) ) ;
#64257 = EDGE_CURVE ( 'NONE', #9906, #64445, #30032, .T. ) ;
#64258 = CARTESIAN_POINT ( 'NONE',  ( 25.49062500061451786, -3.027376345333610441, -5.243569643749999898 ) ) ;
#64259 = CARTESIAN_POINT ( 'NONE',  ( 19.47187500061451360, 3.027376345333611329, 5.243569643749999010 ) ) ;
#64260 = CARTESIAN_POINT ( 'NONE',  ( 14.57812500061451644, -4.541064518000419881, 2.621784821874995952 ) ) ;
#64261 = CARTESIAN_POINT ( 'NONE',  ( 9.001249775931846008E-16, 17.72187500061451715, 34.90005215228797653 ) ) ;
#64262 = CARTESIAN_POINT ( 'NONE',  ( 18.70312500061451644, -4.541064518000417216, -2.621784821875001281 ) ) ;
#64263 = CARTESIAN_POINT ( 'NONE',  ( 29.16562500061451502, 3.027376345333613106, -5.243569643749998122 ) ) ;
#64264 = VERTEX_POINT ( 'NONE', #37550 ) ;
#64265 = CARTESIAN_POINT ( 'NONE',  ( 24.33749999999999858, -2.886751345948125991, -5.000000000000000000 ) ) ;
#64266 = CARTESIAN_POINT ( 'NONE',  ( 3.999999999999999112, 11.22500000000000142, -30.00000000000000000 ) ) ;
#64267 = CARTESIAN_POINT ( 'NONE',  ( -3.756430356249999214, 18.79062499938548214, 27.83122392262697531 ) ) ;
#64268 = CARTESIAN_POINT ( 'NONE',  ( 27.51562500061451644, 3.027376345333611329, 5.243569643749999010 ) ) ;
#64269 = CARTESIAN_POINT ( 'NONE',  ( 7.340625000614518392, -3.027376345333614438, 5.243569643749998122 ) ) ;
#64270 = CARTESIAN_POINT ( 'NONE',  ( 19.72500000122903074, 2.886751345948126879, 4.999999999999999112 ) ) ;
#64271 = CARTESIAN_POINT ( 'NONE',  ( 25.71562500061451573, 3.027376345333611329, 5.243569643749999010 ) ) ;
#64272 = CARTESIAN_POINT ( 'NONE',  ( 25.08749999999999858, -2.886751345948129988, 4.999999999999997335 ) ) ;
#64273 = CARTESIAN_POINT ( 'NONE',  ( 3.999999999999999112, 14.93750000122903288, -30.00000000000000000 ) ) ;
#64274 = EDGE_CURVE ( 'NONE', #19923, #54432, #64556, .T. ) ;
#64275 = CARTESIAN_POINT ( 'NONE',  ( 27.47812500061451502, 4.541064518000418104, 2.621784821874999949 ) ) ;
#64276 = CARTESIAN_POINT ( 'NONE',  ( 9.365625000614519635, 3.027376345333613106, -5.243569643749998122 ) ) ;
#64277 = ORIENTED_EDGE ( 'NONE', *, *, #66154, .T. ) ;
#64278 = CARTESIAN_POINT ( 'NONE',  ( 24.66562500061451502, 3.027376345333613106, -5.243569643749998122 ) ) ;
#64279 = CARTESIAN_POINT ( 'NONE',  ( 5.090625000614516615, -3.027376345333614438, 5.243569643749998122 ) ) ;
#64280 = AXIS2_PLACEMENT_3D ( 'NONE', #35996, #7925, #30821 ) ;
#64281 = CARTESIAN_POINT ( 'NONE',  ( 14.55937500061451573, 0.000000000000000000, 4.756430356249998326 ) ) ;
#64282 = CYLINDRICAL_SURFACE ( 'NONE', #53855, 4.999999999999998224 ) ;
#64283 = CARTESIAN_POINT ( 'NONE',  ( 12.67499999999999893, 6.123233995736764310E-16, -4.999999999999998224 ) ) ;
#64285 = CARTESIAN_POINT ( 'NONE',  ( 14.03437500061451715, 4.541064518000418104, 2.621784821874999949 ) ) ;
#64284 = CIRCLE ( 'NONE', #6514, 1.500000000000000444 ) ;
#64286 = CARTESIAN_POINT ( 'NONE',  ( 8.662500001229034297, -4.330127018922190985, -2.500000000000001332 ) ) ;
#64287 = CARTESIAN_POINT ( 'NONE',  ( 17.97187500061451715, 3.027376345333613106, -5.243569643749998122 ) ) ;
#64288 = CARTESIAN_POINT ( 'NONE',  ( 16.23750000000000071, -2.886751345948125991, -5.000000000000000000 ) ) ;
#64289 = CARTESIAN_POINT ( 'NONE',  ( 8.859375000614518214, -4.541064518000417216, -2.621784821875001281 ) ) ;
#64290 = CARTESIAN_POINT ( 'NONE',  ( 2.121784821874999061, 12.00312500061451715, -33.67503911421598417 ) ) ;
#64291 = VECTOR ( 'NONE', #42718, 1000.000000000000000 ) ;
#64292 = CARTESIAN_POINT ( 'NONE',  ( -3.999999999999999112, 11.90000000000000036, -30.00000000000000000 ) ) ;
#64293 = CARTESIAN_POINT ( 'NONE',  ( 23.14687500061451786, -4.119189519843965641, -2.378215178125001383 ) ) ;
#64294 = ORIENTED_EDGE ( 'NONE', *, *, #55830, .F. ) ;
#64295 = CARTESIAN_POINT ( 'NONE',  ( 25.60312500061451502, 4.541064518000418104, -2.621784821874998173 ) ) ;
#64296 = DIRECTION ( 'NONE',  ( 0.000000000000000000, 0.000000000000000000, 1.000000000000000000 ) ) ;
#64297 = CARTESIAN_POINT ( 'NONE',  ( 25.32187500061451857, 3.027376345333611329, 5.243569643749999010 ) ) ;
#64298 = CARTESIAN_POINT ( 'NONE',  ( 28.65937500061451715, -4.541064518000417216, -2.621784821875001281 ) ) ;
#64299 = CARTESIAN_POINT ( 'NONE',  ( 22.53750000000000142, -2.886751345948125991, -5.000000000000000000 ) ) ;
#64300 = CARTESIAN_POINT ( 'NONE',  ( 3.665625000614517681, 3.027376345333611329, 5.243569643749999010 ) ) ;
#64301 = CARTESIAN_POINT ( 'NONE',  ( 22.54687500061451644, 0.000000000000000000, 4.756430356249998326 ) ) ;
#64302 = CARTESIAN_POINT ( 'NONE',  ( 17.22187500061451715, 3.027376345333611329, 5.243569643749999010 ) ) ;
#64303 = CARTESIAN_POINT ( 'NONE',  ( 8.671875000614518214, -4.119189519843968306, 2.378215178124996054 ) ) ;
#64304 = CARTESIAN_POINT ( 'NONE',  ( 3.178125000614515638, 4.541064518000418104, 2.621784821874999949 ) ) ;
#64305 = CARTESIAN_POINT ( 'NONE',  ( 8.971875000614515372, 3.027376345333613106, -5.243569643749998122 ) ) ;
#64306 = CARTESIAN_POINT ( 'NONE',  ( 17.89687500061451431, -3.027376345333610441, -5.243569643749999898 ) ) ;
#64307 = CARTESIAN_POINT ( 'NONE',  ( 9.993750001229033231, -2.886751345948126435, -5.000000000000000000 ) ) ;
#64308 = CARTESIAN_POINT ( 'NONE',  ( 25.91250000000000142, 2.886751345948126879, 4.999999999999999112 ) ) ;
#64309 = CARTESIAN_POINT ( 'NONE',  ( 28.02187500061451431, 3.027376345333611329, 5.243569643749999010 ) ) ;
#64310 = CYLINDRICAL_SURFACE ( 'NONE', #72656, 4.999999999999998224 ) ;
#64311 = CARTESIAN_POINT ( 'NONE',  ( 14.28750000122903430, 4.330127018922191873, 2.499999999999999556 ) ) ;
#64312 = ORIENTED_EDGE ( 'NONE', *, *, #58905, .T. ) ;
#64313 = CARTESIAN_POINT ( 'NONE',  ( 8.775000000000002132, 4.330127018922191873, 2.499999999999999556 ) ) ;
#64314 = CARTESIAN_POINT ( 'NONE',  ( 11.74687500061451573, 0.000000000000000000, 4.756430356249998326 ) ) ;
#64315 = CARTESIAN_POINT ( 'NONE',  ( 22.07812500061451644, 4.541064518000418104, 2.621784821874999949 ) ) ;
#64316 = CARTESIAN_POINT ( 'NONE',  ( 11.17500000000000071, -4.330127018922194537, 2.499999999999995559 ) ) ;
#64317 = CARTESIAN_POINT ( 'NONE',  ( 7.537500001229033408, 4.330127018922191873, 2.499999999999999556 ) ) ;
#64318 = CARTESIAN_POINT ( 'NONE',  ( 6.553125000614518747, -4.541064518000417216, -2.621784821875001281 ) ) ;
#64319 = CARTESIAN_POINT ( 'NONE',  ( 23.02499999999999858, 6.123233995736764310E-16, -4.999999999999998224 ) ) ;
#64320 = CARTESIAN_POINT ( 'NONE',  ( 19.94062500061451715, -3.027376345333614438, 5.243569643749998122 ) ) ;
#64321 = CARTESIAN_POINT ( 'NONE',  ( 25.65000000122903145, -2.886751345948129988, 4.999999999999997335 ) ) ;
#64322 = CARTESIAN_POINT ( 'NONE',  ( -1.878215178125001827, 20.59062499938548285, 33.25316411605952283 ) ) ;
#64323 = CARTESIAN_POINT ( 'NONE',  ( 4.762499999999999289, 2.886751345948126879, 4.999999999999999112 ) ) ;
#64324 = ORIENTED_EDGE ( 'NONE', *, *, #9299, .F. ) ;
#64325 = CARTESIAN_POINT ( 'NONE',  ( 19.49062500061451431, -3.027376345333614438, 5.243569643749998122 ) ) ;
#64326 = CARTESIAN_POINT ( 'NONE',  ( 25.75312500061451715, 0.000000000000000000, 5.243569643749999010 ) ) ;
#64327 = CARTESIAN_POINT ( 'NONE',  ( 27.42187500061451644, 3.027376345333613106, -5.243569643749998122 ) ) ;
#64328 = EDGE_CURVE ( 'NONE', #57266, #46535, #31551, .T. ) ;
#64329 = CARTESIAN_POINT ( 'NONE',  ( 13.86562500061451431, 3.027376345333613106, -5.243569643749998122 ) ) ;
#64330 = CARTESIAN_POINT ( 'NONE',  ( 28.97812500061451502, -4.541064518000419881, 2.621784821874995952 ) ) ;
#64331 = CARTESIAN_POINT ( 'NONE',  ( 9.928125000614517859, 4.541064518000418104, 2.621784821874999949 ) ) ;
#64332 = CYLINDRICAL_SURFACE ( 'NONE', #39250, 4.999999999999998224 ) ;
#64333 = CARTESIAN_POINT ( 'NONE',  ( -4.243569643749997233, 13.14687500061451786, 32.45002607614398471 ) ) ;
#64334 = AXIS2_PLACEMENT_3D ( 'NONE', #56877, #51714, #28100 ) ;
#64335 = CARTESIAN_POINT ( 'NONE',  ( 25.83750000122903501, 6.123233995736764310E-16, -4.999999999999998224 ) ) ;
#64336 = CARTESIAN_POINT ( 'NONE',  ( 19.62187500061451573, -5.492252693125287522, -1.008910452111647106E-15 ) ) ;
#64337 = CARTESIAN_POINT ( 'NONE',  ( 16.90312500061451573, -4.541064518000417216, -2.621784821875001281 ) ) ;
#64338 = CARTESIAN_POINT ( 'NONE',  ( -1.071796769724492115, 15.51740381056766438, 34.00000000000000000 ) ) ;
#64339 = CARTESIAN_POINT ( 'NONE',  ( 9.421875000614519990, 3.027376345333613106, -5.243569643749998122 ) ) ;
#64340 = CARTESIAN_POINT ( 'NONE',  ( 8.634375000614518569, 4.541064518000418104, 2.621784821874999949 ) ) ;
#64341 = CARTESIAN_POINT ( 'NONE',  ( 17.89687500061451431, -3.027376345333610441, -5.243569643749999898 ) ) ;
#64342 = ORIENTED_EDGE ( 'NONE', *, *, #68280, .F. ) ;
#64343 = CARTESIAN_POINT ( 'NONE',  ( 29.48437500061451644, -4.541064518000419881, 2.621784821874995952 ) ) ;
#64344 = CARTESIAN_POINT ( 'NONE',  ( 22.11562500061451786, 3.027376345333611329, 5.243569643749999010 ) ) ;
#64345 = VECTOR ( 'NONE', #55654, 1000.000000000000000 ) ;
#64346 = CARTESIAN_POINT ( 'NONE',  ( 15.42187500061451821, 3.027376345333611329, 5.243569643749999010 ) ) ;
#64347 = CARTESIAN_POINT ( 'NONE',  ( 22.67812500061451431, -4.541064518000419881, 2.621784821874995952 ) ) ;
#64348 = CARTESIAN_POINT ( 'NONE',  ( -3.999999999999997335, 13.73749999999999893, 32.30940107675850470 ) ) ;
#64349 = CARTESIAN_POINT ( 'NONE',  ( 26.95312500061451644, 4.541064518000418104, -2.621784821874998173 ) ) ;
#64350 = CARTESIAN_POINT ( 'NONE',  ( 8.400000001229035007, 5.773502691896255534, 3.535250795749688894E-16 ) ) ;
#64351 = VECTOR ( 'NONE', #31890, 1000.000000000000000 ) ;
#64352 = ORIENTED_EDGE ( 'NONE', *, *, #66154, .F. ) ;
#64353 = CARTESIAN_POINT ( 'NONE',  ( 4.875000001229034652, 2.886751345948126879, 4.999999999999999112 ) ) ;
#64354 = CARTESIAN_POINT ( 'NONE',  ( -2.000000000000000000, 16.77500000000000213, -33.46410161513775705 ) ) ;
#64355 = CARTESIAN_POINT ( 'NONE',  ( 24.03750000122903430, 6.123233995736764310E-16, -4.999999999999998224 ) ) ;
#64356 = CARTESIAN_POINT ( 'NONE',  ( -3.756430356250000102, 12.97812499938548214, 30.00000000000000000 ) ) ;
#64357 = CARTESIAN_POINT ( 'NONE',  ( 6.421875000614519102, 3.027376345333611329, 5.243569643749999010 ) ) ;
#64358 = CARTESIAN_POINT ( 'NONE',  ( 21.05625000122903145, 0.000000000000000000, 4.999999999999998224 ) ) ;
#64359 = CARTESIAN_POINT ( 'NONE',  ( 14.50312500061451537, 0.000000000000000000, 5.243569643749999010 ) ) ;
#64360 = CARTESIAN_POINT ( 'NONE',  ( 11.44687500061451857, -3.027376345333614438, 5.243569643749998122 ) ) ;
#64361 = CARTESIAN_POINT ( 'NONE',  ( 27.60000000122903430, -2.886751345948125991, -5.000000000000000000 ) ) ;
#64362 = CARTESIAN_POINT ( 'NONE',  ( 17.25937500061451502, 0.000000000000000000, 5.243569643749999010 ) ) ;
#64363 = CARTESIAN_POINT ( 'NONE',  ( 4.996875000614516615, 6.054752690667223547, 3.707466751127219781E-16 ) ) ;
#64364 = FACE_OUTER_BOUND ( 'NONE', #49618, .T. ) ;
#64365 = CARTESIAN_POINT ( 'NONE',  ( 7.865625000614516971, -6.054752690667223547, -1.112240025338166033E-15 ) ) ;
#64366 = CARTESIAN_POINT ( 'NONE',  ( 17.09062500061451573, 6.054752690667223547, 3.707466751127219781E-16 ) ) ;
#64367 = ORIENTED_EDGE ( 'NONE', *, *, #34144, .T. ) ;
#64368 = CARTESIAN_POINT ( 'NONE',  ( 14.50312500061451537, 0.000000000000000000, 5.243569643749999010 ) ) ;
#64369 = CARTESIAN_POINT ( 'NONE',  ( 8.775000001229033231, 2.886751345948129099, -4.999999999999998224 ) ) ;
#64370 = CARTESIAN_POINT ( 'NONE',  ( 9.740625000614516082, -3.027376345333610441, -5.243569643749999898 ) ) ;
#64371 = CARTESIAN_POINT ( 'NONE',  ( 21.04687500061451644, -2.746126346562642428, -4.756430356249999214 ) ) ;
#64372 = CARTESIAN_POINT ( 'NONE',  ( 10.38750000000000107, -2.886751345948125991, -5.000000000000000000 ) ) ;
#64373 = CARTESIAN_POINT ( 'NONE',  ( 5.850000001229035185, -2.886751345948129988, 4.999999999999997335 ) ) ;
#64374 = CARTESIAN_POINT ( 'NONE',  ( 15.12187500061451750, -6.054752690667223547, -1.112240025338166033E-15 ) ) ;
#64375 = CARTESIAN_POINT ( 'NONE',  ( 16.38750000122903216, 6.123233995736764310E-16, -4.999999999999998224 ) ) ;
#64376 = CARTESIAN_POINT ( 'NONE',  ( 25.19999999999999929, -4.330127018922190985, -2.500000000000001332 ) ) ;
#64377 = AXIS2_PLACEMENT_3D ( 'NONE', #13774, #31509, #54049 ) ;
#64378 = CARTESIAN_POINT ( 'NONE',  ( -4.243569643749999898, 19.31562500061451715, -32.45002607614398471 ) ) ;
#64379 = DIRECTION ( 'NONE',  ( -1.000000000000000000, -0.000000000000000000, -0.000000000000000000 ) ) ;
#64380 = CARTESIAN_POINT ( 'NONE',  ( 23.08125000122903359, 6.123233995736764310E-16, -4.999999999999998224 ) ) ;
#64381 = CYLINDRICAL_SURFACE ( 'NONE', #6858, 4.999999999999998224 ) ;
#64382 = CARTESIAN_POINT ( 'NONE',  ( 2.000000000000001332, 14.41250000122903430, 33.46410161513774995 ) ) ;
#64383 = CARTESIAN_POINT ( 'NONE',  ( 15.23437500061451644, 6.421520780324663323E-16, -5.243569643749999010 ) ) ;
#64384 =( BOUNDED_CURVE ( )  B_SPLINE_CURVE ( 2, ( #67059, #38607, #61490, #33055, #55955, #28604, #5351, #44526, #45238 ),
 .UNSPECIFIED., .F., .F. ) 
 B_SPLINE_CURVE_WITH_KNOTS ( ( 3, 2, 2, 2, 3 ),
 ( 0.4239130434782608647, 0.4275362318840579823, 0.4347826086956521618, 0.4420289855072463969, 0.4456521739130435145 ),
 .UNSPECIFIED. ) 
 CURVE ( )  GEOMETRIC_REPRESENTATION_ITEM ( )  RATIONAL_B_SPLINE_CURVE ( ( 0.9330127018922194093, 0.9330127018922194093, 1.000000000000000000, 0.8660254037844387076, 1.000000000000000000, 0.8660254037844387076, 1.000000000000000000, 0.9330127018922188542, 0.9330127018922194093 ) ) 
 REPRESENTATION_ITEM ( '' )  );
#64385 = CARTESIAN_POINT ( 'NONE',  ( 29.69999999999999574, -4.330127018922190985, -2.500000000000001332 ) ) ;
#64386 = ADVANCED_FACE ( 'NONE', ( #56372 ), #45288, .T. ) ;
#64387 = CARTESIAN_POINT ( 'NONE',  ( 14.65312500061451573, -4.541064518000417216, -2.621784821875001281 ) ) ;
#64388 = CARTESIAN_POINT ( 'NONE',  ( 29.10937500061451999, 2.746126346562645981, -4.756430356249997438 ) ) ;
#64389 = CARTESIAN_POINT ( 'NONE',  ( 22.84687500061451715, -3.027376345333610441, -5.243569643749999898 ) ) ;
#64390 = CARTESIAN_POINT ( 'NONE',  ( 16.13437500061451502, 5.492252693125287522, 3.363034840372157021E-16 ) ) ;
#64391 = CARTESIAN_POINT ( 'NONE',  ( 9.928125000614517859, 4.541064518000418104, 2.621784821874999949 ) ) ;
#64392 = CARTESIAN_POINT ( 'NONE',  ( 14.52187500061451608, 3.027376345333611329, 5.243569643749999010 ) ) ;
#64393 = ORIENTED_EDGE ( 'NONE', *, *, #7054, .T. ) ;
#64394 = CARTESIAN_POINT ( 'NONE',  ( 26.48437500061451644, 6.421520780324663323E-16, -5.243569643749999010 ) ) ;
#64395 = CARTESIAN_POINT ( 'NONE',  ( 28.37812500061451715, 4.541064518000418104, 2.621784821874999949 ) ) ;
#64396 = CARTESIAN_POINT ( 'NONE',  ( 18.92812500061451431, 4.541064518000418104, 2.621784821874999949 ) ) ;
#64397 = CARTESIAN_POINT ( 'NONE',  ( 29.61562500061451431, 3.027376345333613106, -5.243569643749998122 ) ) ;
#64398 = CARTESIAN_POINT ( 'NONE',  ( 4.869452396223757695, 1.135286901598331566, -5.119236970012235766 ) ) ;
#64399 = CARTESIAN_POINT ( 'NONE',  ( 7.987500000000000711, -2.886751345948129988, 4.999999999999997335 ) ) ;
#64400 = CARTESIAN_POINT ( 'NONE',  ( 20.36250000122903359, -4.330127018922190985, -2.500000000000001332 ) ) ;
#64401 = CARTESIAN_POINT ( 'NONE',  ( -5.810221930991193690E-16, 18.65000000122903501, -34.00000000000000000 ) ) ;
#64402 = CARTESIAN_POINT ( 'NONE',  ( 11.37187500061451573, -4.119189519843968306, 2.378215178124996054 ) ) ;
#64403 = VERTEX_POINT ( 'NONE', #230 ) ;
#64404 = CARTESIAN_POINT ( 'NONE',  ( 17.39999999999999858, 0.000000000000000000, 4.999999999999998224 ) ) ;
#64405 = CARTESIAN_POINT ( 'NONE',  ( 19.20000000000000284, 0.000000000000000000, 4.999999999999998224 ) ) ;
#64406 = CARTESIAN_POINT ( 'NONE',  ( 18.94687500061451502, 6.054752690667223547, 3.707466751127219781E-16 ) ) ;
#64407 = CARTESIAN_POINT ( 'NONE',  ( 14.01562500061451644, 3.027376345333611329, 5.243569643749999010 ) ) ;
#64408 = ORIENTED_EDGE ( 'NONE', *, *, #49257, .F. ) ;
#64409 = CARTESIAN_POINT ( 'NONE',  ( 1.626862140677534273E-15, 18.42500000122903359, -26.00000000000000355 ) ) ;
#64410 = CARTESIAN_POINT ( 'NONE',  ( 5.240625000614516971, -3.027376345333610441, -5.243569643749999898 ) ) ;
#64411 = CARTESIAN_POINT ( 'NONE',  ( -3.756430356250000990, 12.90312499938548463, 32.16877607737301048 ) ) ;
#64412 = CARTESIAN_POINT ( 'NONE',  ( 11.88749999999999751, 5.773502691896255534, 3.535250795749688894E-16 ) ) ;
#64413 = CARTESIAN_POINT ( 'NONE',  ( 29.59687500061451360, 4.119189519843966529, -2.378215178124998275 ) ) ;
#64414 = CARTESIAN_POINT ( 'NONE',  ( 4.243569643749999010, 15.11562500061451608, 27.54997392385601174 ) ) ;
#64415 = CARTESIAN_POINT ( 'NONE',  ( 26.84062500061451573, -3.027376345333610441, -5.243569643749999898 ) ) ;
#64416 = CARTESIAN_POINT ( 'NONE',  ( 9.412499999999999645, -5.773502691896255534, -1.060575238724906372E-15 ) ) ;
#64417 = CARTESIAN_POINT ( 'NONE',  ( 3.756430356250000546, 17.17812499938548143, 27.83122392262697886 ) ) ;
#64418 = CARTESIAN_POINT ( 'NONE',  ( 23.85937500061451644, 4.541064518000418104, -2.621784821874998173 ) ) ;
#64419 = ORIENTED_EDGE ( 'NONE', *, *, #65890, .T. ) ;
#64420 = CARTESIAN_POINT ( 'NONE',  ( 22.45312500061451644, 4.541064518000418104, -2.621784821874998173 ) ) ;
#64421 = CARTESIAN_POINT ( 'NONE',  ( 22.20937500061451431, 0.000000000000000000, 5.243569643749999010 ) ) ;
#64422 = CARTESIAN_POINT ( 'NONE',  ( 9.001249775931846008E-16, 16.31562500061459176, -25.09994784771203058 ) ) ;
#64423 = CARTESIAN_POINT ( 'NONE',  ( 7.678125000614516082, 4.541064518000418104, 2.621784821874999949 ) ) ;
#64424 = CARTESIAN_POINT ( 'NONE',  ( 26.89687500061451431, -2.746126346562641984, -4.756430356249999214 ) ) ;
#64425 = CARTESIAN_POINT ( 'NONE',  ( 24.89062500061451644, -3.027376345333614438, 5.243569643749998122 ) ) ;
#64426 = CARTESIAN_POINT ( 'NONE',  ( 10.69687500061451679, -2.746126346562642428, -4.756430356249999214 ) ) ;
#64427 = CARTESIAN_POINT ( 'NONE',  ( -3.756430356249999214, 15.52812499938548108, 27.83122392262697531 ) ) ;
#64428 = CARTESIAN_POINT ( 'NONE',  ( 16.84687500061451715, -3.027376345333614438, 5.243569643749998122 ) ) ;
#64429 = CARTESIAN_POINT ( 'NONE',  ( 25.43437500061451573, -4.541064518000419881, 2.621784821874995952 ) ) ;
#64430 = CARTESIAN_POINT ( 'NONE',  ( 4.243569643749999898, 13.78437500061451715, 30.00000000000000000 ) ) ;
#64431 = CARTESIAN_POINT ( 'NONE',  ( 5.315625000614516260, 3.027376345333613106, -5.243569643749998122 ) ) ;
#64432 = CARTESIAN_POINT ( 'NONE',  ( 29.42812500061451431, -4.541064518000419881, 2.621784821874995952 ) ) ;
#64433 = CARTESIAN_POINT ( 'NONE',  ( 3.009375000614516793, -4.541064518000417216, -2.621784821875001281 ) ) ;
#64434 = DIRECTION ( 'NONE',  ( 0.000000000000000000, 0.000000000000000000, 1.000000000000000000 ) ) ;
#64435 = CARTESIAN_POINT ( 'NONE',  ( 4.228125000614517681, -4.541064518000419881, 2.621784821874995952 ) ) ;
#64436 = CARTESIAN_POINT ( 'NONE',  ( 8.484375000614518214, 6.421520780324663323E-16, -5.243569643749999010 ) ) ;
#64437 = PRESENTATION_STYLE_ASSIGNMENT (( #69985 ) ) ;
#64438 = CARTESIAN_POINT ( 'NONE',  ( 15.82500000122903216, -5.773502691896255534, -1.060575238724906372E-15 ) ) ;
#64439 = CARTESIAN_POINT ( 'NONE',  ( 29.57812500061451644, 6.421520780324663323E-16, -5.243569643749999010 ) ) ;
#64440 = CARTESIAN_POINT ( 'NONE',  ( 6.215625000614517504, 3.027376345333613106, -5.243569643749998122 ) ) ;
#64441 = CARTESIAN_POINT ( 'NONE',  ( 3.999999999999998668, 14.20624999877096606, 32.30940107675850470 ) ) ;
#64442 = CARTESIAN_POINT ( 'NONE',  ( 21.20625000122903359, -4.330127018922190985, -2.500000000000001332 ) ) ;
#64443 = CARTESIAN_POINT ( 'NONE',  ( 14.03437500061451715, 4.541064518000418104, 2.621784821874999949 ) ) ;
#64444 = CARTESIAN_POINT ( 'NONE',  ( 3.999999999999998668, 17.67500000122903359, 27.69059892324149530 ) ) ;
#64445 = VERTEX_POINT ( 'NONE', #6483 ) ;
#64446 = CARTESIAN_POINT ( 'NONE',  ( 21.06562500061451715, 3.027376345333613106, -5.243569643749998122 ) ) ;
#64447 = CARTESIAN_POINT ( 'NONE',  ( 7.228125000614517681, 4.541064518000418104, 2.621784821874999949 ) ) ;
#64448 = ADVANCED_FACE ( 'NONE', ( #17551 ), #17905, .T. ) ;
#64449 = CARTESIAN_POINT ( 'NONE',  ( 24.53437500061451715, -4.541064518000419881, 2.621784821874995952 ) ) ;
#64450 = CARTESIAN_POINT ( 'NONE',  ( 7.790625000614518569, -3.027376345333614438, 5.243569643749998122 ) ) ;
#64451 = CARTESIAN_POINT ( 'NONE',  ( 18.97499999999999787, 6.123233995736764310E-16, -4.999999999999998224 ) ) ;
#64452 = CARTESIAN_POINT ( 'NONE',  ( 10.87500000122903288, -5.773502691896255534, -1.060575238724906372E-15 ) ) ;
#64453 = CARTESIAN_POINT ( 'NONE',  ( 25.19062500061451715, 6.054752690667223547, 3.707466751127219781E-16 ) ) ;
#64454 = CARTESIAN_POINT ( 'NONE',  ( -0.7368814052146555049, 9.803648494990884643, -34.17910147232696261 ) ) ;
#64455 = CARTESIAN_POINT ( 'NONE',  ( 10.05000000122903181, -2.886751345948125991, -5.000000000000000000 ) ) ;
#64456 = CARTESIAN_POINT ( 'NONE',  ( 22.37812500061451360, 6.421520780324663323E-16, -5.243569643749999010 ) ) ;
#64457 = CARTESIAN_POINT ( 'NONE',  ( 19.07812500061451644, -4.541064518000419881, 2.621784821874995952 ) ) ;
#64458 = CARTESIAN_POINT ( 'NONE',  ( 29.63437500061451502, 5.824947211148865298E-16, -4.756430356249998326 ) ) ;
#64459 = CARTESIAN_POINT ( 'NONE',  ( 18.52499999999999858, 6.123233995736764310E-16, -4.999999999999998224 ) ) ;
#64460 = CARTESIAN_POINT ( 'NONE',  ( 13.76250000122903394, 4.330127018922192761, -2.499999999999997780 ) ) ;
#64461 = CARTESIAN_POINT ( 'NONE',  ( 11.24062500061451608, 6.054752690667223547, 3.707466751127219781E-16 ) ) ;
#64462 = CARTESIAN_POINT ( 'NONE',  ( 12.77812500061451750, -4.541064518000419881, 2.621784821874995952 ) ) ;
#64463 = CARTESIAN_POINT ( 'NONE',  ( 22.72500000122903430, 2.886751345948129099, -4.999999999999998224 ) ) ;
#64464 = CARTESIAN_POINT ( 'NONE',  ( 22.05937500061451573, 4.541064518000418104, -2.621784821874998173 ) ) ;
#64465 = CARTESIAN_POINT ( 'NONE',  ( 21.98437500061451644, 6.421520780324663323E-16, -5.243569643749999010 ) ) ;
#64466 = CARTESIAN_POINT ( 'NONE',  ( 25.38749999999999929, 5.773502691896255534, 3.535250795749688401E-16 ) ) ;
#64467 = CARTESIAN_POINT ( 'NONE',  ( 7.875000001229034652, 2.886751345948129099, -4.999999999999998224 ) ) ;
#64468 = CARTESIAN_POINT ( 'NONE',  ( 6.759375000614516793, 4.541064518000418104, -2.621784821874998173 ) ) ;
#64469 = CARTESIAN_POINT ( 'NONE',  ( 24.30937500061451573, 4.541064518000418104, -2.621784821874998173 ) ) ;
#64470 = CARTESIAN_POINT ( 'NONE',  ( 4.544030691951923551, 2.086093255490381715, -4.659623712765267989 ) ) ;
#64471 = CARTESIAN_POINT ( 'NONE',  ( 22.04062500061451502, 6.054752690667223547, 3.707466751127219781E-16 ) ) ;
#64472 = CARTESIAN_POINT ( 'NONE',  ( 23.07187500061451857, 3.027376345333611329, 5.243569643749999010 ) ) ;
#64473 = CARTESIAN_POINT ( 'NONE',  ( 1.878215178125000495, 17.77812499938548285, 26.74683588394047007 ) ) ;
#64474 = CARTESIAN_POINT ( 'NONE',  ( -3.999999999999999112, 14.48750000000000071, 27.69059892324149530 ) ) ;
#64475 = VECTOR ( 'NONE', #52100, 1000.000000000000000 ) ;
#64476 = CARTESIAN_POINT ( 'NONE',  ( 1.626862140677534273E-15, 15.61250000000000071, 34.00000000000000000 ) ) ;
#64477 = CARTESIAN_POINT ( 'NONE',  ( 5.934375000614517504, 4.541064518000418104, 2.621784821874999949 ) ) ;
#64478 = CARTESIAN_POINT ( 'NONE',  ( 17.01562500061451644, 3.027376345333613106, -5.243569643749998122 ) ) ;
#64479 = EDGE_LOOP ( 'NONE', ( #33421, #13652, #66426, #7799 ) ) ;
#64480 = FACE_OUTER_BOUND ( 'NONE', #54237, .T. ) ;
#64481 = CARTESIAN_POINT ( 'NONE',  ( 25.60312500061451502, 4.541064518000418104, -2.621784821874998173 ) ) ;
#64482 = CARTESIAN_POINT ( 'NONE',  ( 2.896875000614518747, -3.027376345333614438, 5.243569643749998122 ) ) ;
#64483 = CARTESIAN_POINT ( 'NONE',  ( 4.720164951879130655, 1.649934272948560654, 4.824171440055819993 ) ) ;
#64484 = CARTESIAN_POINT ( 'NONE',  ( 8.512500001229033941, 0.000000000000000000, 4.999999999999998224 ) ) ;
#64485 = CARTESIAN_POINT ( 'NONE',  ( 13.61250000000000071, 2.886751345948129099, -4.999999999999998224 ) ) ;
#64486 = CARTESIAN_POINT ( 'NONE',  ( 19.90312500061451573, 0.000000000000000000, 5.243569643749999010 ) ) ;
#64487 = VERTEX_POINT ( 'NONE', #29732 ) ;
#64488 = CARTESIAN_POINT ( 'NONE',  ( 24.22500000000000142, -4.330127018922194537, 2.499999999999995559 ) ) ;
#64489 = EDGE_CURVE ( 'NONE', #44084, #41163, #46660, .T. ) ;
#64490 = CARTESIAN_POINT ( 'NONE',  ( 25.92187500061451999, -6.054752690667223547, -1.112240025338166033E-15 ) ) ;
#64491 = ORIENTED_EDGE ( 'NONE', *, *, #35816, .T. ) ;
#64492 = CARTESIAN_POINT ( 'NONE',  ( 3.009043979185748174, -3.993209162649682842, -3.398434824636790363 ) ) ;
#64493 = CARTESIAN_POINT ( 'NONE',  ( 13.15312500061451750, 0.000000000000000000, 5.243569643749999010 ) ) ;
#64494 = CARTESIAN_POINT ( 'NONE',  ( 25.05000000122903359, 5.773502691896255534, 3.535250795749688401E-16 ) ) ;
#64495 = CARTESIAN_POINT ( 'NONE',  ( 15.90937500061451360, -5.492252693125287522, -1.008910452111647106E-15 ) ) ;
#64496 = CARTESIAN_POINT ( 'NONE',  ( 28.45312500061451289, 0.000000000000000000, 5.243569643749999010 ) ) ;
#64497 = CARTESIAN_POINT ( 'NONE',  ( 13.57500000122903572, -5.773502691896255534, -1.060575238724906372E-15 ) ) ;
#64498 = CARTESIAN_POINT ( 'NONE',  ( 18.71249999999999858, 2.886751345948126879, 4.999999999999999112 ) ) ;
#64499 = CARTESIAN_POINT ( 'NONE',  ( 26.88749999999999574, -2.886751345948129988, 4.999999999999997335 ) ) ;
#64500 = CARTESIAN_POINT ( 'NONE',  ( 3.182137239616405822, -4.123714228212172372, 2.857517440841834233 ) ) ;
#64501 = CARTESIAN_POINT ( 'NONE',  ( 6.196875000614515905, -3.027376345333610441, -5.243569643749999898 ) ) ;
#64502 = CARTESIAN_POINT ( 'NONE',  ( 18.90937500061451360, 4.541064518000418104, -2.621784821874998173 ) ) ;
#64503 = DIRECTION ( 'NONE',  ( -0.000000000000000000, -1.000000000000000000, -0.000000000000000000 ) ) ;
#64504 = ORIENTED_EDGE ( 'NONE', *, *, #21977, .F. ) ;
#64505 = CARTESIAN_POINT ( 'NONE',  ( 2.859375000614519546, 0.000000000000000000, 5.243569643749999010 ) ) ;
#64506 = CARTESIAN_POINT ( 'NONE',  ( 29.37187500061451928, 3.027376345333611329, 5.243569643749999010 ) ) ;
#64507 = CARTESIAN_POINT ( 'NONE',  ( 4.996875000614516615, 6.054752690667223547, 3.707466751127219781E-16 ) ) ;
#64508 = CARTESIAN_POINT ( 'NONE',  ( 17.36249999999999716, 2.886751345948126879, 4.999999999999999112 ) ) ;
#64509 = CARTESIAN_POINT ( 'NONE',  ( 12.96562500061451750, 3.027376345333613106, -5.243569643749998122 ) ) ;
#64510 = CARTESIAN_POINT ( 'NONE',  ( 3.586992791275801729, 3.483314903268937446, -3.919380039434936513 ) ) ;
#64511 = DIRECTION ( 'NONE',  ( 1.000000000000000000, 0.000000000000000000, -0.000000000000000000 ) ) ;
#64512 = CARTESIAN_POINT ( 'NONE',  ( 3.947751918878622757, -3.068428716296062841, 3.947751918878600108 ) ) ;
#64513 = CARTESIAN_POINT ( 'NONE',  ( 17.81250000122903288, 4.330127018922192761, -2.499999999999997780 ) ) ;
#64514 = CARTESIAN_POINT ( 'NONE',  ( -2.000000000000001776, 19.49374999877096570, 33.46410161513775705 ) ) ;
#64515 = CARTESIAN_POINT ( 'NONE',  ( 17.25937500061451502, 0.000000000000000000, 4.756430356249998326 ) ) ;
#64516 = CARTESIAN_POINT ( 'NONE',  ( 7.490625000614516082, -3.027376345333610441, -5.243569643749999898 ) ) ;
#64517 = CARTESIAN_POINT ( 'NONE',  ( 24.72187500061451360, 3.027376345333613106, -5.243569643749998122 ) ) ;
#64518 = CARTESIAN_POINT ( 'NONE',  ( 2.121784821875001281, 19.10937500061451644, 33.67503911421598417 ) ) ;
#64519 = CARTESIAN_POINT ( 'NONE',  ( 23.52187500061451786, 3.027376345333611329, 5.243569643749999010 ) ) ;
#64520 = CARTESIAN_POINT ( 'NONE',  ( 5.287500000000000533, -2.886751345948129988, 4.999999999999997335 ) ) ;
#64521 = CARTESIAN_POINT ( 'NONE',  ( 2.000000000000001332, 11.71250000122903501, 33.46410161513774995 ) ) ;
#64522 = CARTESIAN_POINT ( 'NONE',  ( 14.54062500061451679, -3.027376345333614438, 5.243569643749998122 ) ) ;
#64523 = CARTESIAN_POINT ( 'NONE',  ( 4.650000001229035895, -2.886751345948125991, -5.000000000000000000 ) ) ;
#64524 = CARTESIAN_POINT ( 'NONE',  ( 10.13437500061451679, -4.541064518000419881, 2.621784821874995952 ) ) ;
#64525 = CARTESIAN_POINT ( 'NONE',  ( 4.000000000000000000, 14.90000000122903323, 32.30940107675849760 ) ) ;
#64526 = VERTEX_POINT ( 'NONE', #46370 ) ;
#64527 = CARTESIAN_POINT ( 'NONE',  ( 13.52812500061451750, 4.541064518000418104, 2.621784821874999949 ) ) ;
#64528 = CARTESIAN_POINT ( 'NONE',  ( 3.422429900546629877, -3.645130117820770455, -3.769356580772429410 ) ) ;
#64529 = CARTESIAN_POINT ( 'NONE',  ( 23.21250000122903501, 4.330127018922192761, -2.499999999999997780 ) ) ;
#64530 = CARTESIAN_POINT ( 'NONE',  ( 11.29687500061451644, 6.054752690667223547, 3.707466751127219781E-16 ) ) ;
#64531 = CARTESIAN_POINT ( 'NONE',  ( 11.57812500061451644, 6.421520780324663323E-16, -5.243569643749999010 ) ) ;
#64532 = CARTESIAN_POINT ( 'NONE',  ( 27.24375000122903145, 5.773502691896255534, 3.535250795749688894E-16 ) ) ;
#64533 = CARTESIAN_POINT ( 'NONE',  ( 24.00937500061451502, 0.000000000000000000, 5.243569643749999010 ) ) ;
#64534 = CARTESIAN_POINT ( 'NONE',  ( 0.000000000000000000, 20.00000000000000000, -30.00000000000000000 ) ) ;
#64535 = DIRECTION ( 'NONE',  ( 1.000000000000000000, 0.000000000000000000, 0.000000000000000000 ) ) ;
#64536 = VECTOR ( 'NONE', #63020, 1000.000000000000000 ) ;
#64537 = CARTESIAN_POINT ( 'NONE',  ( 20.47500000122903074, 2.886751345948162850, -4.999999999999940492 ) ) ;
#64538 = CARTESIAN_POINT ( 'NONE',  ( -3.000416591977282496E-16, 13.89687500061451608, -34.90005215228797653 ) ) ;
#64539 = CARTESIAN_POINT ( 'NONE',  ( 16.95937500061451786, -4.541064518000417216, -2.621784821875001281 ) ) ;
#64540 = CARTESIAN_POINT ( 'NONE',  ( 16.80000000122903359, -2.886751345948125991, -5.000000000000000000 ) ) ;
#64541 = CARTESIAN_POINT ( 'NONE',  ( 12.57187500061451857, 3.027376345333613106, -5.243569643749998122 ) ) ;
#64542 = CARTESIAN_POINT ( 'NONE',  ( -4.243569643749997233, 16.69062500061451360, -27.54997392385601174 ) ) ;
#64543 = CARTESIAN_POINT ( 'NONE',  ( 19.80000000122903359, -2.886751345948129988, 4.999999999999997335 ) ) ;
#64544 = CARTESIAN_POINT ( 'NONE',  ( 12.66562500061451502, 3.027376345333611329, 5.243569643749999010 ) ) ;
#64545 = VERTEX_POINT ( 'NONE', #11308 ) ;
#64546 = ORIENTED_EDGE ( 'NONE', *, *, #16678, .F. ) ;
#64547 = CARTESIAN_POINT ( 'NONE',  ( 15.48749999999999893, 5.773502691896255534, 3.535250795749688894E-16 ) ) ;
#64548 = CYLINDRICAL_SURFACE ( 'NONE', #29107, 4.999999999999998224 ) ;
#64549 = CARTESIAN_POINT ( 'NONE',  ( 11.59687500061451892, -3.027376345333610441, -5.243569643749999898 ) ) ;
#64550 = FACE_OUTER_BOUND ( 'NONE', #16802, .T. ) ;
#64551 = EDGE_CURVE ( 'NONE', #72719, #46824, #28650, .T. ) ;
#64552 = CARTESIAN_POINT ( 'NONE',  ( 12.41250000122903430, 4.330127018922192761, -2.499999999999997780 ) ) ;
#64553 = CARTESIAN_POINT ( 'NONE',  ( 20.06250000122903643, 4.330127018922192761, -2.499999999999997780 ) ) ;
#64554 = EDGE_CURVE ( 'NONE', #36412, #72350, #34183, .T. ) ;
#64555 = CARTESIAN_POINT ( 'NONE',  ( 17.72812500061451502, -4.541064518000419881, 2.621784821874995952 ) ) ;
#64556 =( BOUNDED_CURVE ( )  B_SPLINE_CURVE ( 2, ( #65625, #32013, #49743, #54548, #21282, #38277, #61537 ),
 .UNSPECIFIED., .F., .F. ) 
 B_SPLINE_CURVE_WITH_KNOTS ( ( 3, 2, 2, 3 ),
 ( 0.7500000000000000000, 0.7533333333333332993, 0.7566666666666667096, 0.7600000000000000089 ),
 .UNSPECIFIED. ) 
 CURVE ( )  GEOMETRIC_REPRESENTATION_ITEM ( )  RATIONAL_B_SPLINE_CURVE ( ( 1.000000000000000000, 0.8660254037844387076, 1.000000000000000000, 0.8660254037844387076, 1.000000000000000000, 0.8660254037844387076, 1.000000000000000000 ) ) 
 REPRESENTATION_ITEM ( '' )  );
#64557 = CARTESIAN_POINT ( 'NONE',  ( 20.01562500061451644, -6.054752690667223547, -1.112240025338166033E-15 ) ) ;
#64558 = CARTESIAN_POINT ( 'NONE',  ( 27.97500000122903074, -5.773502691896255534, -1.060575238724906372E-15 ) ) ;
#64559 = CARTESIAN_POINT ( 'NONE',  ( 25.46249999999999858, 2.886751345948126879, 4.999999999999999112 ) ) ;
#64560 = CARTESIAN_POINT ( 'NONE',  ( 5.857864376269049878, -9.999999999999992895, 5.857864376269049878 ) ) ;
#64561 = CARTESIAN_POINT ( 'NONE',  ( 7.846875000614518036, -2.746126346562646425, 4.756430356249996549 ) ) ;
#64562 = CARTESIAN_POINT ( 'NONE',  ( 28.92187500061451644, 3.027376345333611329, 5.243569643749999010 ) ) ;
#64563 = LINE ( 'NONE', #13218, #22874 ) ;
#64564 = CARTESIAN_POINT ( 'NONE',  ( -2.121784821874999949, 12.58437500061451786, -33.67503911421598417 ) ) ;
#64565 = CARTESIAN_POINT ( 'NONE',  ( 4.462500001229035007, 0.000000000000000000, 4.999999999999998224 ) ) ;
#64566 = CARTESIAN_POINT ( 'NONE',  ( 4.837500000000001243, -2.886751345948129988, 4.999999999999997335 ) ) ;
#64567 = CARTESIAN_POINT ( 'NONE',  ( 0.000000000000000000, 27.50000000000000000, 26.00000000000000000 ) ) ;
#64568 = CARTESIAN_POINT ( 'NONE',  ( 7.996875000614519280, -3.027376345333610441, -5.243569643749999898 ) ) ;
#64569 = CARTESIAN_POINT ( 'NONE',  ( 28.04062500061451502, -3.027376345333614438, 5.243569643749998122 ) ) ;
#64570 = FACE_OUTER_BOUND ( 'NONE', #4929, .T. ) ;
#64571 = CARTESIAN_POINT ( 'NONE',  ( -1.587936087009578445, 9.880963660774179758, -35.79978921151577964 ) ) ;
#64572 = CARTESIAN_POINT ( 'NONE',  ( 16.83750000122903145, 6.123233995736764310E-16, -4.999999999999998224 ) ) ;
#64573 = CARTESIAN_POINT ( 'NONE',  ( 5.596875000614516260, -3.027376345333614438, 5.243569643749998122 ) ) ;
#64574 = CARTESIAN_POINT ( 'NONE',  ( 11.59687500061451892, -3.027376345333610441, -5.243569643749999898 ) ) ;
#64575 = CARTESIAN_POINT ( 'NONE',  ( 4.612500000000002487, 2.886751345948129099, -4.999999999999998224 ) ) ;
#64576 = CARTESIAN_POINT ( 'NONE',  ( 2.121784821875001281, 15.00312500061459353, 33.67503911421598417 ) ) ;
#64577 = EDGE_CURVE ( 'NONE', #50518, #43273, #51398, .T. ) ;
#64578 = CARTESIAN_POINT ( 'NONE',  ( 2.441552069295954475, 25.34000229536805548, 33.17907134633756527 ) ) ;
#64579 = CARTESIAN_POINT ( 'NONE',  ( 6.862500000000002487, 2.886751345948129099, -4.999999999999998224 ) ) ;
#64580 = CARTESIAN_POINT ( 'NONE',  ( 15.83437500061451253, -2.746126346562646425, 4.756430356249996549 ) ) ;
#64581 = CARTESIAN_POINT ( 'NONE',  ( 20.12812500061451715, 6.421520780324663323E-16, -5.243569643749999010 ) ) ;
#64582 = CARTESIAN_POINT ( 'NONE',  ( 12.21562500061451573, 3.027376345333611329, 5.243569643749999010 ) ) ;
#64583 = CARTESIAN_POINT ( 'NONE',  ( 23.07187500061451502, -4.119189519843968306, 2.378215178124996054 ) ) ;
#64584 = CARTESIAN_POINT ( 'NONE',  ( 10.58437500061451964, -4.541064518000419881, 2.621784821874995952 ) ) ;
#64585 = CARTESIAN_POINT ( 'NONE',  ( 25.23749999999999716, -2.886751345948125991, -5.000000000000000000 ) ) ;
#64586 = CARTESIAN_POINT ( 'NONE',  ( 22.23750000122903003, 6.123233995736764310E-16, -4.999999999999998224 ) ) ;
#64587 = CARTESIAN_POINT ( 'NONE',  ( 1.999999999999998668, 10.96250000122903501, 26.53589838486224650 ) ) ;
#64588 = CARTESIAN_POINT ( 'NONE',  ( 9.609375000614518214, 0.000000000000000000, 5.243569643749999010 ) ) ;
#64589 = CARTESIAN_POINT ( 'NONE',  ( 27.57187500061451857, 3.027376345333611329, 5.243569643749999010 ) ) ;
#64590 = CARTESIAN_POINT ( 'NONE',  ( 23.25000000000000000, 0.000000000000000000, 4.999999999999998224 ) ) ;
#64591 = LINE ( 'NONE', #36155, #39590 ) ;
#64592 = CARTESIAN_POINT ( 'NONE',  ( 19.58437500061451786, -4.541064518000419881, 2.621784821874995952 ) ) ;
#64593 =( BOUNDED_CURVE ( )  B_SPLINE_CURVE ( 2, ( #47958, #25787, #31324, #2167, #70115, #7336, #47586, #64936, #14327 ),
 .UNSPECIFIED., .F., .F. ) 
 B_SPLINE_CURVE_WITH_KNOTS ( ( 3, 2, 2, 2, 3 ),
 ( 0.03260869565217391908, 0.03623188405797101580, 0.04347826086956521618, 0.05072463768115942351, 0.05434782608695652717 ),
 .UNSPECIFIED. ) 
 CURVE ( )  GEOMETRIC_REPRESENTATION_ITEM ( )  RATIONAL_B_SPLINE_CURVE ( ( 0.9330127018922192983, 0.9330127018922194093, 1.000000000000000000, 0.8660254037844387076, 1.000000000000000000, 0.8660254037844387076, 1.000000000000000000, 0.9330127018922192983, 0.9330127018922194093 ) ) 
 REPRESENTATION_ITEM ( '' )  );
#64594 = CARTESIAN_POINT ( 'NONE',  ( 12.94687500061451857, -3.027376345333610441, -5.243569643749999898 ) ) ;
#64595 = CARTESIAN_POINT ( 'NONE',  ( -3.756430356250000102, 19.72812499938548214, 30.00000000000000000 ) ) ;
#64596 = CARTESIAN_POINT ( 'NONE',  ( 24.07499999999999929, 4.330127018922191873, 2.499999999999999556 ) ) ;
#64597 = CARTESIAN_POINT ( 'NONE',  ( 4.000000000000000000, 15.68750000000000000, 27.69059892324149530 ) ) ;
#64598 = CARTESIAN_POINT ( 'NONE',  ( 4.243569643749999898, 12.88437500061451857, -30.00000000000000000 ) ) ;
#64599 = CARTESIAN_POINT ( 'NONE',  ( 24.72187500061451360, 2.746126346562645981, -4.756430356249997438 ) ) ;
#64600 = CARTESIAN_POINT ( 'NONE',  ( 15.17812500061451608, 6.421520780324663323E-16, -5.243569643749999010 ) ) ;
#64601 = CARTESIAN_POINT ( 'NONE',  ( 4.200000000000001954, 4.330127018922192761, -2.499999999999997780 ) ) ;
#64602 = CARTESIAN_POINT ( 'NONE',  ( 25.08749999999999858, -2.886751345948130876, 4.999999999999996447 ) ) ;
#64603 = DIRECTION ( 'NONE',  ( -1.000000000000000000, -0.000000000000000000, -0.000000000000000000 ) ) ;
#64604 =( BOUNDED_CURVE ( )  B_SPLINE_CURVE ( 2, ( #22081, #33888, #16172, #56071, #33168, #49806, #66425, #28353, #290 ),
 .UNSPECIFIED., .F., .F. ) 
 B_SPLINE_CURVE_WITH_KNOTS ( ( 3, 2, 2, 2, 3 ),
 ( 0.5108695652173913526, 0.5144927536231883591, 0.5217391304347825942, 0.5289855072463768293, 0.5326086956521739468 ),
 .UNSPECIFIED. ) 
 CURVE ( )  GEOMETRIC_REPRESENTATION_ITEM ( )  RATIONAL_B_SPLINE_CURVE ( ( 0.9330127018922192983, 0.9330127018922202975, 1.000000000000000000, 0.8660254037844387076, 1.000000000000000000, 0.8660254037844387076, 1.000000000000000000, 0.9330127018922194093, 0.9330127018922194093 ) ) 
 REPRESENTATION_ITEM ( '' )  );
#64605 = CARTESIAN_POINT ( 'NONE',  ( 11.21250000000000036, -5.773502691896255534, -1.060575238724906372E-15 ) ) ;
#64606 = CARTESIAN_POINT ( 'NONE',  ( 1.999999999999998668, 17.26250000122903572, 26.53589838486224650 ) ) ;
#64607 = CARTESIAN_POINT ( 'NONE',  ( 13.83750000122903323, 4.330127018922191873, 2.499999999999999556 ) ) ;
#64608 = CARTESIAN_POINT ( 'NONE',  ( 24.60937500061451644, -4.541064518000417216, -2.621784821875001281 ) ) ;
#64609 = CARTESIAN_POINT ( 'NONE',  ( 16.95937500061451786, -4.541064518000417216, -2.621784821875001281 ) ) ;
#64610 = DIRECTION ( 'NONE',  ( -1.000000000000000000, -0.000000000000000000, -0.000000000000000000 ) ) ;
#64611 = ORIENTED_EDGE ( 'NONE', *, *, #30682, .F. ) ;
#64612 = CARTESIAN_POINT ( 'NONE',  ( 19.11562500061451431, -6.054752690667223547, -1.112240025338166033E-15 ) ) ;
#64613 = CARTESIAN_POINT ( 'NONE',  ( 5.128125000614516260, -4.541064518000419881, 2.621784821874995952 ) ) ;
#64614 = CARTESIAN_POINT ( 'NONE',  ( 18.49687500061452283, 6.054752690667223547, 3.707466751127219781E-16 ) ) ;
#64615 = CARTESIAN_POINT ( 'NONE',  ( 28.69687500061451502, -3.027376345333610441, -5.243569643749999898 ) ) ;
#64616 = CARTESIAN_POINT ( 'NONE',  ( 4.790625000614518569, -3.027376345333610441, -5.243569643749999898 ) ) ;
#64617 = CARTESIAN_POINT ( 'NONE',  ( 22.41562500061451502, 3.027376345333613106, -5.243569643749998122 ) ) ;
#64618 = CARTESIAN_POINT ( 'NONE',  ( 2.121784821875001281, 15.45312500061451644, 33.67503911421598417 ) ) ;
#64619 = CARTESIAN_POINT ( 'NONE',  ( 16.16250000122903430, 0.000000000000000000, 4.999999999999998224 ) ) ;
#64620 = CARTESIAN_POINT ( 'NONE',  ( 12.75937500061451857, 0.000000000000000000, 4.756430356249998326 ) ) ;
#64621 = CARTESIAN_POINT ( 'NONE',  ( 7.415625000614516793, -6.054752690667223547, -1.112240025338166033E-15 ) ) ;
#64622 = CARTESIAN_POINT ( 'NONE',  ( 27.75000000000000000, 0.000000000000000000, 4.999999999999998224 ) ) ;
#64623 = CARTESIAN_POINT ( 'NONE',  ( 29.76562500061451644, 3.027376345333611329, 5.243569643749999010 ) ) ;
#64624 = CARTESIAN_POINT ( 'NONE',  ( 22.05937500061451573, 4.541064518000418104, -2.621784821874998173 ) ) ;
#64625 = CARTESIAN_POINT ( 'NONE',  ( 14.69062500061451537, -3.027376345333610441, -5.243569643749999898 ) ) ;
#64626 = CARTESIAN_POINT ( 'NONE',  ( 25.31250000122903288, -4.330127018922190985, -2.500000000000001332 ) ) ;
#64627 =( BOUNDED_CURVE ( )  B_SPLINE_CURVE ( 2, ( #52130, #29950, #19580, #52490, #64662, #14047, #24405 ),
 .UNSPECIFIED., .F., .T. ) 
 B_SPLINE_CURVE_WITH_KNOTS ( ( 3, 2, 2, 3 ),
 ( 0.1599999999999999756, 0.1633333333333333026, 0.1666666666666666019, 0.1699999999999999567 ),
 .UNSPECIFIED. ) 
 CURVE ( )  GEOMETRIC_REPRESENTATION_ITEM ( )  RATIONAL_B_SPLINE_CURVE ( ( 1.000000000000001332, 0.8660254037844377084, 1.000000000000000000, 0.8660254037844387076, 1.000000000000000000, 0.8660254037844409281, 0.9999999999999977796 ) ) 
 REPRESENTATION_ITEM ( '' )  );
#64628 = CARTESIAN_POINT ( 'NONE',  ( 25.34062500061451217, -3.027376345333614438, 5.243569643749998122 ) ) ;
#64629 = CARTESIAN_POINT ( 'NONE',  ( 20.07187500061451857, -6.054752690667223547, -1.112240025338166033E-15 ) ) ;
#64630 = CARTESIAN_POINT ( 'NONE',  ( 14.35312500061451679, 4.541064518000418104, -2.621784821874998173 ) ) ;
#64631 = CARTESIAN_POINT ( 'NONE',  ( -3.000416591977282496E-16, 13.89687500061451786, 25.09994784771203058 ) ) ;
#64632 = CARTESIAN_POINT ( 'NONE',  ( 20.69062500061451715, 6.054752690667223547, 3.707466751127219781E-16 ) ) ;
#64633 = CARTESIAN_POINT ( 'NONE',  ( 28.56562500061451715, -6.054752690667223547, -1.112240025338166033E-15 ) ) ;
#64634 = ORIENTED_EDGE ( 'NONE', *, *, #21313, .F. ) ;
#64635 = CARTESIAN_POINT ( 'NONE',  ( 26.09999999999999787, -4.330127018922190985, -2.500000000000001332 ) ) ;
#64636 = CARTESIAN_POINT ( 'NONE',  ( 3.999999999999998668, 10.81250000000000178, -32.30940107675850470 ) ) ;
#64637 = CARTESIAN_POINT ( 'NONE',  ( 16.08749999999999858, -2.886751345948130876, 4.999999999999996447 ) ) ;
#64638 = CARTESIAN_POINT ( 'NONE',  ( 26.69062500061451715, -3.027376345333614438, 5.243569643749998122 ) ) ;
#64639 = CARTESIAN_POINT ( 'NONE',  ( 8.053125000614516082, 4.541064518000418104, -2.621784821874998173 ) ) ;
#64640 = CARTESIAN_POINT ( 'NONE',  ( 19.87500000122903288, -5.773502691896255534, -1.060575238724906372E-15 ) ) ;
#64641 = AXIS2_PLACEMENT_3D ( 'NONE', #56613, #6369, #34073 ) ;
#64642 = CARTESIAN_POINT ( 'NONE',  ( 25.67812500061451431, 4.541064518000418104, 2.621784821874999949 ) ) ;
#64643 = CARTESIAN_POINT ( 'NONE',  ( 26.36249999999999716, 2.886751345948126879, 4.999999999999999112 ) ) ;
#64644 = ADVANCED_FACE ( 'NONE', ( #57441 ), #39384, .F. ) ;
#64645 = CARTESIAN_POINT ( 'NONE',  ( 28.67812500061451431, 6.421520780324663323E-16, -5.243569643749999010 ) ) ;
#64646 = CARTESIAN_POINT ( 'NONE',  ( 9.178125000614517859, -4.541064518000419881, 2.621784821874995952 ) ) ;
#64647 = EDGE_LOOP ( 'NONE', ( #63811, #27187, #18354, #34163 ) ) ;
#64648 = CARTESIAN_POINT ( 'NONE',  ( 24.51562500061451289, -6.054752690667223547, -1.112240025338166033E-15 ) ) ;
#64649 = CARTESIAN_POINT ( 'NONE',  ( 4.453125000614517326, 4.541064518000418104, -2.621784821874998173 ) ) ;
#64650 = CARTESIAN_POINT ( 'NONE',  ( 13.39687500061451608, -2.746126346562642428, -4.756430356249999214 ) ) ;
#64651 = CARTESIAN_POINT ( 'NONE',  ( 3.478125000614517237, 6.421520780324663323E-16, -5.243569643749999010 ) ) ;
#64652 = CYLINDRICAL_SURFACE ( 'NONE', #7861, 3.999999999999996447 ) ;
#64653 = CARTESIAN_POINT ( 'NONE',  ( 13.79999999999999893, 0.000000000000000000, 4.999999999999998224 ) ) ;
#64654 = CARTESIAN_POINT ( 'NONE',  ( 13.13437500061451857, 4.541064518000418104, 2.621784821874999949 ) ) ;
#64655 = CARTESIAN_POINT ( 'NONE',  ( 8.812500001229034652, 4.330127018922192761, -2.499999999999997780 ) ) ;
#64656 = CARTESIAN_POINT ( 'NONE',  ( 16.43437500061451573, -4.541064518000419881, 2.621784821874995952 ) ) ;
#64657 = CARTESIAN_POINT ( 'NONE',  ( 15.22500000000000142, -4.330127018922194537, 2.499999999999995559 ) ) ;
#64658 = CARTESIAN_POINT ( 'NONE',  ( 7.696875000614516793, 6.054752690667223547, 3.707466751127219781E-16 ) ) ;
#64659 = CARTESIAN_POINT ( 'NONE',  ( -4.243569643749997233, 11.29062500061451857, -27.54997392385601174 ) ) ;
#64660 = CYLINDRICAL_SURFACE ( 'NONE', #6461, 4.999999999999998224 ) ;
#64661 = CARTESIAN_POINT ( 'NONE',  ( 24.19687500061451502, 4.119189519843966529, -2.378215178124998275 ) ) ;
#64662 = CARTESIAN_POINT ( 'NONE',  ( 26.25000000000000000, 4.330127018922192761, -2.499999999999997780 ) ) ;
#64663 = CARTESIAN_POINT ( 'NONE',  ( 24.89062500061451644, -3.027376345333614438, 5.243569643749998122 ) ) ;
#64664 = CARTESIAN_POINT ( 'NONE',  ( -1.473772837211104303, 9.872922166578582903, 25.95083099200021692 ) ) ;
#64665 = CARTESIAN_POINT ( 'NONE',  ( 21.22500000122903074, -5.773502691896255534, -1.060575238724906372E-15 ) ) ;
#64666 = CARTESIAN_POINT ( 'NONE',  ( 27.15937500061451360, 0.000000000000000000, 5.243569643749999010 ) ) ;
#64667 = CARTESIAN_POINT ( 'NONE',  ( 27.90937500061451715, 4.541064518000418104, -2.621784821874998173 ) ) ;
#64668 = ADVANCED_FACE ( 'NONE', ( #18261 ), #40834, .F. ) ;
#64669 = CARTESIAN_POINT ( 'NONE',  ( 3.478125000614517237, 6.421520780324663323E-16, -5.243569643749999010 ) ) ;
#64670 = CARTESIAN_POINT ( 'NONE',  ( 21.34687500061451715, -4.119189519843965641, -2.378215178125001383 ) ) ;
#64671 = CARTESIAN_POINT ( 'NONE',  ( 16.02187500061451786, -6.054752690667223547, -1.112240025338166033E-15 ) ) ;
#64672 = CARTESIAN_POINT ( 'NONE',  ( 8.409375000614515372, 2.746126346562645981, -4.756430356249997438 ) ) ;
#64673 = CARTESIAN_POINT ( 'NONE',  ( 28.83750000122903145, -4.330127018922194537, 2.499999999999995559 ) ) ;
#64674 = CARTESIAN_POINT ( 'NONE',  ( 6.571875000614517681, -6.054752690667223547, -1.112240025338166033E-15 ) ) ;
#64675 = CARTESIAN_POINT ( 'NONE',  ( 15.75937500061451857, 4.541064518000418104, -2.621784821874998173 ) ) ;
#64676 = CARTESIAN_POINT ( 'NONE',  ( -2.646227255512634713, 25.30407769034638576, 26.98922086287628019 ) ) ;
#64677 = CARTESIAN_POINT ( 'NONE',  ( 26.55000000000000071, -4.330127018922190985, -2.500000000000001332 ) ) ;
#64678 = CARTESIAN_POINT ( 'NONE',  ( 26.70937500061451431, 0.000000000000000000, 5.243569643749999010 ) ) ;
#64679 = CARTESIAN_POINT ( 'NONE',  ( -1.243387493232115393E-14, 15.76249999999999929, 26.00000000000000000 ) ) ;
#64680 = CARTESIAN_POINT ( 'NONE',  ( 29.77499999999999858, 6.123233995736764310E-16, -4.999999999999998224 ) ) ;
#64681 = VERTEX_POINT ( 'NONE', #35273 ) ;
#64682 = CARTESIAN_POINT ( 'NONE',  ( 8.962500000000002132, -5.773502691896255534, -1.060575238724906372E-15 ) ) ;
#64683 = CARTESIAN_POINT ( 'NONE',  ( 8.296875000614518214, -4.119189519843965641, -2.378215178125001383 ) ) ;
#64684 = CARTESIAN_POINT ( 'NONE',  ( 22.64062500061451644, -3.027376345333614438, 5.243569643749998122 ) ) ;
#64685 = CARTESIAN_POINT ( 'NONE',  ( 12.93750000000000178, -2.886751345948129988, 4.999999999999997335 ) ) ;
#64686 = CARTESIAN_POINT ( 'NONE',  ( 8.887500001229033941, 4.330127018922191873, 2.499999999999999556 ) ) ;
#64687 = CARTESIAN_POINT ( 'NONE',  ( 7.640625000614517326, 6.054752690667223547, 3.707466751127219781E-16 ) ) ;
#64688 = CARTESIAN_POINT ( 'NONE',  ( 22.27499999999999858, 4.330127018922191873, 2.499999999999999556 ) ) ;
#64689 = CARTESIAN_POINT ( 'NONE',  ( 19.04062500061451146, -3.027376345333614438, 5.243569643749998122 ) ) ;
#64690 = CARTESIAN_POINT ( 'NONE',  ( 4.837500001229035895, 4.330127018922191873, 2.499999999999999556 ) ) ;
#64691 = CARTESIAN_POINT ( 'NONE',  ( 25.01250000122903216, 4.330127018922192761, -2.499999999999997780 ) ) ;
#64692 = CARTESIAN_POINT ( 'NONE',  ( 3.756430356250000102, 18.94062499938548427, 30.00000000000000000 ) ) ;
#64693 = CARTESIAN_POINT ( 'NONE',  ( 5.400000000000002132, -4.330127018922190985, -2.500000000000001332 ) ) ;
#64694 = EDGE_LOOP ( 'NONE', ( #8746, #65677, #68712, #34234 ) ) ;
#64695 = CARTESIAN_POINT ( 'NONE',  ( 19.56562500061451715, -6.054752690667223547, -1.112240025338166033E-15 ) ) ;
#64696 = CARTESIAN_POINT ( 'NONE',  ( 26.42812500061451431, 6.421520780324663323E-16, -5.243569643749999010 ) ) ;
#64697 = CARTESIAN_POINT ( 'NONE',  ( 26.40937500061451715, -4.541064518000417216, -2.621784821875001281 ) ) ;
#64698 = CARTESIAN_POINT ( 'NONE',  ( 9.000000000000001776, -4.330127018922190985, -2.500000000000001332 ) ) ;
#64699 = CARTESIAN_POINT ( 'NONE',  ( 10.79062500061451679, 6.054752690667223547, 3.707466751127219781E-16 ) ) ;
#64700 = CARTESIAN_POINT ( 'NONE',  ( 28.52812500061451573, -4.541064518000419881, 2.621784821874995952 ) ) ;
#64701 = CARTESIAN_POINT ( 'NONE',  ( 8.165625000614516793, 3.027376345333611329, 5.243569643749999010 ) ) ;
#64702 = CARTESIAN_POINT ( 'NONE',  ( 14.08125000122903181, 6.123233995736764310E-16, -4.999999999999998224 ) ) ;
#64703 = CARTESIAN_POINT ( 'NONE',  ( -4.243569643749999898, 12.20937500061451608, 30.00000000000000000 ) ) ;
#64704 = CARTESIAN_POINT ( 'NONE',  ( 24.56250000122903288, 4.330127018922192761, -2.499999999999997780 ) ) ;
#64705 = CARTESIAN_POINT ( 'NONE',  ( 19.24687500061452283, -2.746126346562641984, -4.756430356249999214 ) ) ;
#64706 = CARTESIAN_POINT ( 'NONE',  ( 14.42812500061451786, 4.541064518000418104, 2.621784821874999949 ) ) ;
#64707 = CARTESIAN_POINT ( 'NONE',  ( 11.37187500061451750, 3.027376345333611329, 5.243569643749999010 ) ) ;
#64708 = CARTESIAN_POINT ( 'NONE',  ( 10.39687500061451786, 6.054752690667223547, 3.707466751127219781E-16 ) ) ;
#64709 = CARTESIAN_POINT ( 'NONE',  ( 17.07187500061451502, 3.027376345333613106, -5.243569643749998122 ) ) ;
#64710 = EDGE_LOOP ( 'NONE', ( #49080, #39660, #30292, #65743 ) ) ;
#64711 = CARTESIAN_POINT ( 'NONE',  ( -2.699902572705014769, 9.635935948006316920, 35.37283348364390179 ) ) ;
#64712 = CARTESIAN_POINT ( 'NONE',  ( 20.84062500061451573, -3.027376345333614438, 5.243569643749998122 ) ) ;
#64713 = CARTESIAN_POINT ( 'NONE',  ( 16.24687500061451573, 6.054752690667223547, 3.707466751127219781E-16 ) ) ;
#64714 = CARTESIAN_POINT ( 'NONE',  ( 22.97812500061451857, 4.541064518000418104, 2.621784821874999949 ) ) ;
#64715 = CARTESIAN_POINT ( 'NONE',  ( -2.000000000000000000, 13.17500000000000071, 26.53589838486224650 ) ) ;
#64716 = CARTESIAN_POINT ( 'NONE',  ( 27.81562500061452070, 3.027376345333613106, -5.243569643749998122 ) ) ;
#64717 = CARTESIAN_POINT ( 'NONE',  ( 7.725000001229034297, -5.773502691896255534, -1.060575238724906372E-15 ) ) ;
#64718 = ORIENTED_EDGE ( 'NONE', *, *, #58187, .F. ) ;
#64719 = CARTESIAN_POINT ( 'NONE',  ( 5.625000001229036428, 2.886751345948129099, -4.999999999999998224 ) ) ;
#64720 = CARTESIAN_POINT ( 'NONE',  ( -2.828200636599751609E-16, 17.18750000000000000, -34.61880215351700230 ) ) ;
#64721 = CARTESIAN_POINT ( 'NONE',  ( 25.16250000122903074, 0.000000000000000000, 4.999999999999998224 ) ) ;
#64722 = CARTESIAN_POINT ( 'NONE',  ( -3.756430356249999214, 12.94062499938548250, 27.83122392262697531 ) ) ;
#64723 = CARTESIAN_POINT ( 'NONE',  ( 7.696875000614516793, 6.054752690667223547, 3.707466751127219781E-16 ) ) ;
#64724 = DIRECTION ( 'NONE',  ( -1.000000000000000000, -0.000000000000000000, -0.000000000000000000 ) ) ;
#64725 = CARTESIAN_POINT ( 'NONE',  ( 15.06562500061451537, -6.054752690667223547, -1.112240025338166033E-15 ) ) ;
#64726 = CARTESIAN_POINT ( 'NONE',  ( 9.009375000614518569, 4.541064518000418104, -2.621784821874998173 ) ) ;
#64727 = CARTESIAN_POINT ( 'NONE',  ( 28.01250000122903216, -4.330127018922190985, -2.500000000000001332 ) ) ;
#64728 = CARTESIAN_POINT ( 'NONE',  ( 17.37187500061451573, -6.054752690667223547, -1.112240025338166033E-15 ) ) ;
#64729 = CARTESIAN_POINT ( 'NONE',  ( 4.134375000614517681, 4.541064518000418104, 2.621784821874999949 ) ) ;
#64730 = CYLINDRICAL_SURFACE ( 'NONE', #55696, 4.999999999999998224 ) ;
#64731 = CARTESIAN_POINT ( 'NONE',  ( 6.365625000614518747, 3.027376345333611329, 5.243569643749999010 ) ) ;
#64732 = CARTESIAN_POINT ( 'NONE',  ( 15.59062500061451573, -3.027376345333610441, -5.243569643749999898 ) ) ;
#64733 = ORIENTED_EDGE ( 'NONE', *, *, #15774, .T. ) ;
#64734 = CARTESIAN_POINT ( 'NONE',  ( 13.34062500061451750, -3.027376345333610441, -5.243569643749999898 ) ) ;
#64735 = CARTESIAN_POINT ( 'NONE',  ( 5.175000001229033586, 2.886751345948129099, -4.999999999999998224 ) ) ;
#64736 = CARTESIAN_POINT ( 'NONE',  ( 10.15312500061451750, -4.541064518000417216, -2.621784821875001281 ) ) ;
#64737 = CARTESIAN_POINT ( 'NONE',  ( 21.87187500061451573, -5.492252693125287522, -1.008910452111647106E-15 ) ) ;
#64738 = CARTESIAN_POINT ( 'NONE',  ( 9.975000000000001421, 6.123233995736764310E-16, -4.999999999999998224 ) ) ;
#64739 = CARTESIAN_POINT ( 'NONE',  ( 5.737500001229033586, 4.330127018922191873, 2.499999999999999556 ) ) ;
#64740 = CARTESIAN_POINT ( 'NONE',  ( 19.57500000000000284, 4.330127018922191873, 2.499999999999999556 ) ) ;
#64741 = CARTESIAN_POINT ( 'NONE',  ( 13.92187500061451644, 3.027376345333613106, -5.243569643749998122 ) ) ;
#64742 = CARTESIAN_POINT ( 'NONE',  ( 16.68750000122903288, -4.330127018922194537, 2.499999999999995559 ) ) ;
#64743 = CARTESIAN_POINT ( 'NONE',  ( 22.23750000000000071, 5.773502691896255534, 3.535250795749688894E-16 ) ) ;
#64744 = CARTESIAN_POINT ( 'NONE',  ( -2.121784821874999949, 9.884375000614518569, -33.67503911421598417 ) ) ;
#64745 = CARTESIAN_POINT ( 'NONE',  ( 3.205315561573065963, 3.837448607643382026, 3.573382659177642751 ) ) ;
#64746 = CARTESIAN_POINT ( 'NONE',  ( 30.00000000000000000, 0.000000000000000000, 0.000000000000000000 ) ) ;
#64747 = CARTESIAN_POINT ( 'NONE',  ( 0.000000000000000000, 20.00000000000000000, -30.00000000000000000 ) ) ;
#64748 = CARTESIAN_POINT ( 'NONE',  ( 0.000000000000000000, 20.00000000000000000, 30.00000000000000000 ) ) ;
#64749 = CARTESIAN_POINT ( 'NONE',  ( 18.61875000122903145, 2.886751345948073588, -5.000000000000094147 ) ) ;
#64750 = CARTESIAN_POINT ( 'NONE',  ( 16.62187500061451573, 3.027376345333613106, -5.243569643749998122 ) ) ;
#64751 = CARTESIAN_POINT ( 'NONE',  ( 28.19999999999999929, 0.000000000000000000, 4.999999999999998224 ) ) ;
#64752 = EDGE_CURVE ( 'NONE', #3427, #65794, #34340, .T. ) ;
#64753 = CARTESIAN_POINT ( 'NONE',  ( 10.79062500061451679, 6.054752690667223547, 3.707466751127219781E-16 ) ) ;
#64754 = CARTESIAN_POINT ( 'NONE',  ( 29.29687500061451644, 0.000000000000000000, 4.756430356249998326 ) ) ;
#64755 = CARTESIAN_POINT ( 'NONE',  ( 22.77187500061451786, -6.054752690667223547, -1.112240025338166033E-15 ) ) ;
#64756 = CARTESIAN_POINT ( 'NONE',  ( 14.89687500061451608, 0.000000000000000000, 4.756430356249998326 ) ) ;
#64757 = CARTESIAN_POINT ( 'NONE',  ( 10.64062500061451644, -3.027376345333610441, -5.243569643749999898 ) ) ;
#64758 = CARTESIAN_POINT ( 'NONE',  ( 14.93437500061451750, 4.541064518000418104, 2.621784821874999949 ) ) ;
#64759 = ORIENTED_EDGE ( 'NONE', *, *, #47041, .T. ) ;
#64760 = CARTESIAN_POINT ( 'NONE',  ( 26.93437500061451573, 6.421520780324663323E-16, -5.243569643749999010 ) ) ;
#64761 = CARTESIAN_POINT ( 'NONE',  ( 27.32812500061451644, 6.421520780324663323E-16, -5.243569643749999010 ) ) ;
#64762 = CARTESIAN_POINT ( 'NONE',  ( 28.07812500061451289, -4.541064518000419881, 2.621784821874995952 ) ) ;
#64763 = CARTESIAN_POINT ( 'NONE',  ( 4.874144969157243601, 1.114769402001472676, -5.123700985539431763 ) ) ;
#64764 = CARTESIAN_POINT ( 'NONE',  ( 6.337499999999998579, -2.886751345948125991, -5.000000000000000000 ) ) ;
#64765 = CARTESIAN_POINT ( 'NONE',  ( 16.68750000122903288, -4.330127018922194537, 2.499999999999995559 ) ) ;
#64766 = CARTESIAN_POINT ( 'NONE',  ( 45.00000000000000000, 0.000000000000000000, 4.999999999999998224 ) ) ;
#64767 = CARTESIAN_POINT ( 'NONE',  ( 7.959375000614516082, 2.746126346562645981, -4.756430356249997438 ) ) ;
#64768 = ORIENTED_EDGE ( 'NONE', *, *, #57914, .F. ) ;
#64769 = CARTESIAN_POINT ( 'NONE',  ( 14.21249999999999858, 2.886751345948126879, 4.999999999999999112 ) ) ;
#64770 = CARTESIAN_POINT ( 'NONE',  ( 19.65000000000000213, 0.000000000000000000, 4.999999999999998224 ) ) ;
#64771 = CARTESIAN_POINT ( 'NONE',  ( 14.05312500061451431, 0.000000000000000000, 5.243569643749999010 ) ) ;
#64772 = ORIENTED_EDGE ( 'NONE', *, *, #62833, .F. ) ;
#64773 = CARTESIAN_POINT ( 'NONE',  ( 28.49999999999999645, 4.330127018922192761, -2.499999999999997780 ) ) ;
#64774 = CARTESIAN_POINT ( 'NONE',  ( 2.121784821874999061, 16.55937500061451573, -33.67503911421598417 ) ) ;
#64775 = CARTESIAN_POINT ( 'NONE',  ( 5.315625000614516260, 3.027376345333613106, -5.243569643749998122 ) ) ;
#64776 = CARTESIAN_POINT ( 'NONE',  ( 13.31250000000000178, 2.886751345948126879, 4.999999999999999112 ) ) ;
#64777 = CARTESIAN_POINT ( 'NONE',  ( 28.54687500061451644, -4.119189519843965641, -2.378215178125001383 ) ) ;
#64778 = ORIENTED_EDGE ( 'NONE', *, *, #45135, .F. ) ;
#64779 = CARTESIAN_POINT ( 'NONE',  ( -3.000416591977282496E-16, 16.09062500061451573, 25.09994784771203058 ) ) ;
#64780 = CARTESIAN_POINT ( 'NONE',  ( 25.56562500061452070, 3.027376345333613106, -5.243569643749998122 ) ) ;
#64781 = CARTESIAN_POINT ( 'NONE',  ( 7.500000000000000000, 0.000000000000000000, 4.999999999999998224 ) ) ;
#64782 = CARTESIAN_POINT ( 'NONE',  ( 1.878215178125000495, 16.76562499938548356, 26.74683588394047007 ) ) ;
#64783 = CARTESIAN_POINT ( 'NONE',  ( 23.40937500061451715, 4.541064518000418104, -2.621784821874998173 ) ) ;
#64784 = CARTESIAN_POINT ( 'NONE',  ( 22.15312500061451573, 0.000000000000000000, 5.243569643749999010 ) ) ;
#64785 = CARTESIAN_POINT ( 'NONE',  ( -4.243569643749999898, 14.40312500061459389, -30.00000000000000000 ) ) ;
#64786 = CARTESIAN_POINT ( 'NONE',  ( 24.15000000122903145, 5.773502691896255534, 3.535250795749688894E-16 ) ) ;
#64787 = CARTESIAN_POINT ( 'NONE',  ( 5.840625000614516615, 6.054752690667223547, 3.707466751127219781E-16 ) ) ;
#64788 = CARTESIAN_POINT ( 'NONE',  ( 27.87187500061451573, 2.746126346562645981, -4.756430356249997438 ) ) ;
#64789 = CARTESIAN_POINT ( 'NONE',  ( 25.11562500061451431, 3.027376345333612662, -5.243569643749998122 ) ) ;
#64790 = CARTESIAN_POINT ( 'NONE',  ( 10.73437500061451644, 5.824947211148865298E-16, -4.756430356249998326 ) ) ;
#64791 = CARTESIAN_POINT ( 'NONE',  ( 1.878215178125000495, 14.96562499938548463, 26.74683588394047007 ) ) ;
#64792 = CARTESIAN_POINT ( 'NONE',  ( 16.50937500061451502, -4.541064518000417216, -2.621784821875001281 ) ) ;
#64793 = CARTESIAN_POINT ( 'NONE',  ( 25.02187500061451431, -6.054752690667223547, -1.112240025338166033E-15 ) ) ;
#64794 = CARTESIAN_POINT ( 'NONE',  ( -2.121784821874999949, 13.48437500061451821, 26.32496088578401938 ) ) ;
#64795 = CARTESIAN_POINT ( 'NONE',  ( 6.178125000614518747, 6.421520780324663323E-16, -5.243569643749999010 ) ) ;
#64796 = CARTESIAN_POINT ( 'NONE',  ( 29.20312500061451644, 4.541064518000418104, -2.621784821874998173 ) ) ;
#64797 = CARTESIAN_POINT ( 'NONE',  ( 29.20312500061451644, 4.541064518000418104, -2.621784821874998173 ) ) ;
#64798 = CARTESIAN_POINT ( 'NONE',  ( -4.000000000000000000, 14.97499999999999964, 30.00000000000000000 ) ) ;
#64799 = CYLINDRICAL_SURFACE ( 'NONE', #4035, 3.999999999999996447 ) ;
#64800 = CARTESIAN_POINT ( 'NONE',  ( 29.28750000122903074, -4.330127018922194537, 2.499999999999995559 ) ) ;
#64801 = CARTESIAN_POINT ( 'NONE',  ( 8.034375000614518925, 6.421520780324663323E-16, -5.243569643749999010 ) ) ;
#64802 =( NAMED_UNIT ( * ) SI_UNIT ( $, .STERADIAN. ) SOLID_ANGLE_UNIT ( ) );
#64803 = CARTESIAN_POINT ( 'NONE',  ( 15.22500000122903252, 2.886751345948126879, 4.999999999999999112 ) ) ;
#64804 = CARTESIAN_POINT ( 'NONE',  ( 3.459375000614519635, -4.541064518000417216, -2.621784821875001281 ) ) ;
#64805 = CARTESIAN_POINT ( 'NONE',  ( 11.10000000122903252, 5.773502691896255534, 3.535250795749688894E-16 ) ) ;
#64806 = CARTESIAN_POINT ( 'NONE',  ( 4.040625000614517681, 6.054752690667223547, 3.707466751127219781E-16 ) ) ;
#64807 = CARTESIAN_POINT ( 'NONE',  ( 4.000000000000000000, 13.83124999877096606, 27.69059892324149530 ) ) ;
#64808 = CARTESIAN_POINT ( 'NONE',  ( 20.45625000122903359, 4.330127018922192761, -2.499999999999997780 ) ) ;
#64809 = CARTESIAN_POINT ( 'NONE',  ( 13.80937500061451750, -4.541064518000417216, -2.621784821875001281 ) ) ;
#64810 = CARTESIAN_POINT ( 'NONE',  ( 1.626862140677534273E-15, 17.52500000122903145, 34.00000000000000000 ) ) ;
#64811 = ORIENTED_EDGE ( 'NONE', *, *, #64818, .F. ) ;
#64812 = CARTESIAN_POINT ( 'NONE',  ( 22.56562500061451715, 3.027376345333611329, 5.243569643749999010 ) ) ;
#64813 = CARTESIAN_POINT ( 'NONE',  ( 7.828125000614517326, -4.541064518000419881, 2.621784821874995952 ) ) ;
#64814 = CARTESIAN_POINT ( 'NONE',  ( 25.54687500061451644, -3.027376345333610441, -5.243569643749999898 ) ) ;
#64815 = CARTESIAN_POINT ( 'NONE',  ( 6.590625000614518392, -3.027376345333610441, -5.243569643749999898 ) ) ;
#64816 = LINE ( 'NONE', #26030, #47404 ) ;
#64817 = CARTESIAN_POINT ( 'NONE',  ( 7.500000001229034652, 5.773502691896255534, 3.535250795749688894E-16 ) ) ;
#64818 = EDGE_CURVE ( 'NONE', #49631, #13067, #44305, .T. ) ;
#64819 = CARTESIAN_POINT ( 'NONE',  ( 25.07812500061451644, 6.421520780324663323E-16, -5.243569643749999010 ) ) ;
#64820 = CARTESIAN_POINT ( 'NONE',  ( -3.000416591977282496E-16, 11.59062500061451750, -34.90005215228797653 ) ) ;
#64821 = CARTESIAN_POINT ( 'NONE',  ( 9.337500001229033231, 4.330127018922191873, 2.499999999999999556 ) ) ;
#64822 = CARTESIAN_POINT ( 'NONE',  ( 20.31562500061451715, 3.027376345333611329, 5.243569643749999010 ) ) ;
#64823 = EDGE_CURVE ( 'NONE', #28145, #17484, #47450, .T. ) ;
#64824 = CARTESIAN_POINT ( 'NONE',  ( 17.24062500061451786, -3.027376345333614438, 5.243569643749998122 ) ) ;
#64825 = CARTESIAN_POINT ( 'NONE',  ( 29.07187500061451502, -5.492252693125287522, -1.008910452111647106E-15 ) ) ;
#64826 = CARTESIAN_POINT ( 'NONE',  ( 19.31250000000000000, -5.773502691896255534, -1.060575238724906372E-15 ) ) ;
#64827 = CARTESIAN_POINT ( 'NONE',  ( 13.53750000122903430, -4.330127018922194537, 2.499999999999995559 ) ) ;
#64828 = CARTESIAN_POINT ( 'NONE',  ( 9.853125000614516793, 4.541064518000418104, -2.621784821874998173 ) ) ;
#64829 = CARTESIAN_POINT ( 'NONE',  ( 12.92812500061451786, 6.421520780324663323E-16, -5.243569643749999010 ) ) ;
#64830 = EDGE_CURVE ( 'NONE', #31816, #70824, #64101, .T. ) ;
#64831 =( BOUNDED_CURVE ( )  B_SPLINE_CURVE ( 2, ( #35153, #63945, #45885, #46606, #28887, #34785, #12975 ),
 .UNSPECIFIED., .F., .F. ) 
 B_SPLINE_CURVE_WITH_KNOTS ( ( 3, 2, 2, 3 ),
 ( 0.5400000000000001465, 0.5433333333333333348, 0.5466666666666666341, 0.5499999999999999334 ),
 .UNSPECIFIED. ) 
 CURVE ( )  GEOMETRIC_REPRESENTATION_ITEM ( )  RATIONAL_B_SPLINE_CURVE ( ( 0.9999999999999955591, 0.8660254037844431485, 1.000000000000000000, 0.8660254037844387076, 1.000000000000000000, 0.8660254037844431485, 0.9999999999999955591 ) ) 
 REPRESENTATION_ITEM ( '' )  );
#64832 = CARTESIAN_POINT ( 'NONE',  ( 23.40000000122903145, -2.886751345948129988, 4.999999999999997335 ) ) ;
#64833 = CARTESIAN_POINT ( 'NONE',  ( 21.45937500061451786, -4.541064518000417216, -2.621784821875001281 ) ) ;
#64834 = CARTESIAN_POINT ( 'NONE',  ( 21.68437500061451573, 4.541064518000418104, 2.621784821874999949 ) ) ;
#64835 = CARTESIAN_POINT ( 'NONE',  ( 7.556250001229035007, 0.000000000000000000, 4.999999999999998224 ) ) ;
#64836 = EDGE_CURVE ( 'NONE', #10990, #11359, #33921, .T. ) ;
#64837 = CARTESIAN_POINT ( 'NONE',  ( 7.950000001229033053, 5.773502691896255534, 3.535250795749688894E-16 ) ) ;
#64838 = CARTESIAN_POINT ( 'NONE',  ( 5.671875000614519102, -6.054752690667223547, -1.112240025338166033E-15 ) ) ;
#64839 = CARTESIAN_POINT ( 'NONE',  ( 23.25937500061451857, -4.541064518000417216, -2.621784821875001281 ) ) ;
#64840 = DIRECTION ( 'NONE',  ( 0.000000000000000000, 0.000000000000000000, -1.000000000000000000 ) ) ;
#64841 = CARTESIAN_POINT ( 'NONE',  ( 17.91562500061451502, 3.027376345333613106, -5.243569643749998122 ) ) ;
#64842 = CARTESIAN_POINT ( 'NONE',  ( 24.60937500061451644, -4.541064518000417216, -2.621784821875001281 ) ) ;
#64843 = CARTESIAN_POINT ( 'NONE',  ( 1.878215178124997609, 20.32812499938548356, 33.25316411605952993 ) ) ;
#64844 = CYLINDRICAL_SURFACE ( 'NONE', #12597, 4.000000000000000000 ) ;
#64845 = CARTESIAN_POINT ( 'NONE',  ( 6.346875000614517148, 6.054752690667223547, 3.707466751127219781E-16 ) ) ;
#64846 = CARTESIAN_POINT ( 'NONE',  ( 18.21562500061451573, -6.054752690667223547, -1.112240025338166033E-15 ) ) ;
#64847 = ORIENTED_EDGE ( 'NONE', *, *, #12973, .T. ) ;
#64848 = CARTESIAN_POINT ( 'NONE',  ( 0.000000000000000000, 20.00000000000000000, 26.00000000000000000 ) ) ;
#64849 = CARTESIAN_POINT ( 'NONE',  ( 24.66562500061451502, 3.027376345333613106, -5.243569643749998122 ) ) ;
#64850 = CYLINDRICAL_SURFACE ( 'NONE', #66361, 4.999999999999998224 ) ;
#64851 = CARTESIAN_POINT ( 'NONE',  ( 45.00000000000000000, 0.000000000000000000, 4.999999999999998224 ) ) ;
#64852 = CARTESIAN_POINT ( 'NONE',  ( 14.32500000000000107, -4.330127018922194537, 2.499999999999995559 ) ) ;
#64853 = CARTESIAN_POINT ( 'NONE',  ( 25.42500000122903359, 2.886751345948129099, -4.999999999999998224 ) ) ;
#64854 = CARTESIAN_POINT ( 'NONE',  ( 22.07812500061451644, 4.541064518000418104, 2.621784821874999949 ) ) ;
#64855 = VERTEX_POINT ( 'NONE', #9028 ) ;
#64856 = CARTESIAN_POINT ( 'NONE',  ( 23.40000000000000213, -4.330127018922190985, -2.500000000000001332 ) ) ;
#64857 = CARTESIAN_POINT ( 'NONE',  ( 23.10937500061451644, 0.000000000000000000, 5.243569643749999010 ) ) ;
#64858 = ORIENTED_EDGE ( 'NONE', *, *, #5878, .T. ) ;
#64859 = FACE_OUTER_BOUND ( 'NONE', #69203, .T. ) ;
#64860 = CARTESIAN_POINT ( 'NONE',  ( 12.14062500061451821, 6.054752690667223547, 3.707466751127219781E-16 ) ) ;
#64861 = CARTESIAN_POINT ( 'NONE',  ( 3.890625000614517326, -3.027376345333610441, -5.243569643749999898 ) ) ;
#64862 = CARTESIAN_POINT ( 'NONE',  ( 17.22187500061451360, -4.119189519843968306, 2.378215178124996054 ) ) ;
#64863 = CARTESIAN_POINT ( 'NONE',  ( 25.75312500061451715, 0.000000000000000000, 5.243569643749999010 ) ) ;
#64864 = CARTESIAN_POINT ( 'NONE',  ( 12.93750000122903465, 4.330127018922191873, 2.499999999999999556 ) ) ;
#64865 = CARTESIAN_POINT ( 'NONE',  ( 18.93750000000000000, -2.886751345948125991, -5.000000000000000000 ) ) ;
#64866 = CARTESIAN_POINT ( 'NONE',  ( 26.62500000000000000, 6.123233995736764310E-16, -4.999999999999998224 ) ) ;
#64867 = CARTESIAN_POINT ( 'NONE',  ( 0.000000000000000000, 20.00000000000000000, -33.99999999999999289 ) ) ;
#64868 = CARTESIAN_POINT ( 'NONE',  ( 6.234375000614519102, 6.421520780324663323E-16, -5.243569643749999010 ) ) ;
#64869 = CARTESIAN_POINT ( 'NONE',  ( 20.03437500061451715, -4.541064518000419881, 2.621784821874995952 ) ) ;
#64870 = CARTESIAN_POINT ( 'NONE',  ( 1.999999999999998668, 11.41250000122903430, 26.53589838486224650 ) ) ;
#64871 = ORIENTED_EDGE ( 'NONE', *, *, #65098, .F. ) ;
#64872 = CARTESIAN_POINT ( 'NONE',  ( 29.35312500061451502, 0.000000000000000000, 5.243569643749999010 ) ) ;
#64873 = CARTESIAN_POINT ( 'NONE',  ( 3.075000000000001510, -4.330127018922194537, 2.499999999999995559 ) ) ;
#64874 = CARTESIAN_POINT ( 'NONE',  ( 5.821875000614519458, 3.027376345333613106, -5.243569643749998122 ) ) ;
#64875 = CARTESIAN_POINT ( 'NONE',  ( 15.26249999999999929, -5.773502691896255534, -1.060575238724906372E-15 ) ) ;
#64876 = CARTESIAN_POINT ( 'NONE',  ( 13.79062500061451502, -3.027376345333610441, -5.243569643749999898 ) ) ;
#64877 = CARTESIAN_POINT ( 'NONE',  ( 15.43125000122903323, 6.123233995736764310E-16, -4.999999999999998224 ) ) ;
#64878 = DIRECTION ( 'NONE',  ( 1.000000000000000000, 0.000000000000000000, 0.000000000000000000 ) ) ;
#64879 = DIRECTION ( 'NONE',  ( -1.000000000000000000, -0.000000000000000000, -0.000000000000000000 ) ) ;
#64880 = CARTESIAN_POINT ( 'NONE',  ( 18.93750000122903288, -4.330127018922194537, 2.499999999999995559 ) ) ;
#64881 = CARTESIAN_POINT ( 'NONE',  ( 0.000000000000000000, 20.00000000000000000, 26.00000000000000000 ) ) ;
#64882 = CARTESIAN_POINT ( 'NONE',  ( 16.47187500061452070, -5.492252693125287522, -1.008910452111647106E-15 ) ) ;
#64883 = CARTESIAN_POINT ( 'NONE',  ( 8.578125000614518214, 4.541064518000418104, 2.621784821874999949 ) ) ;
#64884 = CARTESIAN_POINT ( 'NONE',  ( 23.40937500061451715, 4.541064518000418104, -2.621784821874998173 ) ) ;
#64885 = CARTESIAN_POINT ( 'NONE',  ( 2.121784821874999061, 17.90937500061451715, 26.32496088578401583 ) ) ;
#64886 = CARTESIAN_POINT ( 'NONE',  ( 25.20937500061451431, 4.541064518000418104, -2.621784821874998173 ) ) ;
#64887 = CARTESIAN_POINT ( 'NONE',  ( 4.349999999999999645, 0.000000000000000000, 4.999999999999998224 ) ) ;
#64888 = CARTESIAN_POINT ( 'NONE',  ( -1.389182545231912203, 9.676047173952133207, 26.18324276292616304 ) ) ;
#64889 = CARTESIAN_POINT ( 'NONE',  ( 13.41562500061451502, 3.027376345333613106, -5.243569643749998122 ) ) ;
#64890 = CARTESIAN_POINT ( 'NONE',  ( 3.600000001229033408, -2.886751345948129988, 4.999999999999997335 ) ) ;
#64891 = CARTESIAN_POINT ( 'NONE',  ( 8.484375000614518214, 6.421520780324663323E-16, -5.243569643749999010 ) ) ;
#64892 = CARTESIAN_POINT ( 'NONE',  ( 3.999999999999998668, 14.97500000122903252, 27.69059892324149530 ) ) ;
#64893 = EDGE_LOOP ( 'NONE', ( #70037, #69313, #69817, #21188 ) ) ;
#64894 = CARTESIAN_POINT ( 'NONE',  ( 10.37812500061451715, 4.541064518000418104, 2.621784821874999949 ) ) ;
#64895 = CARTESIAN_POINT ( 'NONE',  ( 13.73437500061451821, -4.541064518000419881, 2.621784821874995952 ) ) ;
#64896 = CARTESIAN_POINT ( 'NONE',  ( 13.79999999999999893, 0.000000000000000000, 4.999999999999998224 ) ) ;
#64897 = CARTESIAN_POINT ( 'NONE',  ( 24.86250000122903359, -4.330127018922190985, -2.500000000000001332 ) ) ;
#64898 = CARTESIAN_POINT ( 'NONE',  ( 10.50937500061451679, 0.000000000000000000, 5.243569643749999010 ) ) ;
#64899 = CARTESIAN_POINT ( 'NONE',  ( 12.55312500061451786, 4.541064518000418104, -2.621784821874998173 ) ) ;
#64900 = CARTESIAN_POINT ( 'NONE',  ( 28.33125000122903359, -4.330127018922194537, 2.499999999999995559 ) ) ;
#64901 = CARTESIAN_POINT ( 'NONE',  ( 21.75937500061451502, 0.000000000000000000, 5.243569643749999010 ) ) ;
#64902 = LINE ( 'NONE', #36830, #66737 ) ;
#64903 = CARTESIAN_POINT ( 'NONE',  ( 26.23125000122903216, 6.123233995736764310E-16, -4.999999999999998224 ) ) ;
#64904 = CARTESIAN_POINT ( 'NONE',  ( 4.898587196589411843E-16, 20.00000000000000000, -26.00000000000000000 ) ) ;
#64905 = CARTESIAN_POINT ( 'NONE',  ( 4.243569643749999010, 13.82187500061451857, -32.45002607614398471 ) ) ;
#64906 = CARTESIAN_POINT ( 'NONE',  ( 15.30937500061451750, 4.541064518000418104, -2.621784821874998173 ) ) ;
#64907 = CARTESIAN_POINT ( 'NONE',  ( 17.85000000122903430, 5.773502691896255534, 3.535250795749688894E-16 ) ) ;
#64908 = CARTESIAN_POINT ( 'NONE',  ( 11.18437500061451928, 6.421520780324663323E-16, -5.243569643749999010 ) ) ;
#64909 = CARTESIAN_POINT ( 'NONE',  ( -4.243569643749999898, 17.51562500061451644, -32.45002607614398471 ) ) ;
#64910 = CARTESIAN_POINT ( 'NONE',  ( 18.71250000122903145, 4.330127018922192761, -2.499999999999997780 ) ) ;
#64911 = CARTESIAN_POINT ( 'NONE',  ( 11.65312500061451573, 4.541064518000418104, -2.621784821874998173 ) ) ;
#64912 = ORIENTED_EDGE ( 'NONE', *, *, #2338, .T. ) ;
#64913 = CARTESIAN_POINT ( 'NONE',  ( 15.33750000000000036, -2.886751345948125991, -5.000000000000000000 ) ) ;
#64914 = CARTESIAN_POINT ( 'NONE',  ( 19.23750000122903714, 4.330127018922191873, 2.499999999999999556 ) ) ;
#64915 = CARTESIAN_POINT ( 'NONE',  ( 10.65937500061451715, -4.541064518000417216, -2.621784821875001281 ) ) ;
#64916 = CARTESIAN_POINT ( 'NONE',  ( 30.00000000000000000, 0.000000000000000000, 0.000000000000000000 ) ) ;
#64917 = CARTESIAN_POINT ( 'NONE',  ( 12.00000000122903465, 5.773502691896255534, 3.535250795749688894E-16 ) ) ;
#64918 = CARTESIAN_POINT ( 'NONE',  ( 21.60000000122903430, -2.886751345948129988, 4.999999999999997335 ) ) ;
#64919 = CARTESIAN_POINT ( 'NONE',  ( 18.44062500061451715, 6.054752690667223547, 3.707466751127219781E-16 ) ) ;
#64920 = EDGE_CURVE ( 'NONE', #33359, #32339, #6088, .T. ) ;
#64921 = CARTESIAN_POINT ( 'NONE',  ( 21.47812500061451502, 6.421520780324663323E-16, -5.243569643749999010 ) ) ;
#64922 = CARTESIAN_POINT ( 'NONE',  ( 28.38750000122903216, -4.330127018922194537, 2.499999999999995559 ) ) ;
#64923 = CARTESIAN_POINT ( 'NONE',  ( 25.27499999999999858, 6.123233995736764310E-16, -4.999999999999998224 ) ) ;
#64924 = DIRECTION ( 'NONE',  ( 1.000000000000000000, 0.000000000000000000, 0.000000000000000000 ) ) ;
#64925 = CARTESIAN_POINT ( 'NONE',  ( 28.83749999999999858, -2.886751345948125991, -5.000000000000000000 ) ) ;
#64926 = CARTESIAN_POINT ( 'NONE',  ( 29.07187500061451502, -6.054752690667223547, -1.112240025338166033E-15 ) ) ;
#64927 = CARTESIAN_POINT ( 'NONE',  ( 11.62500000000000000, -4.330127018922194537, 2.499999999999995559 ) ) ;
#64928 = CARTESIAN_POINT ( 'NONE',  ( 4.243569643749999898, 13.33437500061451786, -30.00000000000000000 ) ) ;
#64929 = CARTESIAN_POINT ( 'NONE',  ( 3.675000001229035362, -5.773502691896255534, -1.060575238724906372E-15 ) ) ;
#64930 = CARTESIAN_POINT ( 'NONE',  ( 4.425000000000001599, -4.330127018922194537, 2.499999999999995559 ) ) ;
#64931 = CARTESIAN_POINT ( 'NONE',  ( 11.96250000000000213, 2.886751345948126879, 4.999999999999998224 ) ) ;
#64932 = CARTESIAN_POINT ( 'NONE',  ( 6.459375000614518747, 0.000000000000000000, 5.243569643749999010 ) ) ;
#64933 = CARTESIAN_POINT ( 'NONE',  ( 28.71562500061451573, 3.027376345333613106, -5.243569643749998122 ) ) ;
#64934 = CARTESIAN_POINT ( 'NONE',  ( 4.633613603196540254, 1.878729617659674167, 4.895446622381335544 ) ) ;
#64935 = CARTESIAN_POINT ( 'NONE',  ( 5.475000000000000533, 6.123233995736764310E-16, -4.999999999999998224 ) ) ;
#64936 = CARTESIAN_POINT ( 'NONE',  ( -1.071796769724490117, 19.12009619066136423, 26.00000000000000000 ) ) ;
#64937 = CARTESIAN_POINT ( 'NONE',  ( 4.809375000614516615, -4.541064518000417216, -2.621784821875001281 ) ) ;
#64938 = CARTESIAN_POINT ( 'NONE',  ( 12.08437500061451608, 6.421520780324663323E-16, -5.243569643749999010 ) ) ;
#64939 = CARTESIAN_POINT ( 'NONE',  ( 4.987500000000002487, -2.886751345948125991, -5.000000000000000000 ) ) ;
#64940 = ADVANCED_FACE ( 'NONE', ( #24181 ), #70347, .T. ) ;
#64941 = CARTESIAN_POINT ( 'NONE',  ( -4.243569643749998122, 11.74062500061459424, 32.45002607614398471 ) ) ;
#64942 = CARTESIAN_POINT ( 'NONE',  ( 2.000000000000001332, 17.89999999999999858, 33.46410161513774995 ) ) ;
#64943 = CARTESIAN_POINT ( 'NONE',  ( 7.462500000000001243, 2.886751345948126879, 4.999999999999999112 ) ) ;
#64944 = CARTESIAN_POINT ( 'NONE',  ( 16.43437500061451573, -2.746126346562642428, -4.756430356249999214 ) ) ;
#64945 = CARTESIAN_POINT ( 'NONE',  ( 20.76562500061451644, 3.027376345333611329, 5.243569643749999010 ) ) ;
#64946 = CARTESIAN_POINT ( 'NONE',  ( 9.853125000614516793, 4.541064518000418104, -2.621784821874998173 ) ) ;
#64947 = CARTESIAN_POINT ( 'NONE',  ( 23.70937500061451075, 2.746126346562645981, -4.756430356249997438 ) ) ;
#64948 = CARTESIAN_POINT ( 'NONE',  ( 9.984375000614518214, 4.541064518000418104, 2.621784821874999949 ) ) ;
#64949 = CARTESIAN_POINT ( 'NONE',  ( 26.21249999999999858, 2.886751345948129099, -4.999999999999998224 ) ) ;
#64950 = CARTESIAN_POINT ( 'NONE',  ( 21.22500000122903074, -5.773502691896255534, -1.060575238724906372E-15 ) ) ;
#64951 = CARTESIAN_POINT ( 'NONE',  ( 27.51562500061451644, 3.027376345333611329, 5.243569643749999010 ) ) ;
#64952 = CARTESIAN_POINT ( 'NONE',  ( 15.41250000000000142, 2.886751345948129099, -4.999999999999997335 ) ) ;
#64953 = CARTESIAN_POINT ( 'NONE',  ( 8.859375000614518214, -4.541064518000417216, -2.621784821875001281 ) ) ;
#64954 = CARTESIAN_POINT ( 'NONE',  ( 14.85937500061451644, 4.541064518000418104, -2.621784821874998173 ) ) ;
#64955 = CARTESIAN_POINT ( 'NONE',  ( 26.22187500061451715, 3.027376345333611329, 5.243569643749999010 ) ) ;
#64956 = CARTESIAN_POINT ( 'NONE',  ( 23.71875000122902577, 2.886751345948154857, 4.999999999999951150 ) ) ;
#64957 = ADVANCED_FACE ( 'NONE', ( #31184 ), #13447, .F. ) ;
#64958 = CARTESIAN_POINT ( 'NONE',  ( 13.04999999999999893, -4.330127018922190985, -2.500000000000001332 ) ) ;
#64959 = CARTESIAN_POINT ( 'NONE',  ( 19.95937500061451786, 0.000000000000000000, 5.243569643749999010 ) ) ;
#64960 = CARTESIAN_POINT ( 'NONE',  ( 11.40937500061451892, 0.000000000000000000, 5.243569643749999010 ) ) ;
#64961 = CARTESIAN_POINT ( 'NONE',  ( -3.756430356249999214, 13.72812499938548392, 27.83122392262697531 ) ) ;
#64962 = CARTESIAN_POINT ( 'NONE',  ( 22.61250000000000071, 2.886751345948129099, -4.999999999999998224 ) ) ;
#64963 = CARTESIAN_POINT ( 'NONE',  ( 3.999999999999998668, 14.71250000000000036, 32.30940107675850470 ) ) ;
#64964 = CARTESIAN_POINT ( 'NONE',  ( -4.243569643749999898, 12.20937500061451608, -30.00000000000000000 ) ) ;
#64965 = CARTESIAN_POINT ( 'NONE',  ( 25.39687500061451431, -2.746126346562646425, 4.756430356249996549 ) ) ;
#64966 = CARTESIAN_POINT ( 'NONE',  ( 15.81562500061451537, 3.027376345333611329, 5.243569643749999010 ) ) ;
#64967 = CARTESIAN_POINT ( 'NONE',  ( 4.575000000000002842, 6.123233995736764310E-16, -4.999999999999998224 ) ) ;
#64968 = CARTESIAN_POINT ( 'NONE',  ( 13.36875000122903323, 2.886751345948126879, 4.999999999999998224 ) ) ;
#64969 = DIRECTION ( 'NONE',  ( -1.000000000000000000, -0.000000000000000000, -0.000000000000000000 ) ) ;
#64970 = CARTESIAN_POINT ( 'NONE',  ( 13.50000000000000178, -4.330127018922190985, -2.500000000000001332 ) ) ;
#64971 = CARTESIAN_POINT ( 'NONE',  ( -2.000000000000000000, 18.68750000122903288, 26.53589838486224650 ) ) ;
#64972 = CARTESIAN_POINT ( 'NONE',  ( 10.91250000122903252, -4.330127018922190985, -2.500000000000001332 ) ) ;
#64973 = CARTESIAN_POINT ( 'NONE',  ( 23.37187500061451573, 3.027376345333613106, -5.243569643749998122 ) ) ;
#64974 = CARTESIAN_POINT ( 'NONE',  ( 16.17187500061451644, 3.027376345333613106, -5.243569643749998122 ) ) ;
#64975 = FACE_OUTER_BOUND ( 'NONE', #29103, .T. ) ;
#64976 = ORIENTED_EDGE ( 'NONE', *, *, #12710, .F. ) ;
#64977 = CARTESIAN_POINT ( 'NONE',  ( 20.09062500061451573, -3.027376345333610441, -5.243569643749999898 ) ) ;
#64978 = CARTESIAN_POINT ( 'NONE',  ( 3.553125000614516082, 4.541064518000418104, -2.621784821874998173 ) ) ;
#64979 = CARTESIAN_POINT ( 'NONE',  ( 16.50937500061451502, -4.541064518000417216, -2.621784821875001281 ) ) ;
#64980 = CARTESIAN_POINT ( 'NONE',  ( 29.33437500061451431, 4.541064518000418104, 2.621784821874999949 ) ) ;
#64981 = CARTESIAN_POINT ( 'NONE',  ( 3.853125000614517681, -4.541064518000417216, -2.621784821875001281 ) ) ;
#64982 = CARTESIAN_POINT ( 'NONE',  ( 20.46562500061451928, -6.054752690667223547, -1.112240025338166033E-15 ) ) ;
#64983 = CARTESIAN_POINT ( 'NONE',  ( 2.121784821875001281, 14.55312500061451786, 33.67503911421598417 ) ) ;
#64984 = CARTESIAN_POINT ( 'NONE',  ( 15.97500000122903430, 2.886751345948129099, -4.999999999999998224 ) ) ;
#64985 = CARTESIAN_POINT ( 'NONE',  ( 11.89687500061451608, -2.746126346562646425, 4.756430356249996549 ) ) ;
#64986 = CARTESIAN_POINT ( 'NONE',  ( 6.478125000614516793, -4.541064518000419881, 2.621784821874995952 ) ) ;
#64987 = CARTESIAN_POINT ( 'NONE',  ( 3.609375000614516882, 4.541064518000418104, -2.621784821874998173 ) ) ;
#64988 = CARTESIAN_POINT ( 'NONE',  ( 8.925000000000002487, -4.330127018922194537, 2.499999999999995559 ) ) ;
#64989 =( BOUNDED_CURVE ( )  B_SPLINE_CURVE ( 2, ( #7148, #29679, #24127, #69572, #2334, #24852, #41852 ),
 .UNSPECIFIED., .F., .F. ) 
 B_SPLINE_CURVE_WITH_KNOTS ( ( 3, 2, 2, 3 ),
 ( 0.2250000000000000611, 0.2277777777777778290, 0.2305555555555555969, 0.2333333333333333648 ),
 .UNSPECIFIED. ) 
 CURVE ( )  GEOMETRIC_REPRESENTATION_ITEM ( )  RATIONAL_B_SPLINE_CURVE ( ( 0.9999999999999973355, 0.8660254037844413721, 1.000000000000000000, 0.8660254037844387076, 1.000000000000000000, 0.8660254037844373753, 1.000000000000001332 ) ) 
 REPRESENTATION_ITEM ( '' )  );
#64990 = CARTESIAN_POINT ( 'NONE',  ( 22.80937500061451573, -4.541064518000417216, -2.621784821875001281 ) ) ;
#64991 = CARTESIAN_POINT ( 'NONE',  ( 15.02812500061451750, -4.541064518000419881, 2.621784821874995952 ) ) ;
#64992 = CARTESIAN_POINT ( 'NONE',  ( 24.41250000122903430, -4.330127018922190985, -2.500000000000001332 ) ) ;
#64993 = CARTESIAN_POINT ( 'NONE',  ( 22.37812500061451360, 6.421520780324663323E-16, -5.243569643749999010 ) ) ;
#64994 = CARTESIAN_POINT ( 'NONE',  ( 19.50937500061451857, 0.000000000000000000, 5.243569643749999010 ) ) ;
#64995 = CARTESIAN_POINT ( 'NONE',  ( 13.75312500061451715, -4.541064518000417216, -2.621784821875001281 ) ) ;
#64996 = CARTESIAN_POINT ( 'NONE',  ( 2.121784821875001281, 15.50937500061451857, 33.67503911421598417 ) ) ;
#64997 = CARTESIAN_POINT ( 'NONE',  ( 19.45312500061451644, 0.000000000000000000, 5.243569643749999010 ) ) ;
#64998 = CARTESIAN_POINT ( 'NONE',  ( 10.08749999999999858, 5.773502691896255534, 3.535250795749688401E-16 ) ) ;
#64999 = ORIENTED_EDGE ( 'NONE', *, *, #30907, .T. ) ;
#65000 = ORIENTED_EDGE ( 'NONE', *, *, #66921, .F. ) ;
#65001 = CARTESIAN_POINT ( 'NONE',  ( 23.02499999999999858, 6.123233995736764310E-16, -4.999999999999998224 ) ) ;
#65002 = CARTESIAN_POINT ( 'NONE',  ( -2.000000000000000000, 10.92500000000000071, -33.46410161513775705 ) ) ;
#65003 = CYLINDRICAL_SURFACE ( 'NONE', #4341, 9.999999999999998224 ) ;
#65004 = CARTESIAN_POINT ( 'NONE',  ( 27.70312500061451289, -4.541064518000417216, -2.621784821875001281 ) ) ;
#65005 = CARTESIAN_POINT ( 'NONE',  ( 8.015625000614518214, 3.027376345333613106, -5.243569643749998122 ) ) ;
#65006 = CARTESIAN_POINT ( 'NONE',  ( 19.61250000122903359, 4.330127018922192761, -2.499999999999997780 ) ) ;
#65007 = CARTESIAN_POINT ( 'NONE',  ( 25.41562500061451146, -6.054752690667223547, -1.112240025338166033E-15 ) ) ;
#65008 = CARTESIAN_POINT ( 'NONE',  ( 25.64999999999999858, -4.330127018922190985, -2.500000000000001332 ) ) ;
#65009 = CARTESIAN_POINT ( 'NONE',  ( 26.65312500061451573, 0.000000000000000000, 5.243569643749999010 ) ) ;
#65010 = CARTESIAN_POINT ( 'NONE',  ( 8.803125000614517859, -4.541064518000417216, -2.621784821875001281 ) ) ;
#65011 = ORIENTED_EDGE ( 'NONE', *, *, #27759, .F. ) ;
#65012 = PRODUCT ( 'valve body', 'valve body', '', ( #4232 ) ) ;
#65013 = CARTESIAN_POINT ( 'NONE',  ( 23.95312500061451289, 0.000000000000000000, 5.243569643749999010 ) ) ;
#65014 = CARTESIAN_POINT ( 'NONE',  ( 4.190625000614518925, -3.027376345333614438, 5.243569643749998122 ) ) ;
#65015 = CARTESIAN_POINT ( 'NONE',  ( 13.95937500061451786, 4.119189519843966529, -2.378215178124998275 ) ) ;
#65016 = CARTESIAN_POINT ( 'NONE',  ( 3.515625000614516882, 3.027376345333613106, -5.243569643749998122 ) ) ;
#65017 = CARTESIAN_POINT ( 'NONE',  ( 13.59375000122903288, -2.886751345948237457, -4.999999999999807265 ) ) ;
#65018 = CARTESIAN_POINT ( 'NONE',  ( 9.899999999999998579, -4.330127018922190985, -2.500000000000001332 ) ) ;
#65019 = CARTESIAN_POINT ( 'NONE',  ( 10.95937500061451964, 0.000000000000000000, 5.243569643749999010 ) ) ;
#65020 = CARTESIAN_POINT ( 'NONE',  ( 9.675000001229035362, 2.886751345948129099, -4.999999999999998224 ) ) ;
#65021 = CARTESIAN_POINT ( 'NONE',  ( 14.85937500061451644, 4.541064518000418104, -2.621784821874998173 ) ) ;
#65022 = CARTESIAN_POINT ( 'NONE',  ( 14.66249999999999964, 2.886751345948126879, 4.999999999999999112 ) ) ;
#65023 = CARTESIAN_POINT ( 'NONE',  ( 5.671875000614519102, -6.054752690667223547, -1.112240025338166033E-15 ) ) ;
#65024 = FACE_OUTER_BOUND ( 'NONE', #58207, .T. ) ;
#65025 = CARTESIAN_POINT ( 'NONE',  ( 13.54687500061451999, 6.054752690667223547, 3.707466751127219781E-16 ) ) ;
#65026 = FACE_OUTER_BOUND ( 'NONE', #35851, .T. ) ;
#65027 = CARTESIAN_POINT ( 'NONE',  ( 23.05312500061451431, 0.000000000000000000, 5.243569643749999010 ) ) ;
#65028 = CARTESIAN_POINT ( 'NONE',  ( 45.00000000000000000, 0.000000000000000000, 0.000000000000000000 ) ) ;
#65029 = CARTESIAN_POINT ( 'NONE',  ( 4.000000000000000000, 20.58124999877096784, 27.69059892324149885 ) ) ;
#65030 = CARTESIAN_POINT ( 'NONE',  ( 25.39687500061451431, -3.027376345333614438, 5.243569643749998122 ) ) ;
#65031 =( BOUNDED_CURVE ( )  B_SPLINE_CURVE ( 2, ( #51233, #73041, #67509, #68232, #17596, #40155, #62675, #12069, #34592 ),
 .UNSPECIFIED., .F., .F. ) 
 B_SPLINE_CURVE_WITH_KNOTS ( ( 3, 2, 2, 2, 3 ),
 ( 0.2934782608695652439, 0.2971014492753623060, 0.3043478260869565410, 0.3115942028985507206, 0.3152173913043478382 ),
 .UNSPECIFIED. ) 
 CURVE ( )  GEOMETRIC_REPRESENTATION_ITEM ( )  RATIONAL_B_SPLINE_CURVE ( ( 0.9330127018922194093, 0.9330127018922198534, 1.000000000000000000, 0.8660254037844387076, 1.000000000000000000, 0.8660254037844387076, 1.000000000000000000, 0.9330127018922188542, 0.9330127018922194093 ) ) 
 REPRESENTATION_ITEM ( '' )  );
#65032 = CARTESIAN_POINT ( 'NONE',  ( 4.828125000614518214, 6.421520780324663323E-16, -5.243569643749999010 ) ) ;
#65033 = CARTESIAN_POINT ( 'NONE',  ( 22.69687500061451502, -4.119189519843965641, -2.378215178125001383 ) ) ;
#65034 = CARTESIAN_POINT ( 'NONE',  ( 16.24687500061451573, 6.054752690667223547, 3.707466751127219781E-16 ) ) ;
#65035 = CARTESIAN_POINT ( 'NONE',  ( 9.721875000614517148, 5.824947211148865298E-16, -4.756430356249998326 ) ) ;
#65036 = CARTESIAN_POINT ( 'NONE',  ( 27.03750000122903430, -4.330127018922194537, 2.499999999999995559 ) ) ;
#65037 = CARTESIAN_POINT ( 'NONE',  ( 6.834375000614518747, 4.541064518000418104, 2.621784821874999949 ) ) ;
#65038 = CARTESIAN_POINT ( 'NONE',  ( 17.22187500061451715, 3.027376345333611329, 5.243569643749999010 ) ) ;
#65039 = CARTESIAN_POINT ( 'NONE',  ( 21.60000000000000142, -4.330127018922190985, -2.500000000000001332 ) ) ;
#65040 = CARTESIAN_POINT ( 'NONE',  ( 25.27499999999999858, 6.123233995736764310E-16, -4.999999999999998224 ) ) ;
#65041 = EDGE_CURVE ( 'NONE', #16672, #4034, #61748, .T. ) ;
#65042 = CARTESIAN_POINT ( 'NONE',  ( 2.812500001229033320, -4.330127018922190985, -2.500000000000001332 ) ) ;
#65043 = CARTESIAN_POINT ( 'NONE',  ( 27.72187500061451715, -6.054752690667223547, -1.112240025338166033E-15 ) ) ;
#65044 = CARTESIAN_POINT ( 'NONE',  ( 1.878215178124997609, 13.57812499938548356, 33.25316411605952993 ) ) ;
#65045 = CARTESIAN_POINT ( 'NONE',  ( 21.86250000000000426, 2.886751345948126879, 4.999999999999998224 ) ) ;
#65046 = CARTESIAN_POINT ( 'NONE',  ( 7.012500000000001066, 2.886751345948126879, 4.999999999999999112 ) ) ;
#65047 = CARTESIAN_POINT ( 'NONE',  ( 9.196875000614515017, -4.119189519843965641, -2.378215178125001383 ) ) ;
#65048 = CARTESIAN_POINT ( 'NONE',  ( 23.05312500061451431, 0.000000000000000000, 5.243569643749999010 ) ) ;
#65049 = CARTESIAN_POINT ( 'NONE',  ( 11.96250000000000213, 2.886751345948126879, 4.999999999999999112 ) ) ;
#65050 = CARTESIAN_POINT ( 'NONE',  ( 5.765625000614519102, 3.027376345333613106, -5.243569643749998122 ) ) ;
#65051 = CARTESIAN_POINT ( 'NONE',  ( 19.12500000000000000, 4.330127018922191873, 2.499999999999999556 ) ) ;
#65052 = CARTESIAN_POINT ( 'NONE',  ( 18.32812500061451644, 6.421520780324663323E-16, -5.243569643749999010 ) ) ;
#65053 = CYLINDRICAL_SURFACE ( 'NONE', #38407, 3.999999999999996447 ) ;
#65054 = CARTESIAN_POINT ( 'NONE',  ( 24.00000000122902932, -2.886751345948125991, -5.000000000000000000 ) ) ;
#65055 = CARTESIAN_POINT ( 'NONE',  ( 3.756430356250000102, 19.84062499938548640, 30.00000000000000000 ) ) ;
#65056 = CARTESIAN_POINT ( 'NONE',  ( 28.43437500061451573, 4.541064518000418104, 2.621784821874999949 ) ) ;
#65057 = ORIENTED_EDGE ( 'NONE', *, *, #5869, .T. ) ;
#65058 = CARTESIAN_POINT ( 'NONE',  ( 19.04062500061451146, -3.027376345333614438, 5.243569643749998122 ) ) ;
#65059 = CARTESIAN_POINT ( 'NONE',  ( 26.39062500061451644, -3.027376345333610441, -5.243569643749999898 ) ) ;
#65060 = CARTESIAN_POINT ( 'NONE',  ( 23.97187500061451360, 3.027376345333611329, 5.243569643749999010 ) ) ;
#65061 = CARTESIAN_POINT ( 'NONE',  ( 8.062500000000000000, -5.773502691896255534, -1.060575238724906372E-15 ) ) ;
#65062 = CARTESIAN_POINT ( 'NONE',  ( 12.47812500061451502, 6.421520780324663323E-16, -5.243569643749999010 ) ) ;
#65063 = CARTESIAN_POINT ( 'NONE',  ( 26.35312500061451857, -4.541064518000417216, -2.621784821875001281 ) ) ;
#65064 = CARTESIAN_POINT ( 'NONE',  ( 18.27187500061451431, -6.054752690667223547, -1.112240025338166033E-15 ) ) ;
#65065 = CARTESIAN_POINT ( 'NONE',  ( 9.965625000614517504, 3.027376345333611329, 5.243569643749999010 ) ) ;
#65066 = CARTESIAN_POINT ( 'NONE',  ( 3.029947538045915323, -3.977363186420035834, 3.130101185692909294 ) ) ;
#65067 = CARTESIAN_POINT ( 'NONE',  ( 2.121784821875001281, 13.25937500061451857, 33.67503911421598417 ) ) ;
#65068 = CARTESIAN_POINT ( 'NONE',  ( 23.28750000122903430, 4.330127018922191873, 2.499999999999999556 ) ) ;
#65069 = CARTESIAN_POINT ( 'NONE',  ( 20.55937500061451573, -4.119189519843965641, -2.378215178125001383 ) ) ;
#65070 = CARTESIAN_POINT ( 'NONE',  ( 13.15312500061451750, 0.000000000000000000, 5.243569643749999010 ) ) ;
#65071 =( GEOMETRIC_REPRESENTATION_CONTEXT ( 3 ) GLOBAL_UNCERTAINTY_ASSIGNED_CONTEXT ( ( #52118 ) ) GLOBAL_UNIT_ASSIGNED_CONTEXT ( ( #22740, #39758, #51192 ) ) REPRESENTATION_CONTEXT ( 'NONE', 'WORKASPACE' ) );
#65072 = CARTESIAN_POINT ( 'NONE',  ( 11.22187500061451892, 3.027376345333613106, -5.243569643749998122 ) ) ;
#65073 = CARTESIAN_POINT ( 'NONE',  ( 8.896875000614517859, -3.027376345333610441, -5.243569643749999898 ) ) ;
#65074 = VERTEX_POINT ( 'NONE', #25270 ) ;
#65075 = CARTESIAN_POINT ( 'NONE',  ( -1.004196803065522836, 9.951383199219653974, 35.91870345184305080 ) ) ;
#65076 = CARTESIAN_POINT ( 'NONE',  ( 21.77812500061451928, -4.541064518000419881, 2.621784821874995952 ) ) ;
#65077 = CARTESIAN_POINT ( 'NONE',  ( 16.43437500061451573, -4.541064518000419881, 2.621784821874995952 ) ) ;
#65078 = CARTESIAN_POINT ( 'NONE',  ( 21.85312500061451502, -4.541064518000417216, -2.621784821875001281 ) ) ;
#65079 = CARTESIAN_POINT ( 'NONE',  ( -3.999999999999997335, 12.38750000000000107, 32.30940107675850470 ) ) ;
#65080 = CARTESIAN_POINT ( 'NONE',  ( 26.42812500061451431, 6.421520780324663323E-16, -5.243569643749999010 ) ) ;
#65081 = CARTESIAN_POINT ( 'NONE',  ( 6.187500001229032875, 4.330127018922191873, 2.499999999999999556 ) ) ;
#65082 = ORIENTED_EDGE ( 'NONE', *, *, #14004, .T. ) ;
#65083 = CARTESIAN_POINT ( 'NONE',  ( 29.62500000000000000, -4.330127018922194537, 2.499999999999995559 ) ) ;
#65084 = CARTESIAN_POINT ( 'NONE',  ( -2.000000000000000000, 17.67500000000000071, -33.46410161513775705 ) ) ;
#65085 = CARTESIAN_POINT ( 'NONE',  ( 25.57500000122903216, 2.886751345948126879, 4.999999999999999112 ) ) ;
#65086 = CARTESIAN_POINT ( 'NONE',  ( 3.756430356250000546, 15.49062499938548321, 27.83122392262697886 ) ) ;
#65087 = CARTESIAN_POINT ( 'NONE',  ( 7.546875000614517326, -3.027376345333610441, -5.243569643749999898 ) ) ;
#65088 = CARTESIAN_POINT ( 'NONE',  ( 23.40000000000000213, -4.330127018922190985, -2.500000000000001332 ) ) ;
#65089 = CARTESIAN_POINT ( 'NONE',  ( 15.47812500061451679, -4.541064518000419881, 2.621784821874995952 ) ) ;
#65090 = CARTESIAN_POINT ( 'NONE',  ( 7.921875000614517326, -6.054752690667223547, -1.112240025338166033E-15 ) ) ;
#65091 = EDGE_CURVE ( 'NONE', #48096, #24010, #14189, .T. ) ;
#65092 = CARTESIAN_POINT ( 'NONE',  ( 28.16250000122903074, 4.330127018922192761, -2.499999999999997780 ) ) ;
#65093 = CARTESIAN_POINT ( 'NONE',  ( 18.19687500061451502, -3.027376345333614438, 5.243569643749998122 ) ) ;
#65094 = CARTESIAN_POINT ( 'NONE',  ( 5.934375000614517504, 4.541064518000418104, 2.621784821874999949 ) ) ;
#65095 = CARTESIAN_POINT ( 'NONE',  ( 4.000000000000000000, 16.25000000122903643, 32.30940107675849760 ) ) ;
#65096 = CARTESIAN_POINT ( 'NONE',  ( 4.640625000614518214, -3.027376345333614438, 5.243569643749998122 ) ) ;
#65097 = CARTESIAN_POINT ( 'NONE',  ( 16.00312500061451715, -4.541064518000417216, -2.621784821875001281 ) ) ;
#65098 = EDGE_CURVE ( 'NONE', #41592, #66380, #6522, .T. ) ;
#65099 = VERTEX_POINT ( 'NONE', #49653 ) ;
#65100 = CARTESIAN_POINT ( 'NONE',  ( 12.55312500061451786, 4.541064518000418104, -2.621784821874998173 ) ) ;
#65101 = CARTESIAN_POINT ( 'NONE',  ( 6.337500001229033231, -4.330127018922194537, 2.499999999999995559 ) ) ;
#65102 = CARTESIAN_POINT ( 'NONE',  ( 10.64062500061451644, -3.027376345333610441, -5.243569643749999898 ) ) ;
#65103 = CARTESIAN_POINT ( 'NONE',  ( 20.33437500061451786, 4.119189519843966529, 2.378215178124999607 ) ) ;
#65104 = CARTESIAN_POINT ( 'NONE',  ( 11.66249999999999964, -5.773502691896255534, -1.060575238724906372E-15 ) ) ;
#65105 = CARTESIAN_POINT ( 'NONE',  ( 3.675000001229035362, -5.773502691896255534, -1.060575238724906372E-15 ) ) ;
#65106 = CARTESIAN_POINT ( 'NONE',  ( 20.32499999999999929, 6.123233995736764310E-16, -4.999999999999998224 ) ) ;
#65107 = CARTESIAN_POINT ( 'NONE',  ( 15.68437500061451573, 6.421520780324663323E-16, -5.243569643749999010 ) ) ;
#65108 = CARTESIAN_POINT ( 'NONE',  ( 17.06250000122903288, 0.000000000000000000, 4.999999999999998224 ) ) ;
#65109 = CARTESIAN_POINT ( 'NONE',  ( 21.63749999999999929, -2.886751345948125991, -5.000000000000000000 ) ) ;
#65110 = CARTESIAN_POINT ( 'NONE',  ( -3.000416591977282496E-16, 17.89062500061451644, -34.90005215228797653 ) ) ;
#65111 = CARTESIAN_POINT ( 'NONE',  ( 3.217156950473346377, 3.827526723824332677, 3.584008178510168730 ) ) ;
#65112 = LINE ( 'NONE', #14502, #67799 ) ;
#65113 = CARTESIAN_POINT ( 'NONE',  ( 28.94062500061452070, -3.027376345333614438, 5.243569643749998122 ) ) ;
#65114 = CARTESIAN_POINT ( 'NONE',  ( 3.999999999999998668, 10.92500000122903536, -32.30940107675850470 ) ) ;
#65115 = CARTESIAN_POINT ( 'NONE',  ( 18.65625000122902932, 4.330127018922192761, -2.499999999999997780 ) ) ;
#65116 = CARTESIAN_POINT ( 'NONE',  ( 16.13437500061451502, 6.421520780324663323E-16, -5.243569643749999010 ) ) ;
#65117 = CARTESIAN_POINT ( 'NONE',  ( 29.43750000000000000, 5.773502691896255534, 3.535250795749688894E-16 ) ) ;
#65118 = CARTESIAN_POINT ( 'NONE',  ( 12.62812500061451537, 4.541064518000418104, 2.621784821874999949 ) ) ;
#65119 = VECTOR ( 'NONE', #31487, 1000.000000000000000 ) ;
#65120 = CARTESIAN_POINT ( 'NONE',  ( 29.07187500061451502, 5.824947211148865298E-16, -4.756430356249998326 ) ) ;
#65121 = CARTESIAN_POINT ( 'NONE',  ( 24.60937500061451644, -4.541064518000417216, -2.621784821875001281 ) ) ;
#65122 = CARTESIAN_POINT ( 'NONE',  ( 16.47187500061451715, 5.824947211148865298E-16, -4.756430356249998326 ) ) ;
#65123 = CARTESIAN_POINT ( 'NONE',  ( 10.82812500061451644, 4.541064518000418104, 2.621784821874999949 ) ) ;
#65124 = CARTESIAN_POINT ( 'NONE',  ( 14.03437500061451715, 4.541064518000418104, 2.621784821874999949 ) ) ;
#65125 = ORIENTED_EDGE ( 'NONE', *, *, #43245, .F. ) ;
#65126 = CARTESIAN_POINT ( 'NONE',  ( 23.85937500061451644, 4.541064518000418104, -2.621784821874998173 ) ) ;
#65127 = CARTESIAN_POINT ( 'NONE',  ( 27.32812500061451644, 6.421520780324663323E-16, -5.243569643749999010 ) ) ;
#65128 = CARTESIAN_POINT ( 'NONE',  ( 17.11875000122903145, -5.773502691896255534, -1.060575238724906372E-15 ) ) ;
#65129 = CARTESIAN_POINT ( 'NONE',  ( 7.650000000000000355, -4.330127018922190985, -2.500000000000001332 ) ) ;
#65130 = CARTESIAN_POINT ( 'NONE',  ( 16.01250000122903216, 4.330127018922192761, -2.499999999999997780 ) ) ;
#65131 = CYLINDRICAL_SURFACE ( 'NONE', #45680, 3.999999999999996447 ) ;
#65132 = EDGE_LOOP ( 'NONE', ( #47385, #42851, #22337, #7899 ) ) ;
#65133 = CARTESIAN_POINT ( 'NONE',  ( 15.45000000000000107, 4.330127018922192761, -2.499999999999997780 ) ) ;
#65134 = CARTESIAN_POINT ( 'NONE',  ( 18.48750000000000071, -2.886751345948125991, -5.000000000000000000 ) ) ;
#65135 = CARTESIAN_POINT ( 'NONE',  ( 14.12812500061451715, -4.541064518000419881, 2.621784821874995952 ) ) ;
#65136 = ORIENTED_EDGE ( 'NONE', *, *, #61648, .T. ) ;
#65137 = CARTESIAN_POINT ( 'NONE',  ( 65.00000000000000000, -9.000000000000000000, 0.000000000000000000 ) ) ;
#65138 = CARTESIAN_POINT ( 'NONE',  ( -3.000416591977282496E-16, 17.94687500061451502, -34.90005215228797653 ) ) ;
#65139 = CARTESIAN_POINT ( 'NONE',  ( 29.43750000122903288, 6.123233995736764310E-16, -4.999999999999998224 ) ) ;
#65140 = CARTESIAN_POINT ( 'NONE',  ( -3.756430356249999214, 13.27812499938548285, 27.83122392262697176 ) ) ;
#65141 = CARTESIAN_POINT ( 'NONE',  ( 11.51250000000000107, 2.886751345948126879, 4.999999999999999112 ) ) ;
#65142 = CARTESIAN_POINT ( 'NONE',  ( 27.90937500061451715, 2.746126346562643317, 4.756430356249998326 ) ) ;
#65143 = VERTEX_POINT ( 'NONE', #37825 ) ;
#65144 = CARTESIAN_POINT ( 'NONE',  ( 2.121784821874999061, 15.15312500061451750, 26.32496088578401583 ) ) ;
#65145 = CARTESIAN_POINT ( 'NONE',  ( 26.65312500061451573, 0.000000000000000000, 5.243569643749999010 ) ) ;
#65146 = DIRECTION ( 'NONE',  ( 1.000000000000000000, 0.000000000000000000, 0.000000000000000000 ) ) ;
#65147 = CARTESIAN_POINT ( 'NONE',  ( 3.756430356250000102, 19.84062499938548640, 30.00000000000000000 ) ) ;
#65148 = CARTESIAN_POINT ( 'NONE',  ( 22.73437500061451644, -4.541064518000419881, 2.621784821874995952 ) ) ;
#65149 = CARTESIAN_POINT ( 'NONE',  ( 18.55312500061451431, 0.000000000000000000, 5.243569643749999010 ) ) ;
#65150 = CARTESIAN_POINT ( 'NONE',  ( 2.121784821875001281, 14.55312500061459424, -26.32496088578401938 ) ) ;
#65151 = CARTESIAN_POINT ( 'NONE',  ( 22.87500000122903288, 2.886751345948126879, 4.999999999999999112 ) ) ;
#65152 = CARTESIAN_POINT ( 'NONE',  ( 4.003125000614518925, 4.541064518000418104, -2.621784821874998173 ) ) ;
#65153 = CARTESIAN_POINT ( 'NONE',  ( 27.72187500061451715, -5.492252693125287522, -1.008910452111647106E-15 ) ) ;
#65154 = CARTESIAN_POINT ( 'NONE',  ( 21.51562500061451644, 3.027376345333612662, -5.243569643749998122 ) ) ;
#65155 = CARTESIAN_POINT ( 'NONE',  ( 10.17187500061451999, -5.492252693125287522, -1.008910452111647106E-15 ) ) ;
#65156 = CARTESIAN_POINT ( 'NONE',  ( 3.756430356250000102, 15.79062499938548392, 30.00000000000000000 ) ) ;
#65157 = CARTESIAN_POINT ( 'NONE',  ( 17.22187500061451715, 3.027376345333611329, 5.243569643749999010 ) ) ;
#65158 = CARTESIAN_POINT ( 'NONE',  ( 17.29687500061451999, -3.027376345333614438, 5.243569643749998122 ) ) ;
#65159 = CARTESIAN_POINT ( 'NONE',  ( 24.68437500061451573, 6.421520780324663323E-16, -5.243569643749999010 ) ) ;
#65160 = CARTESIAN_POINT ( 'NONE',  ( 2.121784821874999061, 13.40937500061451892, 26.32496088578401583 ) ) ;
#65161 = CARTESIAN_POINT ( 'NONE',  ( 4.865625000614517859, 3.027376345333613106, -5.243569643749998122 ) ) ;
#65162 = CARTESIAN_POINT ( 'NONE',  ( 28.52812500061451573, -4.541064518000419881, 2.621784821874995952 ) ) ;
#65163 = CARTESIAN_POINT ( 'NONE',  ( 28.64062500061451289, -3.027376345333610441, -5.243569643749999898 ) ) ;
#65164 = CARTESIAN_POINT ( 'NONE',  ( 3.999999999999998668, 17.41250000000000142, 32.30940107675850470 ) ) ;
#65165 = CARTESIAN_POINT ( 'NONE',  ( 3.999999999999999112, 19.77500000000000213, 30.00000000000000000 ) ) ;
#65166 = CARTESIAN_POINT ( 'NONE',  ( 3.478125000614517237, 6.421520780324663323E-16, -5.243569643749999010 ) ) ;
#65167 = CARTESIAN_POINT ( 'NONE',  ( 7.884375000614517681, -4.541064518000419881, 2.621784821874995952 ) ) ;
#65168 = SHAPE_REPRESENTATION_RELATIONSHIP ( 'NONE' , 'NONE' ,  #68023, #54116 ) ;
#65169 = CARTESIAN_POINT ( 'NONE',  ( 14.32500000122903394, 2.886751345948126879, 4.999999999999999112 ) ) ;
#65170 = CARTESIAN_POINT ( 'NONE',  ( 10.57500000122903572, 2.886751345948129099, -4.999999999999998224 ) ) ;
#65171 = CARTESIAN_POINT ( 'NONE',  ( 5.240625000614516971, -3.027376345333610441, -5.243569643749999898 ) ) ;
#65172 = CARTESIAN_POINT ( 'NONE',  ( 1.999999999999997335, 16.86874999877096570, 33.46410161513775705 ) ) ;
#65173 = CARTESIAN_POINT ( 'NONE',  ( 19.93125000122903145, 6.123233995736764310E-16, -4.999999999999998224 ) ) ;
#65174 = CARTESIAN_POINT ( 'NONE',  ( 14.33437500061451786, 6.421520780324663323E-16, -5.243569643749999010 ) ) ;
#65175 = CARTESIAN_POINT ( 'NONE',  ( 21.35625000122903216, 4.330127018922192761, -2.499999999999997780 ) ) ;
#65176 = VERTEX_POINT ( 'NONE', #15647 ) ;
#65177 = CARTESIAN_POINT ( 'NONE',  ( 23.16562500061451502, -6.054752690667223547, -1.112240025338166033E-15 ) ) ;
#65178 = CARTESIAN_POINT ( 'NONE',  ( 7.078125000614516438, 6.421520780324663323E-16, -5.243569643749999010 ) ) ;
#65179 = CARTESIAN_POINT ( 'NONE',  ( 25.50937500061451502, -4.541064518000417216, -2.621784821875001281 ) ) ;
#65180 = CARTESIAN_POINT ( 'NONE',  ( 8.653125000614515727, 0.000000000000000000, 5.243569643749999010 ) ) ;
#65181 = CYLINDRICAL_SURFACE ( 'NONE', #8497, 4.999999999999998224 ) ;
#65182 = CARTESIAN_POINT ( 'NONE',  ( 8.100000001229034297, -2.886751345948129988, 4.999999999999997335 ) ) ;
#65183 = CARTESIAN_POINT ( 'NONE',  ( 23.27812500061451573, 6.421520780324663323E-16, -5.243569643749999010 ) ) ;
#65184 = EDGE_CURVE ( 'NONE', #4034, #62113, #41478, .T. ) ;
#65185 = CARTESIAN_POINT ( 'NONE',  ( 9.001249775931846008E-16, 10.46562500061451928, -25.09994784771203058 ) ) ;
#65186 = CARTESIAN_POINT ( 'NONE',  ( 10.76250000122903572, 0.000000000000000000, 4.999999999999998224 ) ) ;
#65187 = CARTESIAN_POINT ( 'NONE',  ( 19.19062500061452070, -3.027376345333610441, -5.243569643749999898 ) ) ;
#65188 = CARTESIAN_POINT ( 'NONE',  ( 18.85312500061451502, 4.541064518000418104, -2.621784821874998173 ) ) ;
#65189 = CARTESIAN_POINT ( 'NONE',  ( 27.98437500061451289, 4.119189519843966529, 2.378215178124999607 ) ) ;
#65190 = CARTESIAN_POINT ( 'NONE',  ( 17.62500000000000000, 6.123233995736764310E-16, -4.999999999999998224 ) ) ;
#65191 = CARTESIAN_POINT ( 'NONE',  ( 14.62500000122903288, 2.886751345948129099, -4.999999999999998224 ) ) ;
#65192 = CARTESIAN_POINT ( 'NONE',  ( 11.57812500061451644, 6.421520780324663323E-16, -5.243569643749999010 ) ) ;
#65193 = CARTESIAN_POINT ( 'NONE',  ( 12.74062500061451786, -3.027376345333614438, 5.243569643749998122 ) ) ;
#65194 = CARTESIAN_POINT ( 'NONE',  ( 23.10000000122903074, -2.886751345948125991, -5.000000000000000000 ) ) ;
#65195 = CARTESIAN_POINT ( 'NONE',  ( 22.28437500061451715, -4.541064518000419881, 2.621784821874995952 ) ) ;
#65196 = CARTESIAN_POINT ( 'NONE',  ( 20.33437500061451786, 4.541064518000418104, 2.621784821874999949 ) ) ;
#65197 = CARTESIAN_POINT ( 'NONE',  ( 3.531796677802674811, 3.539267187803308179, -3.868928841707397925 ) ) ;
#65198 = CARTESIAN_POINT ( 'NONE',  ( 6.150000001229033231, 5.773502691896255534, 3.535250795749688894E-16 ) ) ;
#65199 = CARTESIAN_POINT ( 'NONE',  ( 6.834375000614518747, 4.541064518000418104, 2.621784821874999949 ) ) ;
#65200 = CARTESIAN_POINT ( 'NONE',  ( 22.47187500061451715, 3.027376345333613106, -5.243569643749998122 ) ) ;
#65201 = CARTESIAN_POINT ( 'NONE',  ( 10.49999999999999822, 4.330127018922192761, -2.499999999999997780 ) ) ;
#65202 = CARTESIAN_POINT ( 'NONE',  ( 19.56562500061451715, -6.054752690667223547, -1.112240025338166033E-15 ) ) ;
#65203 = CARTESIAN_POINT ( 'NONE',  ( 23.63437500061451502, -4.541064518000419881, 2.621784821874995952 ) ) ;
#65204 = CARTESIAN_POINT ( 'NONE',  ( 3.756430356250000546, 19.99062499938547788, 27.83122392262697886 ) ) ;
#65205 = DIRECTION ( 'NONE',  ( 0.000000000000000000, 0.000000000000000000, 1.000000000000000000 ) ) ;
#65206 = CARTESIAN_POINT ( 'NONE',  ( 4.771875000614516971, -6.054752690667223547, -1.112240025338166033E-15 ) ) ;
#65207 = CARTESIAN_POINT ( 'NONE',  ( 16.94062500061451715, -3.027376345333610441, -5.243569643749999898 ) ) ;
#65208 = CARTESIAN_POINT ( 'NONE',  ( 13.92187500061451644, 3.027376345333613106, -5.243569643749998122 ) ) ;
#65209 = ORIENTED_EDGE ( 'NONE', *, *, #42828, .F. ) ;
#65210 = CARTESIAN_POINT ( 'NONE',  ( 10.59375000122903288, 5.773502691896255534, 3.535250795749688401E-16 ) ) ;
#65211 = CARTESIAN_POINT ( 'NONE',  ( 24.10312500061451502, -4.541064518000417216, -2.621784821875001281 ) ) ;
#65212 = CARTESIAN_POINT ( 'NONE',  ( 1.999999999999998668, 13.10000000000000142, -33.46410161513775705 ) ) ;
#65213 = DIRECTION ( 'NONE',  ( -0.000000000000000000, -1.000000000000000000, -0.000000000000000000 ) ) ;
#65214 = CARTESIAN_POINT ( 'NONE',  ( 15.52500000000000036, 4.330127018922191873, 2.499999999999999556 ) ) ;
#65215 = CARTESIAN_POINT ( 'NONE',  ( 24.86250000122903359, -4.330127018922190985, -2.500000000000001332 ) ) ;
#65216 = CARTESIAN_POINT ( 'NONE',  ( 18.29062500061451502, -3.027376345333610441, -5.243569643749999898 ) ) ;
#65217 = ORIENTED_EDGE ( 'NONE', *, *, #5701, .F. ) ;
#65218 = CARTESIAN_POINT ( 'NONE',  ( 22.01249999999999574, -5.773502691896255534, -1.060575238724906372E-15 ) ) ;
#65219 = CARTESIAN_POINT ( 'NONE',  ( 24.49687500061451573, -3.027376345333614438, 5.243569643749998122 ) ) ;
#65220 = ORIENTED_EDGE ( 'NONE', *, *, #27261, .F. ) ;
#65221 = CARTESIAN_POINT ( 'NONE',  ( 19.98750000122903359, 6.123233995736764310E-16, -4.999999999999998224 ) ) ;
#65222 = CARTESIAN_POINT ( 'NONE',  ( 12.06562500061451537, 3.027376345333613106, -5.243569643749998122 ) ) ;
#65223 = CARTESIAN_POINT ( 'NONE',  ( 4.603125000614518569, 0.000000000000000000, 5.243569643749999010 ) ) ;
#65224 = CARTESIAN_POINT ( 'NONE',  ( 16.17187500061451644, 4.119189519843966529, 2.378215178124999607 ) ) ;
#65225 = CARTESIAN_POINT ( 'NONE',  ( 26.16562500061451502, 3.027376345333611329, 5.243569643749999010 ) ) ;
#65226 = CARTESIAN_POINT ( 'NONE',  ( 11.77500000122903501, -5.773502691896255534, -1.060575238724906372E-15 ) ) ;
#65227 = CARTESIAN_POINT ( 'NONE',  ( 20.36249999999999716, 2.886751345948129099, -4.999999999999998224 ) ) ;
#65228 = CARTESIAN_POINT ( 'NONE',  ( 25.61250000000000071, -5.773502691896255534, -1.060575238724906372E-15 ) ) ;
#65229 = CARTESIAN_POINT ( 'NONE',  ( 6.346875000614517148, 6.054752690667223547, 3.707466751127219781E-16 ) ) ;
#65230 = CARTESIAN_POINT ( 'NONE',  ( 17.78437500061451715, -4.541064518000419881, 2.621784821874995952 ) ) ;
#65231 = FACE_OUTER_BOUND ( 'NONE', #24089, .T. ) ;
#65232 = ORIENTED_EDGE ( 'NONE', *, *, #20108, .T. ) ;
#65233 = CARTESIAN_POINT ( 'NONE',  ( 26.16562500061451502, 3.027376345333611329, 5.243569643749999010 ) ) ;
#65234 = CARTESIAN_POINT ( 'NONE',  ( 28.13437500061451502, -4.541064518000419881, 2.621784821874995952 ) ) ;
#65235 = CARTESIAN_POINT ( 'NONE',  ( 2.971875000614517592, -6.054752690667223547, -1.112240025338166033E-15 ) ) ;
#65236 = CARTESIAN_POINT ( 'NONE',  ( 16.35000000000000142, 4.330127018922192761, -2.499999999999997780 ) ) ;
#65237 = CARTESIAN_POINT ( 'NONE',  ( 10.97812500061451679, -4.541064518000419881, 2.621784821874995952 ) ) ;
#65238 = CARTESIAN_POINT ( 'NONE',  ( 15.24375000122903323, -2.886751345948074920, 5.000000000000092371 ) ) ;
#65239 = CARTESIAN_POINT ( 'NONE',  ( 18.13125000122903074, 6.123233995736764310E-16, -4.999999999999998224 ) ) ;
#65240 = CARTESIAN_POINT ( 'NONE',  ( 28.49062500061451431, -3.027376345333614438, 5.243569643749998122 ) ) ;
#65241 = CARTESIAN_POINT ( 'NONE',  ( 19.50000000122903288, -2.886751345948125991, -5.000000000000000000 ) ) ;
#65242 = CARTESIAN_POINT ( 'NONE',  ( 19.42499999999999716, 6.123233995736764310E-16, -4.999999999999998224 ) ) ;
#65243 = CARTESIAN_POINT ( 'NONE',  ( 17.37187500061451573, -5.492252693125287522, -1.008910452111647106E-15 ) ) ;
#65244 = CARTESIAN_POINT ( 'NONE',  ( 5.278125000614516615, 6.421520780324663323E-16, -5.243569643749999010 ) ) ;
#65245 = CARTESIAN_POINT ( 'NONE',  ( 21.00937500061451857, -4.541064518000417216, -2.621784821875001281 ) ) ;
#65246 = CARTESIAN_POINT ( 'NONE',  ( -2.121784821874999949, 16.18437500061451573, 26.32496088578401938 ) ) ;
#65247 = CARTESIAN_POINT ( 'NONE',  ( 24.72187500061451360, 3.027376345333613106, -5.243569643749998122 ) ) ;
#65248 = CARTESIAN_POINT ( 'NONE',  ( 4.762499999999999289, 2.886751345948126879, 4.999999999999999112 ) ) ;
#65249 = CARTESIAN_POINT ( 'NONE',  ( 3.999999999999999112, 9.987500001229033586, 30.00000000000000000 ) ) ;
#65250 = CARTESIAN_POINT ( 'NONE',  ( 11.42812500061451608, -4.541064518000419881, 2.621784821874995952 ) ) ;
#65251 = CARTESIAN_POINT ( 'NONE',  ( 4.725000001229034297, 2.886751345948129099, -4.999999999999998224 ) ) ;
#65252 = CARTESIAN_POINT ( 'NONE',  ( 10.02187500061451964, 3.027376345333611329, 5.243569643749999010 ) ) ;
#65253 = DIRECTION ( 'NONE',  ( 0.000000000000000000, 0.000000000000000000, -1.000000000000000000 ) ) ;
#65254 = CARTESIAN_POINT ( 'NONE',  ( 9.853125000614516793, 4.541064518000418104, -2.621784821874998173 ) ) ;
#65255 = CARTESIAN_POINT ( 'NONE',  ( 13.24687500061451750, -3.027376345333614438, 5.243569643749998122 ) ) ;
#65256 = DIRECTION ( 'NONE',  ( -1.000000000000000000, -0.000000000000000000, -0.000000000000000000 ) ) ;
#65257 = CARTESIAN_POINT ( 'NONE',  ( 21.03750000122903074, 4.330127018922191873, 2.499999999999999556 ) ) ;
#65258 = CARTESIAN_POINT ( 'NONE',  ( 11.25937500061451679, 4.541064518000418104, -2.621784821874998173 ) ) ;
#65259 = CARTESIAN_POINT ( 'NONE',  ( 12.17812500061451608, 4.541064518000418104, 2.621784821874999949 ) ) ;
#65260 = EDGE_CURVE ( 'NONE', #48156, #66756, #38934, .T. ) ;
#65261 = CARTESIAN_POINT ( 'NONE',  ( 28.40625000122903288, -4.330127018922190985, -2.500000000000001332 ) ) ;
#65262 = CARTESIAN_POINT ( 'NONE',  ( 20.97187500061451715, -6.054752690667223547, -1.112240025338166033E-15 ) ) ;
#65263 = CARTESIAN_POINT ( 'NONE',  ( 45.00000000000000000, 0.000000000000000000, 0.000000000000000000 ) ) ;
#65264 = CARTESIAN_POINT ( 'NONE',  ( -1.999999999999997113, 12.08750000122903501, -26.53589838486224295 ) ) ;
#65265 = CARTESIAN_POINT ( 'NONE',  ( 3.236638147732103565, 3.811095019601020262, -3.368060042915717034 ) ) ;
#65266 = CARTESIAN_POINT ( 'NONE',  ( 4.243569643749999010, 14.72187500061451715, -32.45002607614398471 ) ) ;
#65267 = CARTESIAN_POINT ( 'NONE',  ( 14.28750000122903430, 4.330127018922191873, 2.499999999999999556 ) ) ;
#65268 =( BOUNDED_CURVE ( )  B_SPLINE_CURVE ( 2, ( #48959, #71489, #59282, #20866, #65201, #25311, #65941 ),
 .UNSPECIFIED., .F., .F. ) 
 B_SPLINE_CURVE_WITH_KNOTS ( ( 3, 2, 2, 3 ),
 ( 0.7166666666666667851, 0.7194444444444445530, 0.7222222222222222099, 0.7249999999999999778 ),
 .UNSPECIFIED. ) 
 CURVE ( )  GEOMETRIC_REPRESENTATION_ITEM ( )  RATIONAL_B_SPLINE_CURVE ( ( 0.9999999999999946709, 0.8660254037844440367, 1.000000000000000000, 0.8660254037844387076, 1.000000000000000000, 0.8660254037844387076, 1.000000000000000000 ) ) 
 REPRESENTATION_ITEM ( '' )  );
#65269 = CARTESIAN_POINT ( 'NONE',  ( 13.39687500061451608, -3.027376345333610441, -5.243569643749999898 ) ) ;
#65270 = CARTESIAN_POINT ( 'NONE',  ( -2.121784821874999949, 17.02812500061451573, -33.67503911421598417 ) ) ;
#65271 = CARTESIAN_POINT ( 'NONE',  ( 18.37500000122903288, 2.886751345948126879, 4.999999999999999112 ) ) ;
#65272 = CARTESIAN_POINT ( 'NONE',  ( 12.59062500061451573, 6.054752690667223547, 3.707466751127219781E-16 ) ) ;
#65273 = ORIENTED_EDGE ( 'NONE', *, *, #37851, .T. ) ;
#65274 = CARTESIAN_POINT ( 'NONE',  ( 14.84999999999999964, -4.330127018922190985, -2.500000000000001332 ) ) ;
#65275 = CARTESIAN_POINT ( 'NONE',  ( 19.20000000122903216, 5.773502691896255534, 3.535250795749688401E-16 ) ) ;
#65276 = CARTESIAN_POINT ( 'NONE',  ( 9.684375000614517504, -4.541064518000419881, 2.621784821874995952 ) ) ;
#65277 = CARTESIAN_POINT ( 'NONE',  ( 4.368064885651947726, -2.433106893405058813, -4.644891113268574401 ) ) ;
#65278 = CARTESIAN_POINT ( 'NONE',  ( 11.55000000122903181, 5.773502691896255534, 3.535250795749688894E-16 ) ) ;
#65279 = CARTESIAN_POINT ( 'NONE',  ( 22.01250000122903216, 0.000000000000000000, 4.999999999999998224 ) ) ;
#65280 = CARTESIAN_POINT ( 'NONE',  ( 17.91562500061451502, 3.027376345333613106, -5.243569643749998122 ) ) ;
#65281 = CARTESIAN_POINT ( 'NONE',  ( 20.99062500061451431, -3.027376345333610441, -5.243569643749999898 ) ) ;
#65282 = CARTESIAN_POINT ( 'NONE',  ( 27.45000000122903572, -2.886751345948129988, 4.999999999999997335 ) ) ;
#65283 = CARTESIAN_POINT ( 'NONE',  ( 4.265625000614517326, -6.054752690667223547, -1.112240025338166033E-15 ) ) ;
#65284 = CARTESIAN_POINT ( 'NONE',  ( 24.89999999999999858, 4.330127018922192761, -2.499999999999997780 ) ) ;
#65285 = CARTESIAN_POINT ( 'NONE',  ( 28.19999999999999929, 0.000000000000000000, 4.999999999999998224 ) ) ;
#65286 = CARTESIAN_POINT ( 'NONE',  ( 7.396875000614519635, -2.746126346562646425, 4.756430356249996549 ) ) ;
#65287 = CARTESIAN_POINT ( 'NONE',  ( 29.03437500061451715, -4.541064518000419881, 2.621784821874995952 ) ) ;
#65288 = CARTESIAN_POINT ( 'NONE',  ( 3.999999999999999112, 12.57500000000000107, -30.00000000000000000 ) ) ;
#65289 = CARTESIAN_POINT ( 'NONE',  ( 2.925000001229034918, 2.886751345948129099, -4.999999999999998224 ) ) ;
#65290 = CARTESIAN_POINT ( 'NONE',  ( 3.075000000000001510, -4.330127018922194537, 2.499999999999995559 ) ) ;
#65291 = CARTESIAN_POINT ( 'NONE',  ( -1.071796769724480347, 18.61115380933862795, 34.00000000000000711 ) ) ;
#65292 = CARTESIAN_POINT ( 'NONE',  ( 7.659375000614518036, 4.541064518000418104, -2.621784821874998173 ) ) ;
#65293 = CARTESIAN_POINT ( 'NONE',  ( 25.41562500061451146, -6.054752690667223547, -1.112240025338166033E-15 ) ) ;
#65294 = CARTESIAN_POINT ( 'NONE',  ( -3.756430356250000102, 12.97812499938548214, 30.00000000000000000 ) ) ;
#65295 = CARTESIAN_POINT ( 'NONE',  ( -2.672702088255949472E-15, 13.90624999877096890, 26.00000000000000000 ) ) ;
#65296 = FACE_OUTER_BOUND ( 'NONE', #28714, .T. ) ;
#65297 = CARTESIAN_POINT ( 'NONE',  ( 6.271875000614517859, 3.027376345333613106, -5.243569643749998122 ) ) ;
#65298 = CARTESIAN_POINT ( 'NONE',  ( 8.784375000614518925, -4.541064518000419881, 2.621784821874995952 ) ) ;
#65299 = CARTESIAN_POINT ( 'NONE',  ( 3.675000000000001155, 6.123233995736764310E-16, -4.999999999999998224 ) ) ;
#65300 = CARTESIAN_POINT ( 'NONE',  ( -3.000416591977282496E-16, 12.04062500061459495, 25.09994784771203058 ) ) ;
#65301 = CARTESIAN_POINT ( 'NONE',  ( 29.25000000000000000, -4.330127018922190985, -2.500000000000001332 ) ) ;
#65302 = CARTESIAN_POINT ( 'NONE',  ( 4.762499999999999289, 2.886751345948126879, 4.999999999999999112 ) ) ;
#65303 = ADVANCED_FACE ( 'NONE', ( #54460 ), #33016, .T. ) ;
#65304 = CARTESIAN_POINT ( 'NONE',  ( 15.27187500061451608, 4.119189519843966529, 2.378215178124999607 ) ) ;
#65305 = ORIENTED_EDGE ( 'NONE', *, *, #72200, .F. ) ;
#65306 = CARTESIAN_POINT ( 'NONE',  ( 19.34062500061451573, 6.054752690667223547, 3.707466751127219781E-16 ) ) ;
#65307 = CARTESIAN_POINT ( 'NONE',  ( 10.94062500061451537, -3.027376345333614438, 5.243569643749998122 ) ) ;
#65308 = CARTESIAN_POINT ( 'NONE',  ( 23.63437500061451502, -2.746126346562642428, -4.756430356249999214 ) ) ;
#65309 = CARTESIAN_POINT ( 'NONE',  ( 7.659375000614518036, 4.541064518000418104, -2.621784821874998173 ) ) ;
#65310 = CARTESIAN_POINT ( 'NONE',  ( 23.85000000000000142, -4.330127018922190985, -2.500000000000001332 ) ) ;
#65311 = CARTESIAN_POINT ( 'NONE',  ( 20.36250000122903359, -4.330127018922190985, -2.500000000000001332 ) ) ;
#65312 = CARTESIAN_POINT ( 'NONE',  ( 28.26562500061451289, 3.027376345333613106, -5.243569643749998122 ) ) ;
#65313 = LINE ( 'NONE', #42064, #30792 ) ;
#65314 = CARTESIAN_POINT ( 'NONE',  ( 10.62187500061451928, -6.054752690667223547, -1.112240025338166033E-15 ) ) ;
#65315 = CARTESIAN_POINT ( 'NONE',  ( 13.47187500061451537, 3.027376345333613106, -5.243569643749998122 ) ) ;
#65316 = CARTESIAN_POINT ( 'NONE',  ( 25.13437500061451502, 6.421520780324663323E-16, -5.243569643749999010 ) ) ;
#65317 = EDGE_CURVE ( 'NONE', #40213, #25827, #12400, .T. ) ;
#65318 = CARTESIAN_POINT ( 'NONE',  ( 45.00000000000000000, -2.499999999999999556, -3.499999999999999556 ) ) ;
#65319 = CARTESIAN_POINT ( 'NONE',  ( 13.98750000000000249, -2.886751345948125991, -5.000000000000000000 ) ) ;
#65320 = CARTESIAN_POINT ( 'NONE',  ( 20.10937500061451289, -4.541064518000417216, -2.621784821875001281 ) ) ;
#65321 = CARTESIAN_POINT ( 'NONE',  ( 10.47187500061451715, 3.027376345333611329, 5.243569643749999010 ) ) ;
#65322 = CARTESIAN_POINT ( 'NONE',  ( -1.878215178125001827, 19.80312499938548143, 33.25316411605952283 ) ) ;
#65323 = CARTESIAN_POINT ( 'NONE',  ( 22.72499999999999787, 4.330127018922191873, 2.499999999999999556 ) ) ;
#65324 = CARTESIAN_POINT ( 'NONE',  ( -1.999999999999999112, 14.45000000000000107, 26.53589838486224650 ) ) ;
#65325 = CARTESIAN_POINT ( 'NONE',  ( -4.243569643749999898, 10.85937500061451821, -30.00000000000000000 ) ) ;
#65326 = CARTESIAN_POINT ( 'NONE',  ( 24.75937500061451502, 4.119189519843966529, -2.378215178124998275 ) ) ;
#65327 = CARTESIAN_POINT ( 'NONE',  ( 16.04062500061451857, -3.027376345333610441, -5.243569643749999898 ) ) ;
#65328 = CARTESIAN_POINT ( 'NONE',  ( 3.750000000000000000, 4.330127018922192761, -2.499999999999997780 ) ) ;
#65329 = EDGE_CURVE ( 'NONE', #23329, #3427, #16009, .T. ) ;
#65330 = CARTESIAN_POINT ( 'NONE',  ( 13.18125000122903323, 6.123233995736764310E-16, -4.999999999999998224 ) ) ;
#65331 = DIRECTION ( 'NONE',  ( -1.000000000000000000, -0.000000000000000000, -0.000000000000000000 ) ) ;
#65332 = CARTESIAN_POINT ( 'NONE',  ( 13.23750000000000071, 5.773502691896255534, 3.535250795749688894E-16 ) ) ;
#65333 = CARTESIAN_POINT ( 'NONE',  ( 3.999999999999998668, 18.12500000122903288, 27.69059892324149175 ) ) ;
#65334 = CARTESIAN_POINT ( 'NONE',  ( 10.53750000122903252, 6.123233995736764310E-16, -4.999999999999998224 ) ) ;
#65335 = CARTESIAN_POINT ( 'NONE',  ( 22.05937500061451573, 4.541064518000418104, -2.621784821874998173 ) ) ;
#65336 = CARTESIAN_POINT ( 'NONE',  ( 16.13437500061451502, 6.421520780324663323E-16, -5.243569643749999010 ) ) ;
#65337 = CARTESIAN_POINT ( 'NONE',  ( -3.999999999999999112, 19.83125000061451715, -30.00000000000000000 ) ) ;
#65338 = ORIENTED_EDGE ( 'NONE', *, *, #32494, .T. ) ;
#65339 = CARTESIAN_POINT ( 'NONE',  ( 17.69062500061451715, -3.027376345333614438, 5.243569643749998122 ) ) ;
#65340 = CARTESIAN_POINT ( 'NONE',  ( 2.990625000614519191, -3.027376345333610441, -5.243569643749999898 ) ) ;
#65341 = CARTESIAN_POINT ( 'NONE',  ( 17.97187500061451715, 3.027376345333613106, -5.243569643749998122 ) ) ;
#65342 = CARTESIAN_POINT ( 'NONE',  ( 28.02187500061451431, 3.027376345333611329, 5.243569643749999010 ) ) ;
#65343 = CARTESIAN_POINT ( 'NONE',  ( 4.603125000614518569, 0.000000000000000000, 5.243569643749999010 ) ) ;
#65344 = CARTESIAN_POINT ( 'NONE',  ( 20.65312500061451573, 4.541064518000418104, -2.621784821874998173 ) ) ;
#65345 = CARTESIAN_POINT ( 'NONE',  ( 28.58437500061451786, -4.541064518000419881, 2.621784821874995952 ) ) ;
#65346 = CARTESIAN_POINT ( 'NONE',  ( -3.000416591977282496E-16, 12.49062500061451608, 25.09994784771203058 ) ) ;
#65347 = CARTESIAN_POINT ( 'NONE',  ( 16.61250000122903359, 0.000000000000000000, 4.999999999999998224 ) ) ;
#65348 = CARTESIAN_POINT ( 'NONE',  ( 8.896875000614517859, -2.746126346562641984, -4.756430356249999214 ) ) ;
#65349 = CARTESIAN_POINT ( 'NONE',  ( 6.965625000614518392, -6.054752690667223547, -1.112240025338166033E-15 ) ) ;
#65350 = CARTESIAN_POINT ( 'NONE',  ( 26.20312500061451644, 0.000000000000000000, 5.243569643749999010 ) ) ;
#65351 = CYLINDRICAL_SURFACE ( 'NONE', #46255, 4.000000000000000000 ) ;
#65352 = CARTESIAN_POINT ( 'NONE',  ( 23.44687500061451502, 6.054752690667223547, 3.707466751127219781E-16 ) ) ;
#65353 = CARTESIAN_POINT ( 'NONE',  ( 13.60312500061451679, 0.000000000000000000, 5.243569643749999010 ) ) ;
#65354 = CARTESIAN_POINT ( 'NONE',  ( 23.02500000122903145, -5.773502691896255534, -1.060575238724906372E-15 ) ) ;
#65355 = CARTESIAN_POINT ( 'NONE',  ( 24.17812500061451786, 6.421520780324663323E-16, -5.243569643749999010 ) ) ;
#65356 = CARTESIAN_POINT ( 'NONE',  ( 18.60937500061451644, 0.000000000000000000, 5.243569643749999010 ) ) ;
#65357 = CARTESIAN_POINT ( 'NONE',  ( 11.54062500061451857, -3.027376345333610441, -5.243569643749999898 ) ) ;
#65358 = CARTESIAN_POINT ( 'NONE',  ( 4.243569643749999010, 15.62187500061451928, 27.54997392385601174 ) ) ;
#65359 = CARTESIAN_POINT ( 'NONE',  ( 20.05312500061451431, -4.541064518000417216, -2.621784821875001281 ) ) ;
#65360 = CARTESIAN_POINT ( 'NONE',  ( 28.90312500061451217, 0.000000000000000000, 5.243569643749999010 ) ) ;
#65361 = VERTEX_POINT ( 'NONE', #21193 ) ;
#65362 = CARTESIAN_POINT ( 'NONE',  ( 22.27499999999999858, 4.330127018922191873, 2.499999999999999556 ) ) ;
#65363 = CARTESIAN_POINT ( 'NONE',  ( 4.000000000000000000, 10.73750000000000071, -27.69059892324149530 ) ) ;
#65364 = DIRECTION ( 'NONE',  ( 0.000000000000000000, 0.000000000000000000, -1.000000000000000000 ) ) ;
#65365 = CARTESIAN_POINT ( 'NONE',  ( 27.06562500061451004, 3.027376345333611329, 5.243569643749999010 ) ) ;
#65366 = CARTESIAN_POINT ( 'NONE',  ( 6.965625000614518392, -6.054752690667223547, -1.112240025338166033E-15 ) ) ;
#65367 = CARTESIAN_POINT ( 'NONE',  ( 19.35000000122903430, -2.886751345948129988, 4.999999999999997335 ) ) ;
#65368 = EDGE_CURVE ( 'NONE', #23474, #8958, #24409, .T. ) ;
#65369 = CARTESIAN_POINT ( 'NONE',  ( 25.82812500061451644, -4.541064518000419881, 2.621784821874995952 ) ) ;
#65370 = CARTESIAN_POINT ( 'NONE',  ( 22.12500000000000000, 6.123233995736764310E-16, -4.999999999999998224 ) ) ;
#65371 = CARTESIAN_POINT ( 'NONE',  ( 27.77812500061451573, 6.421520780324663323E-16, -5.243569643749999010 ) ) ;
#65372 = CARTESIAN_POINT ( 'NONE',  ( 7.453125000614516438, -4.541064518000417216, -2.621784821875001281 ) ) ;
#65373 = ORIENTED_EDGE ( 'NONE', *, *, #41825, .F. ) ;
#65374 = CARTESIAN_POINT ( 'NONE',  ( 23.87812500061451715, 4.541064518000418104, 2.621784821874999949 ) ) ;
#65375 = CARTESIAN_POINT ( 'NONE',  ( 5.428125000614517859, 4.541064518000418104, 2.621784821874999949 ) ) ;
#65376 = CARTESIAN_POINT ( 'NONE',  ( 12.90937500061451537, -4.119189519843965641, -2.378215178125001383 ) ) ;
#65377 = CARTESIAN_POINT ( 'NONE',  ( 2.990625000614519191, -3.027376345333610441, -5.243569643749999898 ) ) ;
#65378 = CARTESIAN_POINT ( 'NONE',  ( -1.999999999999997113, 13.43750000122903465, -26.53589838486224295 ) ) ;
#65379 = CARTESIAN_POINT ( 'NONE',  ( 13.44375000122903074, -2.886751345948130876, 4.999999999999996447 ) ) ;
#65380 = CARTESIAN_POINT ( 'NONE',  ( 10.27499999999999858, -4.330127018922194537, 2.499999999999995559 ) ) ;
#65381 = CARTESIAN_POINT ( 'NONE',  ( 11.63437500061451857, 6.421520780324663323E-16, -5.243569643749999010 ) ) ;
#65382 = CARTESIAN_POINT ( 'NONE',  ( 7.800000001229035362, -2.886751345948125991, -5.000000000000000000 ) ) ;
#65383 = CARTESIAN_POINT ( 'NONE',  ( 15.83437500061451608, 4.541064518000418104, 2.621784821874999949 ) ) ;
#65384 = CARTESIAN_POINT ( 'NONE',  ( 14.24999999999999822, 0.000000000000000000, 4.999999999999998224 ) ) ;
#65385 = CARTESIAN_POINT ( 'NONE',  ( 6.084375000614518747, -4.541064518000419881, 2.621784821874995952 ) ) ;
#65386 = CARTESIAN_POINT ( 'NONE',  ( 9.001249775931846008E-16, 10.01562500061451644, -25.09994784771203058 ) ) ;
#65387 = AXIS2_PLACEMENT_3D ( 'NONE', #4990, #6072, #10888 ) ;
#65388 = CYLINDRICAL_SURFACE ( 'NONE', #53659, 4.999999999999998224 ) ;
#65389 = CARTESIAN_POINT ( 'NONE',  ( 11.97187500061451892, -6.054752690667223547, -1.112240025338166033E-15 ) ) ;
#65390 = DIRECTION ( 'NONE',  ( 0.000000000000000000, 0.000000000000000000, -1.000000000000000000 ) ) ;
#65391 = CARTESIAN_POINT ( 'NONE',  ( 21.66562500061451502, 3.027376345333611329, 5.243569643749999010 ) ) ;
#65392 = CARTESIAN_POINT ( 'NONE',  ( 4.243569643749999898, 10.14687500061451786, 32.45002607614398471 ) ) ;
#65393 = CARTESIAN_POINT ( 'NONE',  ( 2.121784821874999061, 18.75312500061459531, 26.32496088578401583 ) ) ;
#65394 = CARTESIAN_POINT ( 'NONE',  ( 25.35937500061451644, 0.000000000000000000, 5.243569643749999010 ) ) ;
#65395 = CARTESIAN_POINT ( 'NONE',  ( 4.049280102667188963, 2.933370920535487425, -4.300716962760291473 ) ) ;
#65396 = CARTESIAN_POINT ( 'NONE',  ( 3.853125000614517681, -4.541064518000417216, -2.621784821875001281 ) ) ;
#65397 = AXIS2_PLACEMENT_3D ( 'NONE', #27545, #10909, #38996 ) ;
#65398 = CARTESIAN_POINT ( 'NONE',  ( 22.20937500061451786, -5.492252693125287522, -1.008910452111647106E-15 ) ) ;
#65399 = CARTESIAN_POINT ( 'NONE',  ( 13.17187500061451999, 3.027376345333611329, 5.243569643749999010 ) ) ;
#65400 = CARTESIAN_POINT ( 'NONE',  ( 8.896875000614517859, 4.119189519843966529, -2.378215178124998275 ) ) ;
#65401 = CARTESIAN_POINT ( 'NONE',  ( 28.50000000122903288, -2.886751345948125991, -5.000000000000000000 ) ) ;
#65402 = CARTESIAN_POINT ( 'NONE',  ( 5.146875000614517859, -3.027376345333614438, 5.243569643749998122 ) ) ;
#65403 = CARTESIAN_POINT ( 'NONE',  ( 17.67187500061451644, 3.027376345333611329, 5.243569643749999010 ) ) ;
#65404 = CARTESIAN_POINT ( 'NONE',  ( -1.292810628673454865, 25.48745481703416971, 33.79429592041256569 ) ) ;
#65405 = CARTESIAN_POINT ( 'NONE',  ( 24.44999999999999929, 4.330127018922192761, -2.499999999999997780 ) ) ;
#65406 = CARTESIAN_POINT ( 'NONE',  ( 4.837500001229035895, 4.330127018922191873, 2.499999999999999556 ) ) ;
#65407 = CARTESIAN_POINT ( 'NONE',  ( 26.14687500061451431, 6.054752690667223547, 3.707466751127219781E-16 ) ) ;
#65408 = CARTESIAN_POINT ( 'NONE',  ( -3.756430356250001434, 13.46562499938548285, 32.16877607737301048 ) ) ;
#65409 = CARTESIAN_POINT ( 'NONE',  ( 29.73750000000000071, -2.886751345948125991, -5.000000000000000000 ) ) ;
#65410 = CARTESIAN_POINT ( 'NONE',  ( 7.200000000000001954, -4.330127018922190985, -2.500000000000001332 ) ) ;
#65411 = CARTESIAN_POINT ( 'NONE',  ( 10.05937500061451750, -5.492252693125287522, -1.008910452111647106E-15 ) ) ;
#65412 = CARTESIAN_POINT ( 'NONE',  ( 21.40312500061451573, -4.541064518000417216, -2.621784821875001281 ) ) ;
#65413 = CARTESIAN_POINT ( 'NONE',  ( 12.71250000000000036, 2.886751345948129099, -4.999999999999998224 ) ) ;
#65414 =( BOUNDED_CURVE ( )  B_SPLINE_CURVE ( 2, ( #32832, #10662, #27659, #56098, #55731, #39107, #71996 ),
 .UNSPECIFIED., .F., .F. ) 
 B_SPLINE_CURVE_WITH_KNOTS ( ( 3, 2, 2, 3 ),
 ( 0.09999999999999995004, 0.1033333333333332771, 0.1066666666666666041, 0.1099999999999999312 ),
 .UNSPECIFIED. ) 
 CURVE ( )  GEOMETRIC_REPRESENTATION_ITEM ( )  RATIONAL_B_SPLINE_CURVE ( ( 1.000000000000002220, 0.8660254037844364872, 1.000000000000000000, 0.8660254037844387076, 1.000000000000000000, 0.8660254037844414832, 0.9999999999999972244 ) ) 
 REPRESENTATION_ITEM ( '' )  );
#65415 = EDGE_CURVE ( 'NONE', #36937, #68374, #4229, .T. ) ;
#65416 = CARTESIAN_POINT ( 'NONE',  ( 5.053125000614517859, 0.000000000000000000, 5.243569643749999010 ) ) ;
#65417 = CARTESIAN_POINT ( 'NONE',  ( 19.04999999999999716, 4.330127018922192761, -2.499999999999997780 ) ) ;
#65418 = CARTESIAN_POINT ( 'NONE',  ( 19.52812500061451573, -4.541064518000419881, 2.621784821874995952 ) ) ;
#65419 = CARTESIAN_POINT ( 'NONE',  ( 22.87500000122903288, 2.886751345948126879, 4.999999999999999112 ) ) ;
#65420 = CARTESIAN_POINT ( 'NONE',  ( -1.878215178125001827, 18.79062499938548214, 33.25316411605952283 ) ) ;
#65421 = CARTESIAN_POINT ( 'NONE',  ( 3.862500000000001155, 2.886751345948126879, 4.999999999999999112 ) ) ;
#65422 = VERTEX_POINT ( 'NONE', #65905 ) ;
#65423 = CARTESIAN_POINT ( 'NONE',  ( 18.74062500061451431, -3.027376345333610441, -5.243569643749999898 ) ) ;
#65424 = CARTESIAN_POINT ( 'NONE',  ( 24.32812500061451289, 4.541064518000418104, 2.621784821874999949 ) ) ;
#65425 = CARTESIAN_POINT ( 'NONE',  ( 23.70937500061451786, -4.541064518000417216, -2.621784821875001281 ) ) ;
#65426 = CARTESIAN_POINT ( 'NONE',  ( 9.412499999999999645, -5.773502691896255534, -1.060575238724906372E-15 ) ) ;
#65427 = CARTESIAN_POINT ( 'NONE',  ( 11.35312500061451679, 0.000000000000000000, 5.243569643749999010 ) ) ;
#65428 = CARTESIAN_POINT ( 'NONE',  ( 26.95312500061451644, 4.541064518000418104, -2.621784821874998173 ) ) ;
#65429 = CARTESIAN_POINT ( 'NONE',  ( 18.23437500061451999, -4.541064518000419881, 2.621784821874995952 ) ) ;
#65430 = CARTESIAN_POINT ( 'NONE',  ( 8.128125000614515372, 4.541064518000418104, 2.621784821874999949 ) ) ;
#65431 = CARTESIAN_POINT ( 'NONE',  ( 22.91250000000000142, -5.773502691896255534, -1.060575238724906372E-15 ) ) ;
#65432 = CARTESIAN_POINT ( 'NONE',  ( 4.243569643749999898, 10.59687500061451715, 32.45002607614398471 ) ) ;
#65433 = CARTESIAN_POINT ( 'NONE',  ( 24.03750000122903430, 6.123233995736764310E-16, -4.999999999999998224 ) ) ;
#65434 = CARTESIAN_POINT ( 'NONE',  ( 20.07187500061451857, -5.492252693125287522, -1.008910452111647106E-15 ) ) ;
#65435 = CARTESIAN_POINT ( 'NONE',  ( 15.32812500061451644, 4.541064518000418104, 2.621784821874999949 ) ) ;
#65436 = CARTESIAN_POINT ( 'NONE',  ( 9.121875000614517504, 3.027376345333611329, 5.243569643749999010 ) ) ;
#65437 = CARTESIAN_POINT ( 'NONE',  ( 6.721875000614518925, 3.027376345333613106, -5.243569643749998122 ) ) ;
#65438 = ORIENTED_EDGE ( 'NONE', *, *, #54421, .T. ) ;
#65439 = CARTESIAN_POINT ( 'NONE',  ( 29.29687500061451644, 6.054752690667223547, 3.707466751127219781E-16 ) ) ;
#65440 = CARTESIAN_POINT ( 'NONE',  ( 22.79062500061451502, -3.027376345333610441, -5.243569643749999898 ) ) ;
#65441 = CARTESIAN_POINT ( 'NONE',  ( 16.95937500061451786, -4.541064518000417216, -2.621784821875001281 ) ) ;
#65442 = CARTESIAN_POINT ( 'NONE',  ( 21.17812500061451431, 4.541064518000418104, 2.621784821874999949 ) ) ;
#65443 = CARTESIAN_POINT ( 'NONE',  ( 3.999999999999999112, 10.77500000000000213, 30.00000000000000000 ) ) ;
#65444 = AXIS2_PLACEMENT_3D ( 'NONE', #28064, #28773, #57569 ) ;
#65445 = CARTESIAN_POINT ( 'NONE',  ( 27.66562500061451146, -6.054752690667223547, -1.112240025338166033E-15 ) ) ;
#65446 = CARTESIAN_POINT ( 'NONE',  ( 7.987500001229032698, 4.330127018922191873, 2.499999999999999556 ) ) ;
#65447 = VERTEX_POINT ( 'NONE', #15285 ) ;
#65448 = CARTESIAN_POINT ( 'NONE',  ( 29.28749999999999787, -2.886751345948125991, -5.000000000000000000 ) ) ;
#65449 = CARTESIAN_POINT ( 'NONE',  ( 4.000000000000000000, 18.38749999999999929, -27.69059892324149530 ) ) ;
#65450 = CARTESIAN_POINT ( 'NONE',  ( 24.63750000122903216, 4.330127018922191873, 2.499999999999999556 ) ) ;
#65451 = CARTESIAN_POINT ( 'NONE',  ( 2.655984681222220721E-16, 15.11562499938548321, 25.66244784525396483 ) ) ;
#65452 = CARTESIAN_POINT ( 'NONE',  ( 7.884375000614517681, -4.541064518000419881, 2.621784821874995952 ) ) ;
#65453 = CARTESIAN_POINT ( 'NONE',  ( 20.49375000122903145, 5.773502691896255534, 3.535250795749688401E-16 ) ) ;
#65454 = CARTESIAN_POINT ( 'NONE',  ( 14.12812500061451715, -4.541064518000419881, 2.621784821874995952 ) ) ;
#65455 = CARTESIAN_POINT ( 'NONE',  ( 9.571875000614518569, 3.027376345333611329, 5.243569643749999010 ) ) ;
#65456 = CARTESIAN_POINT ( 'NONE',  ( 27.41250000122903430, 0.000000000000000000, 4.999999999999998224 ) ) ;
#65457 = CLOSED_SHELL ( 'NONE', ( #41666, #19708, #68201, #14121, #54911, #58593, #29653, #56735, #45259, #8386, #13765, #14129, #52831, #19028, #47994, #45841, #5966, #17309, #64957, #33767, #30642, #21800, #17132, #27070, #47350, #42352, #60819, #48169, #18756, #42083, #70101, #22596, #46252, #46043, #60662, #38659, #60169, #3139, #27990, #69969, #66109, #66251, #17388, #23787, #63066, #36658, #6338, #67131, #44776, #45948, #13297, #28585, #40854, #36547, #30311, #47929, #22954, #44228, #8593, #71206, #52581, #24043, #26572, #20548, #56825, #47580, #53597, #17669, #35201, #62304, #62153, #4799, #71669, #32797, #49020, #47721, #3812, #44864, #23406, #20387, #45415, #52323, #11268, #52661, #551, #63085, #61773, #57923, #14846, #71593, #49614, #6499, #67108, #56234, #40997, #36232, #62741, #52239, #113, #35482, #2159, #59378, #30029, #56419, #14459, #50043, #47487, #43593, #4227, #36882, #72771, #12578, #6639, #7981, #25535, #2294, #59653, #12462, #49128, #39569, #37666, #29501, #48586, #46311, #17842, #278, #49773, #31664, #22905, #13624, #60458, #18927, #44023, #6217, #52768, #11904, #4372, #43848, #9826, #70737, #6389, #64668, #13504, #72861, #52683, #38757, #39847, #6863, #50830, #18915, #61336, #28438, #1768, #66694, #66827, #23713, #36383, #50179, #48328, #314, #62004, #19547, #67105, #51206, #40006, #63998, #28988, #4328, #70009, #67944, #55039, #51361, #24686, #50827, #983, #64644, #55344, #50413, #20, #51047, #23932, #70599, #33895, #16942, #10696, #60400, #246, #57127, #39021, #61795, #13524, #29479, #43692, #5339, #71937, #53234, #11615, #45683, #23564, #71677, #34898, #52812, #6883, #22109, #11397, #39505, #46914, #20244, #2059, #59069, #6549, #51838, #2573, #23779, #37321, #16050, #65617, #64014, #66670, #42460, #52514, #21887, #9313, #71450, #23286, #49637, #70064, #34293, #21886, #10235, #44081, #45765, #58040, #68770, #12134, #51477, #53153, #7675, #58092, #51571, #70785, #55935, #42070, #24746, #801, #34627, #31107, #12435, #18534, #52015, #57496, #27394, #62508, #56867, #17066, #70671, #40161, #68286, #61658, #29148, #15873, #39419, #1303, #69565, #40074, #44067, #51161, #21132, #49227 ) ) ;
#65458 = CARTESIAN_POINT ( 'NONE',  ( 17.78437500061451715, -4.541064518000419881, 2.621784821874995952 ) ) ;
#65459 = CARTESIAN_POINT ( 'NONE',  ( 5.221875000614519813, -6.054752690667223547, -1.112240025338166033E-15 ) ) ;
#65460 = DIRECTION ( 'NONE',  ( 0.000000000000000000, 0.000000000000000000, 1.000000000000000000 ) ) ;
#65461 = CARTESIAN_POINT ( 'NONE',  ( 4.453125000614517326, 4.541064518000418104, -2.621784821874998173 ) ) ;
#65462 = CARTESIAN_POINT ( 'NONE',  ( 16.45312500061451289, -4.541064518000417216, -2.621784821875001281 ) ) ;
#65463 = ORIENTED_EDGE ( 'NONE', *, *, #71959, .F. ) ;
#65464 = CARTESIAN_POINT ( 'NONE',  ( 12.74062500061451786, -3.027376345333614438, 5.243569643749998122 ) ) ;
#65465 = CARTESIAN_POINT ( 'NONE',  ( 5.325000001229033941, 2.886751345948126879, 4.999999999999999112 ) ) ;
#65466 = AXIS2_PLACEMENT_3D ( 'NONE', #7063, #35492, #41054 ) ;
#65467 = CARTESIAN_POINT ( 'NONE',  ( 11.76562500061451644, 3.027376345333611329, 5.243569643749999010 ) ) ;
#65468 = CARTESIAN_POINT ( 'NONE',  ( 21.23437500061451644, 4.119189519843966529, 2.378215178124999607 ) ) ;
#65469 = CARTESIAN_POINT ( 'NONE',  ( 11.73750000000000249, -2.886751345948125991, -5.000000000000000000 ) ) ;
#65470 = EDGE_CURVE ( 'NONE', #28698, #53581, #14922, .T. ) ;
#65471 = CARTESIAN_POINT ( 'NONE',  ( 4.687500001229034652, 6.123233995736764310E-16, -4.999999999999998224 ) ) ;
#65472 = CARTESIAN_POINT ( 'NONE',  ( 17.28750000000000142, 5.773502691896255534, 3.535250795749688894E-16 ) ) ;
#65473 =( BOUNDED_CURVE ( )  B_SPLINE_CURVE ( 2, ( #823, #69145, #6718, #18135, #5636, #17063, #39623 ),
 .UNSPECIFIED., .F., .F. ) 
 B_SPLINE_CURVE_WITH_KNOTS ( ( 3, 2, 2, 3 ),
 ( 0.5899999999999999689, 0.5933333333333333792, 0.5966666666666666785, 0.5999999999999999778 ),
 .UNSPECIFIED. ) 
 CURVE ( )  GEOMETRIC_REPRESENTATION_ITEM ( )  RATIONAL_B_SPLINE_CURVE ( ( 1.000000000000000000, 0.8660254037844387076, 1.000000000000000000, 0.8660254037844387076, 1.000000000000000000, 0.8660254037844387076, 1.000000000000000000 ) ) 
 REPRESENTATION_ITEM ( '' )  );
#65474 = CARTESIAN_POINT ( 'NONE',  ( 19.47187500061451360, 3.027376345333611329, 5.243569643749999010 ) ) ;
#65475 = CARTESIAN_POINT ( 'NONE',  ( 16.50000000122903288, 5.773502691896255534, 3.535250795749688894E-16 ) ) ;
#65476 = CARTESIAN_POINT ( 'NONE',  ( 21.41250000000000497, 2.886751345948126879, 4.999999999999999112 ) ) ;
#65477 = CARTESIAN_POINT ( 'NONE',  ( 4.243569643749999898, 15.97812500061451857, -30.00000000000000000 ) ) ;
#65478 = CARTESIAN_POINT ( 'NONE',  ( 1.999999999999997335, 20.07499999999999929, 33.46410161513775705 ) ) ;
#65479 = CARTESIAN_POINT ( 'NONE',  ( 2.733878782416514941, -4.186395442746991158, 2.733878782416514941 ) ) ;
#65480 = CARTESIAN_POINT ( 'NONE',  ( 30.00000000000000000, 0.000000000000000000, 4.999999999999998224 ) ) ;
#65481 = CARTESIAN_POINT ( 'NONE',  ( 0.000000000000000000, 20.00000000000000000, -30.00000000000000000 ) ) ;
#65482 = CARTESIAN_POINT ( 'NONE',  ( 30.00000000000000000, 0.000000000000000000, 0.000000000000000000 ) ) ;
#65483 = CARTESIAN_POINT ( 'NONE',  ( 1.999999999999998668, 14.56250000122903288, 26.53589838486224650 ) ) ;
#65484 = CARTESIAN_POINT ( 'NONE',  ( 16.50937500061451502, -4.541064518000417216, -2.621784821875001281 ) ) ;
#65485 = CARTESIAN_POINT ( 'NONE',  ( 28.98750000000000071, 5.773502691896255534, 3.535250795749688894E-16 ) ) ;
#65486 = CARTESIAN_POINT ( 'NONE',  ( 10.86562500061451431, 3.027376345333611329, 5.243569643749999010 ) ) ;
#65487 = CARTESIAN_POINT ( 'NONE',  ( 29.03437500061451360, -2.746126346562642428, -4.756430356249999214 ) ) ;
#65488 = CARTESIAN_POINT ( 'NONE',  ( 24.27187500061452141, 3.027376345333613106, -5.243569643749998122 ) ) ;
#65489 = CARTESIAN_POINT ( 'NONE',  ( 16.58437500061451431, 5.492252693125287522, 3.363034840372157021E-16 ) ) ;
#65490 = CARTESIAN_POINT ( 'NONE',  ( 6.740625000614516082, 6.054752690667223547, 3.707466751127219781E-16 ) ) ;
#65491 = CARTESIAN_POINT ( 'NONE',  ( 13.73437500061451821, -4.541064518000419881, 2.621784821874995952 ) ) ;
#65492 = ORIENTED_EDGE ( 'NONE', *, *, #52283, .T. ) ;
#65493 = CARTESIAN_POINT ( 'NONE',  ( 24.64687500061451431, -3.027376345333610441, -5.243569643749999898 ) ) ;
#65494 = CARTESIAN_POINT ( 'NONE',  ( 28.41562500061451502, 3.027376345333611329, 5.243569643749999010 ) ) ;
#65495 = CARTESIAN_POINT ( 'NONE',  ( 26.13750000000000284, -2.886751345948098013, -5.000000000000047073 ) ) ;
#65496 = AXIS2_PLACEMENT_3D ( 'NONE', #22595, #45146, #3181 ) ;
#65497 = CARTESIAN_POINT ( 'NONE',  ( 8.400000000000000355, 0.000000000000000000, 4.999999999999998224 ) ) ;
#65498 = CARTESIAN_POINT ( 'NONE',  ( 15.86250000122903181, -4.330127018922190985, -2.500000000000001332 ) ) ;
#65499 = CARTESIAN_POINT ( 'NONE',  ( -1.071796769724490339, 19.77634618820329848, 26.00000000000000000 ) ) ;
#65500 = DIRECTION ( 'NONE',  ( 0.000000000000000000, 0.000000000000000000, -1.000000000000000000 ) ) ;
#65501 = ORIENTED_EDGE ( 'NONE', *, *, #28336, .F. ) ;
#65502 = EDGE_CURVE ( 'NONE', #72010, #21883, #49042, .T. ) ;
#65503 = CARTESIAN_POINT ( 'NONE',  ( 16.35000000000000142, 4.330127018922192761, -2.499999999999997780 ) ) ;
#65504 = CARTESIAN_POINT ( 'NONE',  ( 18.07499999999999929, 6.123233995736764310E-16, -4.999999999999998224 ) ) ;
#65505 = CARTESIAN_POINT ( 'NONE',  ( 11.91562500061451857, -6.054752690667223547, -1.112240025338166033E-15 ) ) ;
#65507 = ORIENTED_EDGE ( 'NONE', *, *, #73043, .T. ) ;
#65506 = AXIS2_PLACEMENT_3D ( 'NONE', #33361, #31905, #55898 ) ;
#65508 = LINE ( 'NONE', #69601, #56075 ) ;
#65509 = CARTESIAN_POINT ( 'NONE',  ( 4.243569643749999010, 17.42187500061451999, -32.45002607614398471 ) ) ;
#65510 = CARTESIAN_POINT ( 'NONE',  ( 4.565625000614516260, 3.027376345333611329, 5.243569643749999010 ) ) ;
#65511 = CARTESIAN_POINT ( 'NONE',  ( 2.655984681222220721E-16, 13.20312499938548534, 25.66244784525396483 ) ) ;
#65512 = CARTESIAN_POINT ( 'NONE',  ( 8.962500000000002132, -5.773502691896255534, -1.060575238724906372E-15 ) ) ;
#65513 = CARTESIAN_POINT ( 'NONE',  ( 3.651773823418189124, 3.415340091791402966, 3.978752903393068863 ) ) ;
#65514 = VERTEX_POINT ( 'NONE', #67380 ) ;
#65515 = CARTESIAN_POINT ( 'NONE',  ( 4.243569643749999898, 16.39062500061451999, 32.45002607614398471 ) ) ;
#65516 = CARTESIAN_POINT ( 'NONE',  ( 26.12812500061451360, 4.541064518000418104, 2.621784821874999949 ) ) ;
#65517 = CARTESIAN_POINT ( 'NONE',  ( 8.587500000000002132, -2.886751345948125991, -5.000000000000000000 ) ) ;
#65518 = CIRCLE ( 'NONE', #623, 4.000000000000000000 ) ;
#65519 = CARTESIAN_POINT ( 'NONE',  ( 2.655984681222220721E-16, 19.05312499938548143, 25.66244784525396483 ) ) ;
#65520 = CARTESIAN_POINT ( 'NONE',  ( 22.65937500061451715, 0.000000000000000000, 5.243569643749999010 ) ) ;
#65521 = CARTESIAN_POINT ( 'NONE',  ( 19.56562500061451715, -6.054752690667223547, -1.112240025338166033E-15 ) ) ;
#65522 = CARTESIAN_POINT ( 'NONE',  ( -4.243569643749999898, 14.81562500061459353, -32.45002607614398471 ) ) ;
#65523 = CARTESIAN_POINT ( 'NONE',  ( 22.72500000122903430, 2.886751345948129099, -4.999999999999998224 ) ) ;
#65524 = CARTESIAN_POINT ( 'NONE',  ( 4.453125000614517326, 4.541064518000418104, -2.621784821874998173 ) ) ;
#65525 = CARTESIAN_POINT ( 'NONE',  ( 27.83437500061451786, 5.824947211148865298E-16, -4.756430356249998326 ) ) ;
#65526 = CARTESIAN_POINT ( 'NONE',  ( 20.87812500061451715, -4.541064518000419881, 2.621784821874995952 ) ) ;
#65527 = CARTESIAN_POINT ( 'NONE',  ( 7.846875000614518036, -2.746126346562646425, 4.756430356249996549 ) ) ;
#65528 = CARTESIAN_POINT ( 'NONE',  ( 2.655984681222220721E-16, 16.35312499938548214, 25.66244784525396483 ) ) ;
#65529 = CARTESIAN_POINT ( 'NONE',  ( 17.10937500061451999, 4.541064518000418104, -2.621784821874998173 ) ) ;
#65530 = CARTESIAN_POINT ( 'NONE',  ( 17.03437500061451715, 6.421520780324663323E-16, -5.243569643749999010 ) ) ;
#65531 = CARTESIAN_POINT ( 'NONE',  ( 25.88437500061451502, -4.541064518000419881, 2.621784821874995952 ) ) ;
#65532 = CARTESIAN_POINT ( 'NONE',  ( 2.121784821874999061, 13.85937500061451821, 26.32496088578401583 ) ) ;
#65533 = CARTESIAN_POINT ( 'NONE',  ( 4.453125000614517326, 4.541064518000418104, -2.621784821874998173 ) ) ;
#65534 = CARTESIAN_POINT ( 'NONE',  ( 27.81562500061452070, 3.027376345333613106, -5.243569643749998122 ) ) ;
#65535 = CARTESIAN_POINT ( 'NONE',  ( 3.309375000614518836, 0.000000000000000000, 5.243569643749999010 ) ) ;
#65536 = CARTESIAN_POINT ( 'NONE',  ( 4.000000000000000000, 15.23750000000000071, 27.69059892324149885 ) ) ;
#65537 = CARTESIAN_POINT ( 'NONE',  ( 4.000000000000000000, 19.28750000000000142, 32.30940107675849049 ) ) ;
#65538 = CARTESIAN_POINT ( 'NONE',  ( 8.071875000614518569, 3.027376345333613106, -5.243569643749998122 ) ) ;
#65539 = DIRECTION ( 'NONE',  ( 0.000000000000000000, 0.000000000000000000, 1.000000000000000000 ) ) ;
#65540 = CARTESIAN_POINT ( 'NONE',  ( 15.11250000122903359, 4.330127018922192761, -2.499999999999997780 ) ) ;
#65541 = CARTESIAN_POINT ( 'NONE',  ( 9.150000001229033231, -2.886751345948125991, -5.000000000000000000 ) ) ;
#65542 = CARTESIAN_POINT ( 'NONE',  ( 5.278125000614516615, 6.421520780324663323E-16, -5.243569643749999010 ) ) ;
#65543 = CARTESIAN_POINT ( 'NONE',  ( -8.484601909799255319E-16, 15.93124999877096748, 34.61880215351700940 ) ) ;
#65544 = CARTESIAN_POINT ( 'NONE',  ( 21.99375000122903145, -2.886751345948129988, 4.999999999999997335 ) ) ;
#65545 = CARTESIAN_POINT ( 'NONE',  ( 13.65937500061451715, 0.000000000000000000, 5.243569643749999010 ) ) ;
#65546 = VERTEX_POINT ( 'NONE', #22292 ) ;
#65547 = CARTESIAN_POINT ( 'NONE',  ( 21.55312500061451431, 4.541064518000418104, -2.621784821874998173 ) ) ;
#65548 = CARTESIAN_POINT ( 'NONE',  ( 8.015625000614518214, 3.027376345333613106, -5.243569643749998122 ) ) ;
#65549 = CARTESIAN_POINT ( 'NONE',  ( 24.45937500061451786, 0.000000000000000000, 5.243569643749999010 ) ) ;
#65550 = CARTESIAN_POINT ( 'NONE',  ( 7.040625000614517681, -3.027376345333610441, -5.243569643749999898 ) ) ;
#65551 = CARTESIAN_POINT ( 'NONE',  ( 45.00000000000000000, 9.426999614876460059E-14, 9.000000000000000000 ) ) ;
#65552 = CARTESIAN_POINT ( 'NONE',  ( 8.025000001229035007, 2.886751345948126879, 4.999999999999999112 ) ) ;
#65553 = CARTESIAN_POINT ( 'NONE',  ( 21.51562500061451644, 3.027376345333613106, -5.243569643749998122 ) ) ;
#65554 = CARTESIAN_POINT ( 'NONE',  ( -4.243569643749997233, 9.940625000614515372, -27.54997392385601174 ) ) ;
#65555 = CARTESIAN_POINT ( 'NONE',  ( 9.187500001229034652, 6.123233995736764310E-16, -4.999999999999998224 ) ) ;
#65556 = CARTESIAN_POINT ( 'NONE',  ( 19.71562500061451928, 3.027376345333613106, -5.243569643749998122 ) ) ;
#65557 =( GEOMETRIC_REPRESENTATION_CONTEXT ( 3 ) GLOBAL_UNCERTAINTY_ASSIGNED_CONTEXT ( ( #54310 ) ) GLOBAL_UNIT_ASSIGNED_CONTEXT ( ( #71243, #60146, #28365 ) ) REPRESENTATION_CONTEXT ( 'NONE', 'WORKASPACE' ) );
#65558 = CARTESIAN_POINT ( 'NONE',  ( 17.39062500061451644, -3.027376345333610441, -5.243569643749999898 ) ) ;
#65559 = CARTESIAN_POINT ( 'NONE',  ( 28.92187500061451644, 2.746126346562643317, 4.756430356249998326 ) ) ;
#65560 = CARTESIAN_POINT ( 'NONE',  ( 16.98750000000000426, -2.886751345948129988, 4.999999999999997335 ) ) ;
#65561 = CARTESIAN_POINT ( 'NONE',  ( 11.81250000122903465, -4.330127018922190985, -2.500000000000001332 ) ) ;
#65562 = CARTESIAN_POINT ( 'NONE',  ( 8.690625000614515372, -3.027376345333614438, 5.243569643749998122 ) ) ;
#65563 = CARTESIAN_POINT ( 'NONE',  ( 10.75312500061451715, 4.541064518000418104, -2.621784821874998173 ) ) ;
#65564 = CARTESIAN_POINT ( 'NONE',  ( 24.30000000122903359, -2.886751345948129988, 4.999999999999997335 ) ) ;
#65565 = CARTESIAN_POINT ( 'NONE',  ( 22.35937500061451644, -4.541064518000417216, -2.621784821875001281 ) ) ;
#65566 = CARTESIAN_POINT ( 'NONE',  ( 3.553828822764864448, 3.517143826812636931, -3.889051543804785016 ) ) ;
#65567 = CARTESIAN_POINT ( 'NONE',  ( 5.850000001229035185, -2.886751345948129988, 4.999999999999997335 ) ) ;
#65568 = CARTESIAN_POINT ( 'NONE',  ( 7.209375000614519635, 4.541064518000418104, -2.621784821874998173 ) ) ;
#65569 = CARTESIAN_POINT ( 'NONE',  ( 23.14687500061451786, -3.027376345333614438, 5.243569643749998122 ) ) ;
#65570 = CARTESIAN_POINT ( 'NONE',  ( -4.000000000000000000, 12.72499999999999964, 30.00000000000000000 ) ) ;
#65571 = CARTESIAN_POINT ( 'NONE',  ( 17.69062500061451715, -3.027376345333614438, 5.243569643749998122 ) ) ;
#65572 = CARTESIAN_POINT ( 'NONE',  ( 23.40937500061451715, 4.541064518000418104, -2.621784821874998173 ) ) ;
#65573 = CARTESIAN_POINT ( 'NONE',  ( 3.756430356250000102, 20.40312499938548285, 30.00000000000000000 ) ) ;
#65574 = CARTESIAN_POINT ( 'NONE',  ( 23.21250000000000213, 2.886751345948126879, 4.999999999999998224 ) ) ;
#65575 = CARTESIAN_POINT ( 'NONE',  ( 4.000000000000000000, 15.68750000000000000, 32.30940107675849760 ) ) ;
#65576 = CARTESIAN_POINT ( 'NONE',  ( 4.846875000614519813, -3.027376345333610441, -5.243569643749999898 ) ) ;
#65577 = CARTESIAN_POINT ( 'NONE',  ( 15.25312500061451715, 4.541064518000418104, -2.621784821874998173 ) ) ;
#65578 = CARTESIAN_POINT ( 'NONE',  ( 14.10937500061451644, 0.000000000000000000, 5.243569643749999010 ) ) ;
#65579 = EDGE_LOOP ( 'NONE', ( #51787, #12571, #35643, #70858 ) ) ;
#65580 = CARTESIAN_POINT ( 'NONE',  ( 30.00000000000000000, 0.000000000000000000, 0.000000000000000000 ) ) ;
#65581 = CARTESIAN_POINT ( 'NONE',  ( 23.99062500061451786, -3.027376345333614438, 5.243569643749998122 ) ) ;
#65582 = CARTESIAN_POINT ( 'NONE',  ( -0.7368805616696194605, 9.859898480082234684, -34.17910162106521454 ) ) ;
#65583 = CARTESIAN_POINT ( 'NONE',  ( -4.000000000000000888, 20.41250000000000142, 32.30940107675850470 ) ) ;
#65584 = CARTESIAN_POINT ( 'NONE',  ( 15.00000000000000000, 4.330127018922192761, -2.499999999999997780 ) ) ;
#65585 = CARTESIAN_POINT ( 'NONE',  ( 24.82500000122902861, -5.773502691896255534, -1.060575238724906372E-15 ) ) ;
#65586 = CARTESIAN_POINT ( 'NONE',  ( 19.52812500061451573, -4.541064518000419881, 2.621784821874995952 ) ) ;
#65587 = ORIENTED_EDGE ( 'NONE', *, *, #27586, .F. ) ;
#65588 = CARTESIAN_POINT ( 'NONE',  ( 21.52499999999999858, -4.330127018922194537, 2.499999999999995559 ) ) ;
#65589 = CARTESIAN_POINT ( 'NONE',  ( 22.65937500061451715, 0.000000000000000000, 5.243569643749999010 ) ) ;
#65590 = EDGE_CURVE ( 'NONE', #11954, #61742, #67398, .T. ) ;
#65591 = ORIENTED_EDGE ( 'NONE', *, *, #3605, .T. ) ;
#65592 = LINE ( 'NONE', #42699, #33665 ) ;
#65593 = CARTESIAN_POINT ( 'NONE',  ( 10.49062500061451431, -3.027376345333614438, 5.243569643749998122 ) ) ;
#65594 = CARTESIAN_POINT ( 'NONE',  ( 2.990625000614519191, -3.027376345333610441, -5.243569643749999898 ) ) ;
#65595 = CARTESIAN_POINT ( 'NONE',  ( 14.52187500061451608, -4.119189519843968306, 2.378215178124996054 ) ) ;
#65596 = CARTESIAN_POINT ( 'NONE',  ( 27.02812500061451573, 4.541064518000418104, 2.621784821874999949 ) ) ;
#65597 = VECTOR ( 'NONE', #59746, 1000.000000000000000 ) ;
#65598 = CARTESIAN_POINT ( 'NONE',  ( 16.76249999999999929, 2.886751345948129099, -4.999999999999998224 ) ) ;
#65599 = CARTESIAN_POINT ( 'NONE',  ( 26.17500000000000071, 6.123233995736764310E-16, -4.999999999999998224 ) ) ;
#65600 = CARTESIAN_POINT ( 'NONE',  ( 1.071796769724489895, 10.86740381056766758, -34.00000000000000000 ) ) ;
#65601 = CARTESIAN_POINT ( 'NONE',  ( 7.059375000614518392, -4.541064518000417216, -2.621784821875001281 ) ) ;
#65602 = CARTESIAN_POINT ( 'NONE',  ( 16.95937500061451786, -4.541064518000417216, -2.621784821875001281 ) ) ;
#65603 = DIRECTION ( 'NONE',  ( 0.000000000000000000, 0.000000000000000000, -1.000000000000000000 ) ) ;
#65604 = ORIENTED_EDGE ( 'NONE', *, *, #24878, .T. ) ;
#65605 = CARTESIAN_POINT ( 'NONE',  ( 25.56562500061452070, 3.027376345333613106, -5.243569643749998122 ) ) ;
#65606 = CARTESIAN_POINT ( 'NONE',  ( 28.65937500061451715, -4.541064518000417216, -2.621784821875001281 ) ) ;
#65607 = CARTESIAN_POINT ( 'NONE',  ( -4.000000000000000000, 14.91874999877096641, 30.00000000000000000 ) ) ;
#65608 = CARTESIAN_POINT ( 'NONE',  ( 14.58750000000000036, 5.773502691896255534, 3.535250795749688894E-16 ) ) ;
#65609 = CARTESIAN_POINT ( 'NONE',  ( 12.44062500061451537, -3.027376345333610441, -5.243569643749999898 ) ) ;
#65610 = CARTESIAN_POINT ( 'NONE',  ( -1.071796769724491005, 14.95759618943233527, -34.00000000000000000 ) ) ;
#65611 = CARTESIAN_POINT ( 'NONE',  ( 45.00000000000000000, 0.000000000000000000, 0.000000000000000000 ) ) ;
#65612 = CARTESIAN_POINT ( 'NONE',  ( 15.33750000122903323, -4.330127018922194537, 2.499999999999995559 ) ) ;
#65613 = DIRECTION ( 'NONE',  ( -0.000000000000000000, -1.000000000000000000, -0.000000000000000000 ) ) ;
#65614 = CARTESIAN_POINT ( 'NONE',  ( 16.77187500061451786, 2.746126346562643317, 4.756430356249998326 ) ) ;
#65615 = CARTESIAN_POINT ( 'NONE',  ( 5.915625000614515905, 3.027376345333611329, 5.243569643749999010 ) ) ;
#65616 = CARTESIAN_POINT ( 'NONE',  ( 22.58437500061451431, 4.541064518000418104, 2.621784821874999949 ) ) ;
#65617 = ADVANCED_FACE ( 'NONE', ( #28212 ), #61812, .F. ) ;
#65618 = CARTESIAN_POINT ( 'NONE',  ( 4.243569643749999898, 16.89687500061451786, 32.45002607614398471 ) ) ;
#65619 = CARTESIAN_POINT ( 'NONE',  ( 23.40937500061451715, 4.541064518000418104, -2.621784821874998173 ) ) ;
#65620 = CARTESIAN_POINT ( 'NONE',  ( 4.612500000000002487, 2.886751345948129099, -4.999999999999998224 ) ) ;
#65621 = CARTESIAN_POINT ( 'NONE',  ( -3.999999999999999112, 11.11250000122903536, 30.00000000000000000 ) ) ;
#65622 = CARTESIAN_POINT ( 'NONE',  ( 12.55312500061451786, 4.541064518000418104, -2.621784821874998173 ) ) ;
#65623 = CARTESIAN_POINT ( 'NONE',  ( 5.137500001229033941, 6.123233995736764310E-16, -4.999999999999998224 ) ) ;
#65624 = CARTESIAN_POINT ( 'NONE',  ( 10.35937500061451644, 4.541064518000418104, -2.621784821874998173 ) ) ;
#65625 = CARTESIAN_POINT ( 'NONE',  ( 13.12500000000000178, 6.123233995736764310E-16, -4.999999999999998224 ) ) ;
#65626 = CARTESIAN_POINT ( 'NONE',  ( 9.403125000614517504, 4.541064518000418104, -2.621784821874998173 ) ) ;
#65627 = CARTESIAN_POINT ( 'NONE',  ( 15.45937500061451608, 0.000000000000000000, 5.243569643749999010 ) ) ;
#65628 = CARTESIAN_POINT ( 'NONE',  ( -1.071796769724492115, 19.11740381056766225, 34.00000000000000000 ) ) ;
#65629 = CARTESIAN_POINT ( 'NONE',  ( 20.73750000122903359, -4.330127018922194537, 2.499999999999995559 ) ) ;
#65630 = CARTESIAN_POINT ( 'NONE',  ( 11.59687500061451892, -3.027376345333610441, -5.243569643749999898 ) ) ;
#65631 = CARTESIAN_POINT ( 'NONE',  ( 13.00312500061451537, 4.541064518000418104, -2.621784821874998173 ) ) ;
#65632 = CARTESIAN_POINT ( 'NONE',  ( 27.91875000122903216, -5.773502691896255534, -1.060575238724906372E-15 ) ) ;
#65633 = CARTESIAN_POINT ( 'NONE',  ( 21.15937500061451715, 4.541064518000418104, -2.621784821874998173 ) ) ;
#65634 = CARTESIAN_POINT ( 'NONE',  ( 1.626862140677534273E-15, 18.42500000122903359, 34.00000000000000000 ) ) ;
#65635 = CARTESIAN_POINT ( 'NONE',  ( -0.2805529113108867767, 4.994030452822312505, 26.00745495759712611 ) ) ;
#65636 = CYLINDRICAL_SURFACE ( 'NONE', #15986, 4.000000000000000000 ) ;
#65637 = CARTESIAN_POINT ( 'NONE',  ( -4.243569643749998122, 14.94687500061451679, -27.54997392385601174 ) ) ;
#65638 = CARTESIAN_POINT ( 'NONE',  ( 15.60000000122903607, 5.773502691896255534, 3.535250795749688894E-16 ) ) ;
#65639 = CARTESIAN_POINT ( 'NONE',  ( 10.84687500061451892, 6.054752690667223547, 3.707466751127219781E-16 ) ) ;
#65640 = CARTESIAN_POINT ( 'NONE',  ( 4.243569643749999898, 17.29062500061451502, -27.54997392385601529 ) ) ;
#65641 = CARTESIAN_POINT ( 'NONE',  ( 16.87500000122903288, 2.886751345948129099, -4.999999999999998224 ) ) ;
#65642 = CARTESIAN_POINT ( 'NONE',  ( 9.890625000614516438, 6.054752690667223547, 3.707466751127219781E-16 ) ) ;
#65643 = VERTEX_POINT ( 'NONE', #34096 ) ;
#65644 = CARTESIAN_POINT ( 'NONE',  ( 16.76249999999999929, 2.886751345948129099, -4.999999999999998224 ) ) ;
#65645 = CARTESIAN_POINT ( 'NONE',  ( 10.46250000122903323, -4.330127018922190985, -2.500000000000001332 ) ) ;
#65646 = CARTESIAN_POINT ( 'NONE',  ( 9.009375000614518569, 4.541064518000418104, -2.621784821874998173 ) ) ;
#65647 = CARTESIAN_POINT ( 'NONE',  ( 9.412500001229034297, 0.000000000000000000, 4.999999999999998224 ) ) ;
#65648 = CARTESIAN_POINT ( 'NONE',  ( 19.65000000122902790, 5.773502691896255534, 3.535250795749688894E-16 ) ) ;
#65649 = CARTESIAN_POINT ( 'NONE',  ( 15.89062500061451289, -3.027376345333614438, 5.243569643749998122 ) ) ;
#65650 = CARTESIAN_POINT ( 'NONE',  ( 19.52812500061451573, -4.541064518000419881, 2.621784821874995952 ) ) ;
#65651 = CARTESIAN_POINT ( 'NONE',  ( 27.26250000122903216, 4.330127018922192761, -2.499999999999997780 ) ) ;
#65652 = CARTESIAN_POINT ( 'NONE',  ( 3.028125000614518392, 6.421520780324663323E-16, -5.243569643749999010 ) ) ;
#65653 = CARTESIAN_POINT ( 'NONE',  ( 24.29999999999999716, -4.330127018922190985, -2.500000000000001332 ) ) ;
#65654 = CARTESIAN_POINT ( 'NONE',  ( 4.955394143245530181, -0.7664506687210094205, -5.056849431660869421 ) ) ;
#65655 = AXIS2_PLACEMENT_3D ( 'NONE', #53301, #15235, #37772 ) ;
#65656 = CARTESIAN_POINT ( 'NONE',  ( 27.78749999999999787, -2.886751345948129988, 4.999999999999997335 ) ) ;
#65657 = CARTESIAN_POINT ( 'NONE',  ( 27.57187500061451857, 3.027376345333611329, 5.243569643749999010 ) ) ;
#65658 = CARTESIAN_POINT ( 'NONE',  ( -1.626862140677534273E-15, 18.18124999877096215, 34.00000000000000000 ) ) ;
#65659 = CARTESIAN_POINT ( 'NONE',  ( 11.81250000122903465, -4.330127018922190985, -2.500000000000001332 ) ) ;
#65660 = CARTESIAN_POINT ( 'NONE',  ( 29.78437500061451715, 4.541064518000418104, 2.621784821874999949 ) ) ;
#65661 = CARTESIAN_POINT ( 'NONE',  ( 22.76249999999999929, 2.886751345948093572, 5.000000000000056843 ) ) ;
#65662 = CARTESIAN_POINT ( 'NONE',  ( 7.246875000614518392, 6.054752690667223547, 3.707466751127219781E-16 ) ) ;
#65663 = B_SPLINE_CURVE_WITH_KNOTS ( 'NONE', 3,
 ( #49124, #48025, #54655, #36928, #70918, #43579, #71653, #26955, #70179, #19926 ),
 .UNSPECIFIED., .F., .F.,
 ( 4, 3, 3, 4 ),
 ( 6.633699979077398476E-15, 0.0001572284277986207531, 0.0003144570899457547575, 0.0005090485883879889480 ),
 .UNSPECIFIED. ) ;
#65664 = CARTESIAN_POINT ( 'NONE',  ( 25.75312500061451715, 0.000000000000000000, 5.243569643749999010 ) ) ;
#65665 = DIRECTION ( 'NONE',  ( -0.000000000000000000, -1.000000000000000000, -0.000000000000000000 ) ) ;
#65666 = CARTESIAN_POINT ( 'NONE',  ( 1.999999999999998668, 10.51250000122903572, 26.53589838486224650 ) ) ;
#65667 = CARTESIAN_POINT ( 'NONE',  ( -1.999999999999999112, 16.69999999999999929, 26.53589838486224650 ) ) ;
#65668 = CARTESIAN_POINT ( 'NONE',  ( 5.934375000614517504, 4.541064518000418104, 2.621784821874999949 ) ) ;
#65669 = CARTESIAN_POINT ( 'NONE',  ( 7.809375000614519280, 0.000000000000000000, 5.243569643749999010 ) ) ;
#65670 = CARTESIAN_POINT ( 'NONE',  ( 4.275000000000001243, 4.330127018922191873, 2.499999999999999556 ) ) ;
#65671 =( BOUNDED_CURVE ( )  B_SPLINE_CURVE ( 2, ( #56125, #73112, #22494, #45044, #16944, #23939, #29854, #23213, #1433 ),
 .UNSPECIFIED., .F., .F. ) 
 B_SPLINE_CURVE_WITH_KNOTS ( ( 3, 2, 2, 2, 3 ),
 ( 0.9021739130434782705, 0.9057971014492753881, 0.9130434782608695121, 0.9202898550724637472, 0.9239130434782608647 ),
 .UNSPECIFIED. ) 
 CURVE ( )  GEOMETRIC_REPRESENTATION_ITEM ( )  RATIONAL_B_SPLINE_CURVE ( ( 0.9330127018922194093, 0.9330127018922194093, 1.000000000000000000, 0.8660254037844387076, 1.000000000000000000, 0.8660254037844387076, 1.000000000000000000, 0.9330127018922194093, 0.9330127018922194093 ) ) 
 REPRESENTATION_ITEM ( '' )  );
#65672 = CARTESIAN_POINT ( 'NONE',  ( -2.121784821874999949, 12.97812500061459318, 26.32496088578401938 ) ) ;
#65673 = CARTESIAN_POINT ( 'NONE',  ( 21.63749999999999929, -2.886751345948125991, -5.000000000000000000 ) ) ;
#65674 = CARTESIAN_POINT ( 'NONE',  ( 29.62500000000000000, -4.330127018922194537, 2.499999999999995559 ) ) ;
#65675 = CARTESIAN_POINT ( 'NONE',  ( 3.225000000000002309, 6.123233995736764310E-16, -4.999999999999998224 ) ) ;
#65676 = EDGE_CURVE ( 'NONE', #28753, #46571, #17814, .T. ) ;
#65677 = ORIENTED_EDGE ( 'NONE', *, *, #9622, .T. ) ;
#65678 = CARTESIAN_POINT ( 'NONE',  ( 17.72812500061451502, -4.541064518000419881, 2.621784821874995952 ) ) ;
#65679 = CARTESIAN_POINT ( 'NONE',  ( 9.553125000614517859, 0.000000000000000000, 5.243569643749999010 ) ) ;
#65680 = CARTESIAN_POINT ( 'NONE',  ( 24.87187500061451217, -4.119189519843968306, 2.378215178124996054 ) ) ;
#65681 = CARTESIAN_POINT ( 'NONE',  ( 6.234375000614519102, 6.421520780324663323E-16, -5.243569643749999010 ) ) ;
#65682 = CARTESIAN_POINT ( 'NONE',  ( 22.87500000000000000, -4.330127018922194537, 2.499999999999995559 ) ) ;
#65683 = CARTESIAN_POINT ( 'NONE',  ( 20.85000000122903430, -2.886751345948125991, -5.000000000000000000 ) ) ;
#65684 = CARTESIAN_POINT ( 'NONE',  ( 0.000000000000000000, 20.00000000000000000, -30.00000000000000000 ) ) ;
#65685 = CARTESIAN_POINT ( 'NONE',  ( 10.17187500061451999, -6.054752690667223547, -1.112240025338166033E-15 ) ) ;
#65686 = CARTESIAN_POINT ( 'NONE',  ( 13.95937500061451786, 4.541064518000418104, -2.621784821874998173 ) ) ;
#65687 = CARTESIAN_POINT ( 'NONE',  ( 23.67187500061451999, -6.054752690667223547, -1.112240025338166033E-15 ) ) ;
#65688 = VECTOR ( 'NONE', #32399, 1000.000000000000000 ) ;
#65689 = CARTESIAN_POINT ( 'NONE',  ( -6.275039685470489619E-15, 17.97500000122903074, -26.00000000000000355 ) ) ;
#65690 = CARTESIAN_POINT ( 'NONE',  ( 14.13750000000000107, 5.773502691896255534, 3.535250795749688894E-16 ) ) ;
#65691 = CARTESIAN_POINT ( 'NONE',  ( 17.63437500061451502, 4.541064518000418104, 2.621784821874999949 ) ) ;
#65692 = CARTESIAN_POINT ( 'NONE',  ( 9.459375000614517859, 4.541064518000418104, -2.621784821874998173 ) ) ;
#65693 = CARTESIAN_POINT ( 'NONE',  ( -3.756430356249999214, 20.14062499938548356, 27.83122392262697531 ) ) ;
#65694 = CARTESIAN_POINT ( 'NONE',  ( 22.68750000000000000, 5.773502691896255534, 3.535250795749688894E-16 ) ) ;
#65695 = CARTESIAN_POINT ( 'NONE',  ( -4.000000000000000000, 14.52500000000000036, 30.00000000000000000 ) ) ;
#65696 = CARTESIAN_POINT ( 'NONE',  ( -1.473772837211104525, 9.872922166578584680, -34.04916900799978663 ) ) ;
#65697 = CARTESIAN_POINT ( 'NONE',  ( 24.27187500061452141, 2.746126346562645981, -4.756430356249997438 ) ) ;
#65698 = CARTESIAN_POINT ( 'NONE',  ( 11.35312500061451679, 0.000000000000000000, 5.243569643749999010 ) ) ;
#65699 = CARTESIAN_POINT ( 'NONE',  ( 28.73437500061451644, 6.421520780324663323E-16, -5.243569643749999010 ) ) ;
#65700 = CARTESIAN_POINT ( 'NONE',  ( 30.00000000000000000, 0.000000000000000000, 4.999999999999998224 ) ) ;
#65701 = CARTESIAN_POINT ( 'NONE',  ( 4.000000000000000000, 9.950000001229033941, -27.69059892324149885 ) ) ;
#65702 = CARTESIAN_POINT ( 'NONE',  ( 12.90000000000000213, 0.000000000000000000, 4.999999999999998224 ) ) ;
#65703 = CARTESIAN_POINT ( 'NONE',  ( 8.484601909799253346E-16, 18.42500000122903714, 34.61880215351700230 ) ) ;
#65705 =( BOUNDED_CURVE ( )  B_SPLINE_CURVE ( 2, ( #28012, #1387, #16898, #44648, #1027, #34617, #662 ),
 .UNSPECIFIED., .F., .F. ) 
 B_SPLINE_CURVE_WITH_KNOTS ( ( 3, 2, 2, 3 ),
 ( 0.3400000000000000799, 0.3433333333333333792, 0.3466666666666667895, 0.3500000000000000888 ),
 .UNSPECIFIED. ) 
 CURVE ( )  GEOMETRIC_REPRESENTATION_ITEM ( )  RATIONAL_B_SPLINE_CURVE ( ( 0.9999999999999977796, 0.8660254037844409281, 1.000000000000000000, 0.8660254037844387076, 1.000000000000000000, 0.8660254037844342667, 1.000000000000004441 ) ) 
 REPRESENTATION_ITEM ( '' )  );
#65704 = CARTESIAN_POINT ( 'NONE',  ( 11.77500000122903501, -5.773502691896255534, -1.060575238724906372E-15 ) ) ;
#65706 = CARTESIAN_POINT ( 'NONE',  ( 23.03437500061451715, 4.541064518000418104, 2.621784821874999949 ) ) ;
#65707 = CARTESIAN_POINT ( 'NONE',  ( 16.92187500061451999, -6.054752690667223547, -1.112240025338166033E-15 ) ) ;
#65708 = CARTESIAN_POINT ( 'NONE',  ( -3.999999999999999112, 16.36250000000000071, -32.30940107675850470 ) ) ;
#65709 = ORIENTED_EDGE ( 'NONE', *, *, #35651, .T. ) ;
#65710 = CARTESIAN_POINT ( 'NONE',  ( 17.16562500061451502, 3.027376345333611329, 5.243569643749999010 ) ) ;
#65711 = CARTESIAN_POINT ( 'NONE',  ( 27.93750000122903288, -4.330127018922194537, 2.499999999999995559 ) ) ;
#65712 = CARTESIAN_POINT ( 'NONE',  ( 17.89687500061451431, -3.027376345333610441, -5.243569643749999898 ) ) ;
#65713 = CARTESIAN_POINT ( 'NONE',  ( 4.490625000614516971, 6.054752690667223547, 3.707466751127219781E-16 ) ) ;
#65714 = CARTESIAN_POINT ( 'NONE',  ( 19.15312500061451573, -4.541064518000417216, -2.621784821875001281 ) ) ;
#65715 = CARTESIAN_POINT ( 'NONE',  ( -3.999999999999999112, 15.38750000000000107, 27.69059892324149530 ) ) ;
#65716 = CARTESIAN_POINT ( 'NONE',  ( 29.70937500061451431, 4.541064518000418104, -2.621784821874998173 ) ) ;
#65717 = CARTESIAN_POINT ( 'NONE',  ( -2.121784821874999949, 12.97812500061451679, 26.32496088578401938 ) ) ;
#65718 = CARTESIAN_POINT ( 'NONE',  ( 17.70000000122903216, -2.886751345948125991, -5.000000000000000000 ) ) ;
#65719 = CARTESIAN_POINT ( 'NONE',  ( 8.821875000614518569, -5.492252693125287522, -1.008910452111647106E-15 ) ) ;
#65720 = CARTESIAN_POINT ( 'NONE',  ( 27.51562500061451644, 3.027376345333611329, 5.243569643749999010 ) ) ;
#65721 = CARTESIAN_POINT ( 'NONE',  ( -2.000000000000000000, 9.687500001229034652, 26.53589838486224650 ) ) ;
#65722 = CARTESIAN_POINT ( 'NONE',  ( 20.52187500061451786, -6.054752690667223547, -1.112240025338166033E-15 ) ) ;
#65723 = CARTESIAN_POINT ( 'NONE',  ( 23.06250000122903288, -4.330127018922190985, -2.500000000000001332 ) ) ;
#65724 = CARTESIAN_POINT ( 'NONE',  ( 22.45312500061451644, 4.541064518000418104, -2.621784821874998173 ) ) ;
#65725 = CARTESIAN_POINT ( 'NONE',  ( 16.05937500061451573, -4.541064518000417216, -2.621784821875001281 ) ) ;
#65726 = CARTESIAN_POINT ( 'NONE',  ( 12.77812500061451750, -4.541064518000419881, 2.621784821874995952 ) ) ;
#65727 = CARTESIAN_POINT ( 'NONE',  ( 9.001249775931846008E-16, 15.02187500061451608, 34.90005215228797653 ) ) ;
#65728 =( BOUNDED_CURVE ( )  B_SPLINE_CURVE ( 2, ( #10528, #50780, #28605, #72585, #55956, #60757, #66684, #10165, #5352 ),
 .UNSPECIFIED., .F., .F. ) 
 B_SPLINE_CURVE_WITH_KNOTS ( ( 3, 2, 2, 2, 3 ),
 ( 0.4239130434782608647, 0.4275362318840579823, 0.4347826086956521618, 0.4420289855072463969, 0.4456521739130435145 ),
 .UNSPECIFIED. ) 
 CURVE ( )  GEOMETRIC_REPRESENTATION_ITEM ( )  RATIONAL_B_SPLINE_CURVE ( ( 0.9330127018922194093, 0.9330127018922194093, 1.000000000000000000, 0.8660254037844387076, 1.000000000000000000, 0.8660254037844387076, 1.000000000000000000, 0.9330127018922188542, 0.9330127018922194093 ) ) 
 REPRESENTATION_ITEM ( '' )  );
#65729 = CARTESIAN_POINT ( 'NONE',  ( 20.99062500061451431, -3.027376345333610441, -5.243569643749999898 ) ) ;
#65730 = CARTESIAN_POINT ( 'NONE',  ( 29.27812500061451573, 4.541064518000418104, 2.621784821874999949 ) ) ;
#65731 = ORIENTED_EDGE ( 'NONE', *, *, #33365, .F. ) ;
#65732 = ORIENTED_EDGE ( 'NONE', *, *, #45894, .F. ) ;
#65733 = CARTESIAN_POINT ( 'NONE',  ( 22.94999999999999929, -4.330127018922190985, -2.500000000000001332 ) ) ;
#65734 = CARTESIAN_POINT ( 'NONE',  ( 4.243569643749999898, 19.18437500061451928, -30.00000000000000000 ) ) ;
#65735 = CARTESIAN_POINT ( 'NONE',  ( 12.44999999999999929, 0.000000000000000000, 4.999999999999998224 ) ) ;
#65736 = CARTESIAN_POINT ( 'NONE',  ( 24.40312500061451573, 0.000000000000000000, 5.243569643749999010 ) ) ;
#65737 = CARTESIAN_POINT ( 'NONE',  ( 4.228125000614517681, -4.541064518000419881, 2.621784821874995952 ) ) ;
#65738 = CARTESIAN_POINT ( 'NONE',  ( 18.07500000122903216, -5.773502691896255534, -1.060575238724906372E-15 ) ) ;
#65739 = CARTESIAN_POINT ( 'NONE',  ( 23.87812500061451715, 4.541064518000418104, 2.621784821874999949 ) ) ;
#65740 = CARTESIAN_POINT ( 'NONE',  ( 23.51249999999999574, 2.886751345948129099, -4.999999999999998224 ) ) ;
#65741 = CARTESIAN_POINT ( 'NONE',  ( 28.49062500061451431, -3.027376345333614438, 5.243569643749998122 ) ) ;
#65742 = CARTESIAN_POINT ( 'NONE',  ( 8.428125000614517859, 6.421520780324663323E-16, -5.243569643749999010 ) ) ;
#65743 = ORIENTED_EDGE ( 'NONE', *, *, #2690, .F. ) ;
#65744 = EDGE_CURVE ( 'NONE', #11954, #6463, #28925, .T. ) ;
#65745 = CARTESIAN_POINT ( 'NONE',  ( 23.69062500061451004, -3.027376345333610441, -5.243569643749999898 ) ) ;
#65746 = CARTESIAN_POINT ( 'NONE',  ( 5.878125000614517148, 4.541064518000418104, 2.621784821874999949 ) ) ;
#65747 = CARTESIAN_POINT ( 'NONE',  ( 14.37187500061451928, 2.746126346562645981, -4.756430356249997438 ) ) ;
#65748 = DIRECTION ( 'NONE',  ( -0.000000000000000000, -1.000000000000000000, -0.000000000000000000 ) ) ;
#65749 = CARTESIAN_POINT ( 'NONE',  ( 3.999999999999999112, 12.68750000122903465, -30.00000000000000000 ) ) ;
#65750 = CARTESIAN_POINT ( 'NONE',  ( -5.810221930991193690E-16, 13.58750000000000036, -34.00000000000000000 ) ) ;
#65751 = CARTESIAN_POINT ( 'NONE',  ( 11.43750000000000000, 5.773502691896255534, 3.535250795749688894E-16 ) ) ;
#65752 = CARTESIAN_POINT ( 'NONE',  ( 12.34687500061452070, -3.027376345333614438, 5.243569643749998122 ) ) ;
#65753 = CARTESIAN_POINT ( 'NONE',  ( 6.525000001229033231, 2.886751345948129099, -4.999999999999998224 ) ) ;
#65754 = CARTESIAN_POINT ( 'NONE',  ( 13.69687500061451679, -3.027376345333614438, 5.243569643749998122 ) ) ;
#65755 = CARTESIAN_POINT ( 'NONE',  ( 15.18750000000000000, -2.886751345948129988, 4.999999999999997335 ) ) ;
#65756 = CARTESIAN_POINT ( 'NONE',  ( 5.596875000614516260, -3.027376345333614438, 5.243569643749998122 ) ) ;
#65757 = CARTESIAN_POINT ( 'NONE',  ( 30.00000000000000000, 6.123233995736764310E-16, -4.999999999999998224 ) ) ;
#65758 = CARTESIAN_POINT ( 'NONE',  ( 19.76249999999999929, -5.773502691896255534, -1.060575238724906372E-15 ) ) ;
#65759 = EDGE_CURVE ( 'NONE', #29541, #58433, #31977, .T. ) ;
#65760 = CARTESIAN_POINT ( 'NONE',  ( 11.48437500061451644, -4.541064518000419881, 2.621784821874995952 ) ) ;
#65761 = CARTESIAN_POINT ( 'NONE',  ( 21.86250000122903003, 4.330127018922192761, -2.499999999999997780 ) ) ;
#65762 = CARTESIAN_POINT ( 'NONE',  ( 22.19062500061451715, -3.027376345333614438, 5.243569643749998122 ) ) ;
#65763 = CARTESIAN_POINT ( 'NONE',  ( 1.071796769724489895, 11.76740381056766616, 26.00000000000000355 ) ) ;
#65764 = CARTESIAN_POINT ( 'NONE',  ( -2.121784821874996840, 18.52812500061459389, 33.67503911421598417 ) ) ;
#65765 = CARTESIAN_POINT ( 'NONE',  ( 24.04687500061451644, -3.027376345333614438, 5.243569643749998122 ) ) ;
#65766 = FACE_OUTER_BOUND ( 'NONE', #17887, .T. ) ;
#65767 = CARTESIAN_POINT ( 'NONE',  ( 4.940625000614515372, 6.054752690667223547, 3.707466751127219781E-16 ) ) ;
#65768 = CARTESIAN_POINT ( 'NONE',  ( 19.92187500061451289, -4.119189519843968306, 2.378215178124996054 ) ) ;
#65769 = CARTESIAN_POINT ( 'NONE',  ( 17.91562500061451502, 3.027376345333613106, -5.243569643749998122 ) ) ;
#65770 = CARTESIAN_POINT ( 'NONE',  ( 15.12187500061451750, -6.054752690667223547, -1.112240025338166033E-15 ) ) ;
#65771 = CARTESIAN_POINT ( 'NONE',  ( -4.000000000000000888, 15.91249999999999964, 32.30940107675850470 ) ) ;
#65772 = CARTESIAN_POINT ( 'NONE',  ( 28.53750000122903074, 6.123233995736764310E-16, -4.999999999999998224 ) ) ;
#65773 = CARTESIAN_POINT ( 'NONE',  ( 5.634375000614519458, -4.541064518000419881, 2.621784821874995952 ) ) ;
#65774 = CARTESIAN_POINT ( 'NONE',  ( 17.18437500061451573, 4.541064518000418104, 2.621784821874999949 ) ) ;
#65775 = CYLINDRICAL_SURFACE ( 'NONE', #23119, 4.999999999999998224 ) ;
#65776 = CARTESIAN_POINT ( 'NONE',  ( 23.43750000000000000, -2.886751345948125991, -5.000000000000000000 ) ) ;
#65777 = CARTESIAN_POINT ( 'NONE',  ( 3.262500001229035718, -4.330127018922190985, -2.500000000000001332 ) ) ;
#65778 = CARTESIAN_POINT ( 'NONE',  ( 23.70937500061451786, -4.541064518000417216, -2.621784821875001281 ) ) ;
#65779 = CARTESIAN_POINT ( 'NONE',  ( 17.40937500061451715, -4.541064518000417216, -2.621784821875001281 ) ) ;
#65780 = CARTESIAN_POINT ( 'NONE',  ( 1.999999999999997335, 15.57500000000000107, 33.46410161513775705 ) ) ;
#65781 = CARTESIAN_POINT ( 'NONE',  ( 29.43750000000000000, 5.773502691896255534, 3.535250795749688894E-16 ) ) ;
#65782 = CARTESIAN_POINT ( 'NONE',  ( 7.724999999999999645, 6.123233995736764310E-16, -4.999999999999998224 ) ) ;
#65783 = CARTESIAN_POINT ( 'NONE',  ( 10.09687500061451715, -4.119189519843965641, -2.378215178125001383 ) ) ;
#65784 = CARTESIAN_POINT ( 'NONE',  ( 19.15312500061451573, -4.541064518000417216, -2.621784821875001281 ) ) ;
#65785 = CARTESIAN_POINT ( 'NONE',  ( 9.112500000000000711, 2.886751345948129099, -4.999999999999998224 ) ) ;
#65786 = EDGE_CURVE ( 'NONE', #4423, #40887, #47085, .T. ) ;
#65787 = CARTESIAN_POINT ( 'NONE',  ( 3.403125000614518836, -4.541064518000417216, -2.621784821875001281 ) ) ;
#65788 = CARTESIAN_POINT ( 'NONE',  ( 18.86249999999999716, -5.773502691896255534, -1.060575238724906372E-15 ) ) ;
#65789 = CARTESIAN_POINT ( 'NONE',  ( 17.42812500061451786, 6.421520780324663323E-16, -5.243569643749999010 ) ) ;
#65790 = CARTESIAN_POINT ( 'NONE',  ( 14.69999999999999929, 0.000000000000000000, 4.999999999999998224 ) ) ;
#65791 = CARTESIAN_POINT ( 'NONE',  ( 22.65000000122903856, -2.886751345948125991, -5.000000000000000000 ) ) ;
#65792 = LINE ( 'NONE', #16630, #4089 ) ;
#65793 = CARTESIAN_POINT ( 'NONE',  ( 29.37187500061451928, 3.027376345333611329, 5.243569643749999010 ) ) ;
#65794 = VERTEX_POINT ( 'NONE', #56987 ) ;
#65795 = CARTESIAN_POINT ( 'NONE',  ( 17.91562500061451502, 3.027376345333613106, -5.243569643749998122 ) ) ;
#65796 = CARTESIAN_POINT ( 'NONE',  ( 24.40312500061451573, 0.000000000000000000, 5.243569643749999010 ) ) ;
#65797 = CARTESIAN_POINT ( 'NONE',  ( 25.69687500061451502, 6.054752690667223547, 3.707466751127219781E-16 ) ) ;
#65798 = CARTESIAN_POINT ( 'NONE',  ( 8.662499999999999645, 2.886751345948129099, -4.999999999999998224 ) ) ;
#65799 = CARTESIAN_POINT ( 'NONE',  ( 12.92812500061451786, 6.421520780324663323E-16, -5.243569643749999010 ) ) ;
#65800 = CARTESIAN_POINT ( 'NONE',  ( 27.44062500061451715, 6.054752690667223547, 3.707466751127219781E-16 ) ) ;
#65801 = CARTESIAN_POINT ( 'NONE',  ( 16.54687500061451644, -3.027376345333610441, -5.243569643749999898 ) ) ;
#65802 = CARTESIAN_POINT ( 'NONE',  ( 10.07812500061451644, -4.541064518000419881, 2.621784821874995952 ) ) ;
#65803 = CARTESIAN_POINT ( 'NONE',  ( 6.975000001229029856, 2.886751345948062486, -5.000000000000113687 ) ) ;
#65804 = CARTESIAN_POINT ( 'NONE',  ( 4.243569643749999010, 19.16562500061451857, 27.54997392385601174 ) ) ;
#65805 = CARTESIAN_POINT ( 'NONE',  ( 23.70000000122903216, 5.773502691896255534, 3.535250795749688894E-16 ) ) ;
#65806 = CARTESIAN_POINT ( 'NONE',  ( 16.02187500061451786, -5.492252693125287522, -1.008910452111647106E-15 ) ) ;
#65807 = CARTESIAN_POINT ( 'NONE',  ( 14.31562500061451892, 3.027376345333612662, -5.243569643749998122 ) ) ;
#65808 = CARTESIAN_POINT ( 'NONE',  ( 7.434375000614519280, -4.541064518000419881, 2.621784821874995952 ) ) ;
#65809 = CARTESIAN_POINT ( 'NONE',  ( 6.459375000614518747, 0.000000000000000000, 5.243569643749999010 ) ) ;
#65810 = VERTEX_POINT ( 'NONE', #62894 ) ;
#65811 = CARTESIAN_POINT ( 'NONE',  ( 29.22187500061451715, 3.027376345333613106, -5.243569643749998122 ) ) ;
#65812 = CARTESIAN_POINT ( 'NONE',  ( 19.49062500061451431, -3.027376345333614438, 5.243569643749998122 ) ) ;
#65813 = B_SPLINE_CURVE_WITH_KNOTS ( 'NONE', 1,
 ( #5976, #39605 ),
 .UNSPECIFIED., .F., .F.,
 ( 2, 2 ),
 ( 0.000000000000000000, 1.000000000000000000 ),
 .UNSPECIFIED. ) ;
#65814 = CARTESIAN_POINT ( 'NONE',  ( 25.28437500061451715, 4.541064518000418104, 2.621784821874999949 ) ) ;
#65815 = CARTESIAN_POINT ( 'NONE',  ( 19.00312500061451715, 0.000000000000000000, 5.243569643749999010 ) ) ;
#65816 = CARTESIAN_POINT ( 'NONE',  ( -2.828200636599751609E-16, 13.13750000000000107, 25.38119784648299770 ) ) ;
#65817 = CARTESIAN_POINT ( 'NONE',  ( 26.39062500061451644, -3.027376345333610441, -5.243569643749999898 ) ) ;
#65818 = CARTESIAN_POINT ( 'NONE',  ( 7.350000001229033408, -2.886751345948125991, -5.000000000000000000 ) ) ;
#65819 = ORIENTED_EDGE ( 'NONE', *, *, #14679, .T. ) ;
#65820 = CARTESIAN_POINT ( 'NONE',  ( 2.887500001229035274, 6.123233995736764310E-16, -4.999999999999998224 ) ) ;
#65821 = CARTESIAN_POINT ( 'NONE',  ( 3.999999999999998668, 14.41250000000000142, -32.30940107675850470 ) ) ;
#65822 = CARTESIAN_POINT ( 'NONE',  ( 22.68750000122903288, 6.123233995736764310E-16, -4.999999999999998224 ) ) ;
#65823 = CARTESIAN_POINT ( 'NONE',  ( -3.756430356250001434, 13.91562499938548392, 32.16877607737301048 ) ) ;
#65824 = CARTESIAN_POINT ( 'NONE',  ( 6.196875000614515905, -3.027376345333610441, -5.243569643749999898 ) ) ;
#65825 = CARTESIAN_POINT ( 'NONE',  ( 20.41875000122903572, 2.886751345948157077, -4.999999999999949374 ) ) ;
#65826 = CARTESIAN_POINT ( 'NONE',  ( 12.14062500061451821, 6.054752690667223547, 3.707466751127219781E-16 ) ) ;
#65827 = CARTESIAN_POINT ( 'NONE',  ( 7.696875000614516793, 6.054752690667223547, 3.707466751127219781E-16 ) ) ;
#65828 = CARTESIAN_POINT ( 'NONE',  ( 26.28750000122903430, 6.123233995736764310E-16, -4.999999999999998224 ) ) ;
#65829 = CARTESIAN_POINT ( 'NONE',  ( 16.99687500061451573, -3.027376345333610441, -5.243569643749999898 ) ) ;
#65830 = CARTESIAN_POINT ( 'NONE',  ( 4.059375000614519280, 4.541064518000418104, -2.621784821874998173 ) ) ;
#65831 = CARTESIAN_POINT ( 'NONE',  ( 1.626862140677534273E-15, 11.11250000000000071, 34.00000000000000000 ) ) ;
#65832 = CARTESIAN_POINT ( 'NONE',  ( 6.440625000614517148, -3.027376345333614438, 5.243569643749998122 ) ) ;
#65833 = CARTESIAN_POINT ( 'NONE',  ( 14.69062500061451537, -3.027376345333610441, -5.243569643749999898 ) ) ;
#65834 = ORIENTED_EDGE ( 'NONE', *, *, #66238, .F. ) ;
#65835 = CARTESIAN_POINT ( 'NONE',  ( 11.99062500061451608, -3.027376345333610441, -5.243569643749999898 ) ) ;
#65836 = CARTESIAN_POINT ( 'NONE',  ( 5.475000001229035185, -5.773502691896255534, -1.060575238724906372E-15 ) ) ;
#65837 = CARTESIAN_POINT ( 'NONE',  ( 8.503125000614515372, 4.541064518000418104, -2.621784821874998173 ) ) ;
#65838 = CARTESIAN_POINT ( 'NONE',  ( 21.38437500061451502, -4.119189519843968306, 2.378215178124996054 ) ) ;
#65839 = CARTESIAN_POINT ( 'NONE',  ( 9.375000000000001776, -4.330127018922194537, 2.499999999999995559 ) ) ;
#65840 = CARTESIAN_POINT ( 'NONE',  ( 3.450000001229036162, 5.773502691896255534, 3.535250795749688894E-16 ) ) ;
#65841 = CARTESIAN_POINT ( 'NONE',  ( 17.92500000000000071, -4.330127018922194537, 2.499999999999995559 ) ) ;
#65842 = EDGE_CURVE ( 'NONE', #35743, #34653, #45199, .T. ) ;
#65843 = CARTESIAN_POINT ( 'NONE',  ( 19.17187500061451999, -6.054752690667223547, -1.112240025338166033E-15 ) ) ;
#65844 = CARTESIAN_POINT ( 'NONE',  ( 14.43750000122903288, -4.330127018922194537, 2.499999999999995559 ) ) ;
#65845 = CARTESIAN_POINT ( 'NONE',  ( 22.08749999999999858, -2.886751345948125991, -5.000000000000000000 ) ) ;
#65846 = CARTESIAN_POINT ( 'NONE',  ( 9.001249775931846008E-16, 15.86562500061451608, -25.09994784771203058 ) ) ;
#65847 = CARTESIAN_POINT ( 'NONE',  ( -3.999999999999999112, 16.06250000122903288, 30.00000000000000000 ) ) ;
#65848 = DIRECTION ( 'NONE',  ( -0.000000000000000000, -1.000000000000000000, -0.000000000000000000 ) ) ;
#65849 = CARTESIAN_POINT ( 'NONE',  ( 20.54999999999999716, 0.000000000000000000, 4.999999999999998224 ) ) ;
#65850 = DIRECTION ( 'NONE',  ( -0.000000000000000000, -1.000000000000000000, -0.000000000000000000 ) ) ;
#65851 = PRESENTATION_STYLE_ASSIGNMENT (( #21873 ) ) ;
#65852 = CYLINDRICAL_SURFACE ( 'NONE', #65655, 4.999999999999998224 ) ;
#65853 = CARTESIAN_POINT ( 'NONE',  ( 15.04687500061451644, -3.027376345333614438, 5.243569643749998122 ) ) ;
#65854 =( BOUNDED_CURVE ( )  B_SPLINE_CURVE ( 2, ( #65295, #37957, #265, #38702, #10978, #44618, #17591, #51228, #16508 ),
 .UNSPECIFIED., .F., .F. ) 
 B_SPLINE_CURVE_WITH_KNOTS ( ( 3, 2, 2, 2, 3 ),
 ( 0.1250000000000000000, 0.1296296296296296224, 0.1388888888888888951, 0.1481481481481481399, 0.1527777777777777901 ),
 .UNSPECIFIED. ) 
 CURVE ( )  GEOMETRIC_REPRESENTATION_ITEM ( )  RATIONAL_B_SPLINE_CURVE ( ( 0.9330127018922192983, 0.9330127018922194093, 1.000000000000000000, 0.8660254037844387076, 1.000000000000000000, 0.8660254037844387076, 1.000000000000000000, 0.9330127018922191873, 0.9330127018922194093 ) ) 
 REPRESENTATION_ITEM ( '' )  );
#65855 = CARTESIAN_POINT ( 'NONE',  ( 27.37500000000000000, -4.330127018922194537, 2.499999999999995559 ) ) ;
#65856 = CARTESIAN_POINT ( 'NONE',  ( 11.39062500061451644, -3.027376345333614438, 5.243569643749998122 ) ) ;
#65857 = CARTESIAN_POINT ( 'NONE',  ( 29.55937500061451217, 2.746126346562645981, -4.756430356249997438 ) ) ;
#65858 = CARTESIAN_POINT ( 'NONE',  ( 21.04687500061451644, -3.027376345333610441, -5.243569643749999898 ) ) ;
#65859 = CARTESIAN_POINT ( 'NONE',  ( 13.92187500061451644, 4.119189519843966529, 2.378215178124999607 ) ) ;
#65860 = CARTESIAN_POINT ( 'NONE',  ( 6.590625000614518392, -3.027376345333610441, -5.243569643749999898 ) ) ;
#65861 = CARTESIAN_POINT ( 'NONE',  ( 11.97187500061451892, -6.054752690667223547, -1.112240025338166033E-15 ) ) ;
#65862 = ORIENTED_EDGE ( 'NONE', *, *, #60328, .T. ) ;
#65863 = CARTESIAN_POINT ( 'NONE',  ( 24.00937500061451502, 0.000000000000000000, 5.243569643749999010 ) ) ;
#65864 = CARTESIAN_POINT ( 'NONE',  ( 3.942105046096217702, 3.076001935233272810, -30.69131329531799679 ) ) ;
#65865 = CARTESIAN_POINT ( 'NONE',  ( 26.95312500061451644, 4.541064518000418104, -2.621784821874998173 ) ) ;
#65866 = DIRECTION ( 'NONE',  ( 1.000000000000000000, 0.000000000000000000, -0.000000000000000000 ) ) ;
#65868 = EDGE_CURVE ( 'NONE', #32715, #51293, #56571, .T. ) ;
#65867 = CARTESIAN_POINT ( 'NONE',  ( 7.837499999999999467, 5.773502691896255534, 3.535250795749688894E-16 ) ) ;
#65869 = CARTESIAN_POINT ( 'NONE',  ( 17.88750000122903216, 4.330127018922191873, 2.499999999999999556 ) ) ;
#65870 = CARTESIAN_POINT ( 'NONE',  ( 0.000000000000000000, 20.00000000000000000, 26.00000000000000000 ) ) ;
#65871 = CARTESIAN_POINT ( 'NONE',  ( 8.221875000614515372, -4.119189519843968306, 2.378215178124996054 ) ) ;
#65872 = ORIENTED_EDGE ( 'NONE', *, *, #61587, .F. ) ;
#65873 = CARTESIAN_POINT ( 'NONE',  ( 15.71250000000000213, -5.773502691896255534, -1.060575238724906372E-15 ) ) ;
#65874 = CARTESIAN_POINT ( 'NONE',  ( 17.81250000000000355, 2.886751345948126879, 4.999999999999999112 ) ) ;
#65875 = CARTESIAN_POINT ( 'NONE',  ( 11.50312500061451892, -4.541064518000417216, -2.621784821875001281 ) ) ;
#65876 = EDGE_LOOP ( 'NONE', ( #68914, #18133, #53080, #14901 ) ) ;
#65877 = CARTESIAN_POINT ( 'NONE',  ( 45.00000000000000000, 0.000000000000000000, 0.000000000000000000 ) ) ;
#65878 = CARTESIAN_POINT ( 'NONE',  ( -2.121784821874999949, 17.08437500061451786, -33.67503911421598417 ) ) ;
#65879 = CARTESIAN_POINT ( 'NONE',  ( 2.915625000614516793, -6.054752690667223547, -1.112240025338166033E-15 ) ) ;
#65880 = CARTESIAN_POINT ( 'NONE',  ( 2.000000000000001332, 12.05000000000000249, 33.46410161513774995 ) ) ;
#65881 = CARTESIAN_POINT ( 'NONE',  ( 10.38750000000000107, -2.886751345948125991, -5.000000000000000000 ) ) ;
#65882 = CARTESIAN_POINT ( 'NONE',  ( 3.193447721043152665, 3.847322660365763536, 3.562742055761627835 ) ) ;
#65883 = ORIENTED_EDGE ( 'NONE', *, *, #52783, .T. ) ;
#65884 = CARTESIAN_POINT ( 'NONE',  ( 2.121784821874999061, 12.90312500061451750, 26.32496088578401583 ) ) ;
#65885 = CARTESIAN_POINT ( 'NONE',  ( 27.06562500061451004, 3.027376345333611329, 5.243569643749999010 ) ) ;
#65886 = CARTESIAN_POINT ( 'NONE',  ( 3.563259964303803873, 3.507650584494903079, 3.697742481698767847 ) ) ;
#65887 = CARTESIAN_POINT ( 'NONE',  ( -3.756430356249999214, 18.67812499938548143, 27.83122392262697531 ) ) ;
#65888 = CARTESIAN_POINT ( 'NONE',  ( 21.75937500061451502, 0.000000000000000000, 5.243569643749999010 ) ) ;
#65889 = CARTESIAN_POINT ( 'NONE',  ( 19.49062500061451431, -3.027376345333614438, 5.243569643749998122 ) ) ;
#65890 = EDGE_CURVE ( 'NONE', #17152, #4778, #69305, .T. ) ;
#65891 = CARTESIAN_POINT ( 'NONE',  ( 9.001249775931846008E-16, 14.51562500061459460, -25.09994784771203058 ) ) ;
#65892 = CARTESIAN_POINT ( 'NONE',  ( 22.23750000122903003, 6.123233995736764310E-16, -4.999999999999998224 ) ) ;
#65893 = CARTESIAN_POINT ( 'NONE',  ( 4.715625000614516615, -6.054752690667223547, -1.112240025338166033E-15 ) ) ;
#65894 = CARTESIAN_POINT ( 'NONE',  ( 23.48437500061451644, 4.119189519843966529, 2.378215178124999607 ) ) ;
#65895 = CARTESIAN_POINT ( 'NONE',  ( 22.26562500061451644, -6.054752690667223547, -1.112240025338166033E-15 ) ) ;
#65896 = CARTESIAN_POINT ( 'NONE',  ( 7.996875000614519280, -2.746126346562642428, -4.756430356249999214 ) ) ;
#65897 = CARTESIAN_POINT ( 'NONE',  ( 1.878215178125000495, 15.41562499938548392, 26.74683588394047007 ) ) ;
#65898 = CARTESIAN_POINT ( 'NONE',  ( 15.34687500061451537, 6.054752690667223547, 3.707466751127219781E-16 ) ) ;
#65899 = CARTESIAN_POINT ( 'NONE',  ( 13.35937500061451821, -4.541064518000417216, -2.621784821875001281 ) ) ;
#65900 = CARTESIAN_POINT ( 'NONE',  ( 21.23437500061451644, 4.541064518000418104, 2.621784821874999949 ) ) ;
#65901 = CARTESIAN_POINT ( 'NONE',  ( 2.121784821874999061, 12.50937500061451857, 26.32496088578401583 ) ) ;
#65902 = CARTESIAN_POINT ( 'NONE',  ( 4.153125000614515727, 0.000000000000000000, 5.243569643749999010 ) ) ;
#65903 = CARTESIAN_POINT ( 'NONE',  ( 28.30312500061451431, 4.541064518000418104, -2.621784821874998173 ) ) ;
#65904 = CARTESIAN_POINT ( 'NONE',  ( 27.29062500061451502, -3.027376345333610441, -5.243569643749999898 ) ) ;
#65905 = CARTESIAN_POINT ( 'NONE',  ( 23.53125000122902932, 6.123233995736764310E-16, -4.999999999999998224 ) ) ;
#65906 = CARTESIAN_POINT ( 'NONE',  ( 8.175000000000002487, 6.123233995736764310E-16, -4.999999999999998224 ) ) ;
#65907 = CARTESIAN_POINT ( 'NONE',  ( 6.234375000614519102, 6.421520780324663323E-16, -5.243569643749999010 ) ) ;
#65908 = CARTESIAN_POINT ( 'NONE',  ( 0.000000000000000000, 0.000000000000000000, -60.00000000000000000 ) ) ;
#65909 = CARTESIAN_POINT ( 'NONE',  ( 13.46250000122903323, 0.000000000000000000, 4.999999999999998224 ) ) ;
#65910 = CARTESIAN_POINT ( 'NONE',  ( 8.925000001229033586, 2.886751345948126879, 4.999999999999999112 ) ) ;
#65911 = CARTESIAN_POINT ( 'NONE',  ( 5.503125000614516260, 0.000000000000000000, 5.243569643749999010 ) ) ;
#65912 = CARTESIAN_POINT ( 'NONE',  ( 1.999999999999997335, 15.51874999877096784, 33.46410161513775705 ) ) ;
#65913 = CARTESIAN_POINT ( 'NONE',  ( 17.98125000122903572, -4.330127018922194537, 2.499999999999995559 ) ) ;
#65914 = CARTESIAN_POINT ( 'NONE',  ( 13.95937500061451786, 4.541064518000418104, -2.621784821874998173 ) ) ;
#65915 = VERTEX_POINT ( 'NONE', #24094 ) ;
#65916 = CARTESIAN_POINT ( 'NONE',  ( 19.75312500061451360, 4.541064518000418104, -2.621784821874998173 ) ) ;
#65917 = CARTESIAN_POINT ( 'NONE',  ( 6.778125000614518392, 4.541064518000418104, 2.621784821874999949 ) ) ;
#65918 = CARTESIAN_POINT ( 'NONE',  ( 24.38437500061451502, 4.541064518000418104, 2.621784821874999949 ) ) ;
#65919 = EDGE_CURVE ( 'NONE', #52475, #59726, #11702, .T. ) ;
#65920 = CARTESIAN_POINT ( 'NONE',  ( 8.765625000614518214, -6.054752690667223547, -1.112240025338166033E-15 ) ) ;
#65921 = CARTESIAN_POINT ( 'NONE',  ( -1.071796769724496334, 16.17634618820330061, 26.00000000000000355 ) ) ;
#65922 = CARTESIAN_POINT ( 'NONE',  ( 8.362500001229031810, 4.330127018922192761, -2.499999999999997780 ) ) ;
#65923 =( BOUNDED_CURVE ( )  B_SPLINE_CURVE ( 2, ( #43086, #71898, #8732, #26462, #31266, #20167, #71532 ),
 .UNSPECIFIED., .F., .F. ) 
 B_SPLINE_CURVE_WITH_KNOTS ( ( 3, 2, 2, 3 ),
 ( 0.5333333333333334370, 0.5361111111111112049, 0.5388888888888888618, 0.5416666666666666297 ),
 .UNSPECIFIED. ) 
 CURVE ( )  GEOMETRIC_REPRESENTATION_ITEM ( )  RATIONAL_B_SPLINE_CURVE ( ( 0.9999999999999946709, 0.8660254037844440367, 1.000000000000000000, 0.8660254037844387076, 1.000000000000000000, 0.8660254037844387076, 1.000000000000000000 ) ) 
 REPRESENTATION_ITEM ( '' )  );
#65924 = CARTESIAN_POINT ( 'NONE',  ( 22.49062500061451431, 6.054752690667223547, 3.707466751127219781E-16 ) ) ;
#65925 = CARTESIAN_POINT ( 'NONE',  ( -2.000000000000000000, 17.33750000122903145, -33.46410161513775705 ) ) ;
#65926 = CARTESIAN_POINT ( 'NONE',  ( 10.27500000122903323, 2.886751345948126879, 4.999999999999999112 ) ) ;
#65927 = CARTESIAN_POINT ( 'NONE',  ( 20.09062500061451573, -3.027376345333610441, -5.243569643749999898 ) ) ;
#65928 = CARTESIAN_POINT ( 'NONE',  ( 16.49062500061451786, -3.027376345333610441, -5.243569643749999898 ) ) ;
#65929 = CARTESIAN_POINT ( 'NONE',  ( 27.83437500061451786, 5.824947211148865298E-16, -4.756430356249998326 ) ) ;
#65930 = CARTESIAN_POINT ( 'NONE',  ( 14.69999999999999929, 0.000000000000000000, 4.999999999999998224 ) ) ;
#65931 = CARTESIAN_POINT ( 'NONE',  ( 12.07500000122903216, 2.886751345948126879, 4.999999999999999112 ) ) ;
#65932 = EDGE_CURVE ( 'NONE', #31631, #25241, #52183, .T. ) ;
#65933 = CARTESIAN_POINT ( 'NONE',  ( 7.753125000614518036, 0.000000000000000000, 5.243569643749999010 ) ) ;
#65934 = CARTESIAN_POINT ( 'NONE',  ( 11.09062500061451573, -3.027376345333610441, -5.243569643749999898 ) ) ;
#65935 = CARTESIAN_POINT ( 'NONE',  ( 23.92500000122903359, -5.773502691896255534, -1.060575238724906372E-15 ) ) ;
#65936 = CARTESIAN_POINT ( 'NONE',  ( 20.55937500061451573, -4.541064518000417216, -2.621784821875001281 ) ) ;
#65937 = CARTESIAN_POINT ( 'NONE',  ( 4.678125000614516971, -4.541064518000419881, 2.621784821874995952 ) ) ;
#65938 = CARTESIAN_POINT ( 'NONE',  ( 4.687500001229034652, 6.123233995736764310E-16, -4.999999999999998224 ) ) ;
#65939 = CARTESIAN_POINT ( 'NONE',  ( 4.921875000614518214, 3.027376345333613106, -5.243569643749998122 ) ) ;
#65940 = CARTESIAN_POINT ( 'NONE',  ( 23.63437500061451502, -4.541064518000419881, 2.621784821874995952 ) ) ;
#65941 = CARTESIAN_POINT ( 'NONE',  ( 10.42500000000000071, 6.123233995736764310E-16, -4.999999999999998224 ) ) ;
#65942 = CARTESIAN_POINT ( 'NONE',  ( 18.89062500061451644, 6.054752690667223547, 3.707466751127219781E-16 ) ) ;
#65943 = CARTESIAN_POINT ( 'NONE',  ( 23.67187500061451999, -6.054752690667223547, -1.112240025338166033E-15 ) ) ;
#65944 = CARTESIAN_POINT ( 'NONE',  ( -3.756430356250000990, 18.86562499938548498, 32.16877607737301048 ) ) ;
#65945 = CARTESIAN_POINT ( 'NONE',  ( -4.000000000000000000, 14.52500000000000036, 30.00000000000000000 ) ) ;
#65946 = CARTESIAN_POINT ( 'NONE',  ( 27.75937500061451502, -4.541064518000417216, -2.621784821875001281 ) ) ;
#65947 = CARTESIAN_POINT ( 'NONE',  ( 5.559375000614517504, 0.000000000000000000, 5.243569643749999010 ) ) ;
#65948 = CARTESIAN_POINT ( 'NONE',  ( 14.05312500061451431, 0.000000000000000000, 5.243569643749999010 ) ) ;
#65949 = CARTESIAN_POINT ( 'NONE',  ( 14.22187500061451537, -6.054752690667223547, -1.112240025338166033E-15 ) ) ;
#65950 = ORIENTED_EDGE ( 'NONE', *, *, #1615, .F. ) ;
#65951 = DIRECTION ( 'NONE',  ( 0.000000000000000000, 0.000000000000000000, 1.000000000000000000 ) ) ;
#65952 = CARTESIAN_POINT ( 'NONE',  ( 25.71562500061451573, 3.027376345333611329, 5.243569643749999010 ) ) ;
#65953 = CARTESIAN_POINT ( 'NONE',  ( 1.071796769724505438, 13.11740381056766580, -33.99999999999999289 ) ) ;
#65954 = LINE ( 'NONE', #27170, #8874 ) ;
#65955 = CARTESIAN_POINT ( 'NONE',  ( 15.75000000000000000, -4.330127018922190985, -2.500000000000001332 ) ) ;
#65956 = CARTESIAN_POINT ( 'NONE',  ( 24.75000000122902932, -2.886751345948129988, 4.999999999999997335 ) ) ;
#65957 = CARTESIAN_POINT ( 'NONE',  ( 18.06562500061451715, 3.027376345333611329, 5.243569643749999010 ) ) ;
#65958 = EDGE_LOOP ( 'NONE', ( #20415, #17615, #15296, #35182 ) ) ;
#65959 = CARTESIAN_POINT ( 'NONE',  ( 22.94999999999999929, -4.330127018922190985, -2.500000000000001332 ) ) ;
#65960 = CARTESIAN_POINT ( 'NONE',  ( 24.27187500061452141, 3.027376345333613106, -5.243569643749998122 ) ) ;
#65961 = ORIENTED_EDGE ( 'NONE', *, *, #27532, .F. ) ;
#65962 = CARTESIAN_POINT ( 'NONE',  ( 1.626862140677534273E-15, 17.86250000000000071, -26.00000000000000355 ) ) ;
#65963 = CARTESIAN_POINT ( 'NONE',  ( 10.86562500061451431, 3.027376345333611329, 5.243569643749999010 ) ) ;
#65964 = CARTESIAN_POINT ( 'NONE',  ( 3.028125000614518392, 6.421520780324663323E-16, -5.243569643749999010 ) ) ;
#65965 = CARTESIAN_POINT ( 'NONE',  ( 14.89687500061451608, 0.000000000000000000, 4.756430356249998326 ) ) ;
#65966 = CARTESIAN_POINT ( 'NONE',  ( 26.12812500061451360, 4.541064518000418104, 2.621784821874999949 ) ) ;
#65967 = CARTESIAN_POINT ( 'NONE',  ( 16.57499999999999929, -4.330127018922194537, 2.499999999999995559 ) ) ;
#65968 = CARTESIAN_POINT ( 'NONE',  ( 24.29999999999999716, -4.330127018922190985, -2.500000000000001332 ) ) ;
#65969 = CARTESIAN_POINT ( 'NONE',  ( -3.000416591977282496E-16, 19.24062500061451431, 25.09994784771203058 ) ) ;
#65970 = CARTESIAN_POINT ( 'NONE',  ( 6.534375000614517148, -4.541064518000419881, 2.621784821874995952 ) ) ;
#65971 = CARTESIAN_POINT ( 'NONE',  ( 16.58437500061451786, 6.421520780324663323E-16, -5.243569643749999010 ) ) ;
#65972 = CARTESIAN_POINT ( 'NONE',  ( 28.62187500061451573, -6.054752690667223547, -1.112240025338166033E-15 ) ) ;
#65973 = ORIENTED_EDGE ( 'NONE', *, *, #19460, .T. ) ;
#65974 = CARTESIAN_POINT ( 'NONE',  ( 26.50312500061451360, 4.541064518000418104, -2.621784821874998173 ) ) ;
#65975 = CARTESIAN_POINT ( 'NONE',  ( 26.70937500061451431, 0.000000000000000000, 5.243569643749999010 ) ) ;
#65976 = LINE ( 'NONE', #66717, #12078 ) ;
#65977 = CARTESIAN_POINT ( 'NONE',  ( 13.61250000000000071, 2.886751345948129099, -4.999999999999998224 ) ) ;
#65978 = CARTESIAN_POINT ( 'NONE',  ( 10.22812500061451679, 6.421520780324663323E-16, -5.243569643749999010 ) ) ;
#65979 = CARTESIAN_POINT ( 'NONE',  ( 9.506250001229030744, -4.330127018922190985, -2.500000000000001332 ) ) ;
#65980 = CARTESIAN_POINT ( 'NONE',  ( 5.250000000000000888, 0.000000000000000000, 4.999999999999998224 ) ) ;
#65981 = CARTESIAN_POINT ( 'NONE',  ( 28.94062500061452070, -3.027376345333614438, 5.243569643749998122 ) ) ;
#65982 = CARTESIAN_POINT ( 'NONE',  ( 17.06250000122903288, 0.000000000000000000, 4.999999999999998224 ) ) ;
#65983 = CARTESIAN_POINT ( 'NONE',  ( 27.09375000122903288, -2.886751345948091796, -5.000000000000060396 ) ) ;
#65984 = CARTESIAN_POINT ( 'NONE',  ( 14.55937500061451573, 0.000000000000000000, 4.756430356249998326 ) ) ;
#65985 = CARTESIAN_POINT ( 'NONE',  ( 6.365625000614518747, 3.027376345333611329, 5.243569643749999010 ) ) ;
#65986 = CARTESIAN_POINT ( 'NONE',  ( 22.88437500061451857, 6.421520780324663323E-16, -5.243569643749999010 ) ) ;
#65987 = CARTESIAN_POINT ( 'NONE',  ( -2.121784821874996840, 16.33437500061451786, 33.67503911421598417 ) ) ;
#65988 = CARTESIAN_POINT ( 'NONE',  ( 20.67187500061451289, 3.027376345333613106, -5.243569643749998122 ) ) ;
#65989 = CARTESIAN_POINT ( 'NONE',  ( 4.912499999999999645, -5.773502691896255534, -1.060575238724906372E-15 ) ) ;
#65990 = CARTESIAN_POINT ( 'NONE',  ( 2.000000000000001332, 9.912500001229034297, 33.46410161513774995 ) ) ;
#65991 = CARTESIAN_POINT ( 'NONE',  ( 11.99062500061451608, -3.027376345333610441, -5.243569643749999898 ) ) ;
#65992 = CARTESIAN_POINT ( 'NONE',  ( 4.162500001229033408, -4.330127018922190985, -2.500000000000001332 ) ) ;
#65993 = CARTESIAN_POINT ( 'NONE',  ( 8.746875000614515727, -3.027376345333614438, 5.243569643749998122 ) ) ;
#65994 = CARTESIAN_POINT ( 'NONE',  ( 3.928581913072007215, 3.092934553507882711, -4.135345885259243737 ) ) ;
#65995 = CARTESIAN_POINT ( 'NONE',  ( 11.01562500061451821, -6.054752690667223547, -1.112240025338166033E-15 ) ) ;
#65996 = CARTESIAN_POINT ( 'NONE',  ( 14.70937500061451786, -4.541064518000417216, -2.621784821875001281 ) ) ;
#65997 = CARTESIAN_POINT ( 'NONE',  ( 24.61875000122903145, 2.886751345948126879, 4.999999999999998224 ) ) ;
#65998 = CARTESIAN_POINT ( 'NONE',  ( 20.58750000122903145, 4.330127018922191873, 2.499999999999999556 ) ) ;
#65999 = CARTESIAN_POINT ( 'NONE',  ( 9.646875000614516082, -3.027376345333614438, 5.243569643749998122 ) ) ;
#66000 = CARTESIAN_POINT ( 'NONE',  ( 12.32812500061451821, -4.541064518000419881, 2.621784821874995952 ) ) ;
#66001 = CARTESIAN_POINT ( 'NONE',  ( 25.70625000122903003, -4.330127018922190985, -2.500000000000001332 ) ) ;
#66002 = EDGE_CURVE ( 'NONE', #10458, #403, #69832, .T. ) ;
#66003 = CARTESIAN_POINT ( 'NONE',  ( 21.68437500061451573, 4.541064518000418104, 2.621784821874999949 ) ) ;
#66004 = CARTESIAN_POINT ( 'NONE',  ( 14.10000000000000142, 4.330127018922192761, -2.499999999999997780 ) ) ;
#66005 = CARTESIAN_POINT ( 'NONE',  ( -0.6909613911670718922, 4.953869264242466208, 26.05777829539367119 ) ) ;
#66006 = CARTESIAN_POINT ( 'NONE',  ( 2.953125000614516438, -4.541064518000417216, -2.621784821875001281 ) ) ;
#66007 = CARTESIAN_POINT ( 'NONE',  ( 2.121784821874999061, 12.50937500061451857, -33.67503911421598417 ) ) ;
#66008 = CARTESIAN_POINT ( 'NONE',  ( 14.88750000122903394, -4.330127018922194537, 2.499999999999995559 ) ) ;
#66009 = CARTESIAN_POINT ( 'NONE',  ( -2.121784821874996840, 16.72812500061451857, -26.32496088578401583 ) ) ;
#66010 = CARTESIAN_POINT ( 'NONE',  ( 16.57500000122903216, 2.886751345948126879, 4.999999999999999112 ) ) ;
#66011 = CARTESIAN_POINT ( 'NONE',  ( 9.065625000614517148, 3.027376345333611329, 5.243569643749999010 ) ) ;
#66012 = ORIENTED_EDGE ( 'NONE', *, *, #42665, .T. ) ;
#66013 = CARTESIAN_POINT ( 'NONE',  ( 14.62500000000000000, 4.330127018922191873, 2.499999999999999556 ) ) ;
#66014 = CARTESIAN_POINT ( 'NONE',  ( 4.957199372764754308, -3.163855285557799935, 4.520041897618551019 ) ) ;
#66015 = CARTESIAN_POINT ( 'NONE',  ( 23.24062500061451786, -3.027376345333610441, -5.243569643749999898 ) ) ;
#66016 = CARTESIAN_POINT ( 'NONE',  ( 11.22187500061451892, 3.027376345333612662, -5.243569643749998122 ) ) ;
#66017 = CARTESIAN_POINT ( 'NONE',  ( 4.359768065504647794, -2.448001861170849836, -4.637088767021002589 ) ) ;
#66018 = CARTESIAN_POINT ( 'NONE',  ( 9.975000001229034297, -5.773502691896255534, -1.060575238724906372E-15 ) ) ;
#66019 = EDGE_CURVE ( 'NONE', #47866, #30305, #49471, .T. ) ;
#66020 = CARTESIAN_POINT ( 'NONE',  ( 19.27500000122903145, 2.886751345948126879, 4.999999999999999112 ) ) ;
#66021 = CARTESIAN_POINT ( 'NONE',  ( 16.41562500061451857, -6.054752690667223547, -1.112240025338166033E-15 ) ) ;
#66022 = CARTESIAN_POINT ( 'NONE',  ( 18.74062500061451431, -3.027376345333610441, -5.243569643749999898 ) ) ;
#66023 = CARTESIAN_POINT ( 'NONE',  ( 25.68750000122903288, -4.330127018922194537, 2.499999999999995559 ) ) ;
#66024 = EDGE_CURVE ( 'NONE', #55912, #52358, #54642, .T. ) ;
#66025 = CARTESIAN_POINT ( 'NONE',  ( 2.878125000614517592, -4.541064518000419881, 2.621784821874995952 ) ) ;
#66026 = CARTESIAN_POINT ( 'NONE',  ( 24.52499999999999858, 4.330127018922191873, 2.499999999999999556 ) ) ;
#66027 = CARTESIAN_POINT ( 'NONE',  ( -7.967954043666661671E-16, 14.32812499938548179, 34.33755215474603517 ) ) ;
#66028 = CARTESIAN_POINT ( 'NONE',  ( 26.67187500061451644, 3.027376345333611329, 5.243569643749999010 ) ) ;
#66029 = CARTESIAN_POINT ( 'NONE',  ( 1.071796769724495668, 17.43259618943233136, 34.00000000000000000 ) ) ;
#66030 = CARTESIAN_POINT ( 'NONE',  ( 12.48750000122903359, 4.330127018922191873, 2.499999999999999556 ) ) ;
#66031 = CARTESIAN_POINT ( 'NONE',  ( 3.112500000000000711, -5.773502691896255534, -1.060575238724906372E-15 ) ) ;
#66032 = CARTESIAN_POINT ( 'NONE',  ( 20.78732959644809952, -4.500000000000000000, 5.500000000000000888 ) ) ;
#66033 = CARTESIAN_POINT ( 'NONE',  ( 6.646875000614518747, -3.027376345333610441, -5.243569643749999898 ) ) ;
#66034 = CARTESIAN_POINT ( 'NONE',  ( 27.21562500061451928, -6.054752690667223547, -1.112240025338166033E-15 ) ) ;
#66035 = CYLINDRICAL_SURFACE ( 'NONE', #54313, 4.000000000000000000 ) ;
#66036 = CARTESIAN_POINT ( 'NONE',  ( 5.700000000000000178, 0.000000000000000000, 4.999999999999998224 ) ) ;
#66037 = CARTESIAN_POINT ( 'NONE',  ( -3.999999999999999112, 16.73750000000000071, 27.69059892324149530 ) ) ;
#66038 = CARTESIAN_POINT ( 'NONE',  ( 5.671875000614519102, -6.054752690667223547, -1.112240025338166033E-15 ) ) ;
#66039 = CARTESIAN_POINT ( 'NONE',  ( 9.159375000614515372, 0.000000000000000000, 5.243569643749999010 ) ) ;
#66040 = CARTESIAN_POINT ( 'NONE',  ( 29.48437500061451644, -4.541064518000419881, 2.621784821874995952 ) ) ;
#66041 = CARTESIAN_POINT ( 'NONE',  ( -4.243569643749998122, 12.64062500061459460, 32.45002607614398471 ) ) ;
#66042 = CARTESIAN_POINT ( 'NONE',  ( 21.71249999999999858, 2.886751345948129099, -4.999999999999998224 ) ) ;
#66043 = CARTESIAN_POINT ( 'NONE',  ( -3.999999999999997335, 17.78750000000000142, -27.69059892324149530 ) ) ;
#66044 = CARTESIAN_POINT ( 'NONE',  ( 5.287500000000000533, -2.886751345948129988, 4.999999999999997335 ) ) ;
#66045 = ORIENTED_EDGE ( 'NONE', *, *, #35732, .T. ) ;
#66046 = CARTESIAN_POINT ( 'NONE',  ( 18.89062500061451644, 6.054752690667223547, 3.707466751127219781E-16 ) ) ;
#66047 = CARTESIAN_POINT ( 'NONE',  ( 11.46562500061451573, -6.054752690667223547, -1.112240025338166033E-15 ) ) ;
#66048 = CARTESIAN_POINT ( 'NONE',  ( 20.22187500061451715, 4.119189519843966529, 2.378215178124999607 ) ) ;
#66049 = CARTESIAN_POINT ( 'NONE',  ( 7.884375000614517681, -4.541064518000419881, 2.621784821874995952 ) ) ;
#66050 = CARTESIAN_POINT ( 'NONE',  ( 23.02499999999999858, 6.123233995736764310E-16, -4.999999999999998224 ) ) ;
#66051 = CARTESIAN_POINT ( 'NONE',  ( 20.40000000122903145, -2.886751345948125991, -5.000000000000000000 ) ) ;
#66052 = CARTESIAN_POINT ( 'NONE',  ( 10.32187500061451679, 3.027376345333613106, -5.243569643749998122 ) ) ;
#66053 = CARTESIAN_POINT ( 'NONE',  ( 13.17187500061451999, 3.027376345333611329, 5.243569643749999010 ) ) ;
#66054 = CARTESIAN_POINT ( 'NONE',  ( 23.52187500061451786, 3.027376345333611329, 5.243569643749999010 ) ) ;
#66055 = CARTESIAN_POINT ( 'NONE',  ( 8.662500001229034297, -4.330127018922190985, -2.500000000000001332 ) ) ;
#66056 = ORIENTED_EDGE ( 'NONE', *, *, #59373, .T. ) ;
#66057 = CARTESIAN_POINT ( 'NONE',  ( 12.67499999999999893, 6.123233995736764310E-16, -4.999999999999998224 ) ) ;
#66058 = CARTESIAN_POINT ( 'NONE',  ( 18.30937500061451928, -4.541064518000417216, -2.621784821875001281 ) ) ;
#66059 = CARTESIAN_POINT ( 'NONE',  ( 8.596875000614518925, 6.054752690667223547, 3.707466751127219781E-16 ) ) ;
#66060 = CARTESIAN_POINT ( 'NONE',  ( -3.756430356249999214, 14.62812499938548250, 27.83122392262697531 ) ) ;
#66061 = CARTESIAN_POINT ( 'NONE',  ( 20.13749999999999929, -2.886751345948129988, 4.999999999999997335 ) ) ;
#66062 = CARTESIAN_POINT ( 'NONE',  ( 2.828200636599751609E-16, 16.21250000000000213, 25.38119784648299415 ) ) ;
#66063 = CARTESIAN_POINT ( 'NONE',  ( 0.000000000000000000, 20.00000000000000000, -33.99999999999999289 ) ) ;
#66064 = CARTESIAN_POINT ( 'NONE',  ( 22.92187500061451644, 2.746126346562645981, -4.756430356249997438 ) ) ;
#66065 = CARTESIAN_POINT ( 'NONE',  ( 12.14062500061451821, 6.054752690667223547, 3.707466751127219781E-16 ) ) ;
#66066 = CARTESIAN_POINT ( 'NONE',  ( 28.17187500061451644, -6.054752690667223547, -1.112240025338166033E-15 ) ) ;
#66067 =( BOUNDED_CURVE ( )  B_SPLINE_CURVE ( 2, ( #25002, #8382, #2477, #8020, #63442, #12828, #64896 ),
 .UNSPECIFIED., .F., .F. ) 
 B_SPLINE_CURVE_WITH_KNOTS ( ( 3, 2, 2, 3 ),
 ( 0.7100000000000001865, 0.7133333333333334858, 0.7166666666666667851, 0.7199999999999999734 ),
 .UNSPECIFIED. ) 
 CURVE ( )  GEOMETRIC_REPRESENTATION_ITEM ( )  RATIONAL_B_SPLINE_CURVE ( ( 0.9999999999999911182, 0.8660254037844475894, 1.000000000000000000, 0.8660254037844387076, 1.000000000000000000, 0.8660254037844387076, 1.000000000000000000 ) ) 
 REPRESENTATION_ITEM ( '' )  );
#66068 = CARTESIAN_POINT ( 'NONE',  ( 1.071796769724489895, 10.07990381179669903, -34.00000000000000000 ) ) ;
#66069 = CARTESIAN_POINT ( 'NONE',  ( 12.67499999999999893, 6.123233995736764310E-16, -4.999999999999998224 ) ) ;
#66070 = CARTESIAN_POINT ( 'NONE',  ( 2.000000000000001332, 17.11250000122903359, 33.46410161513774995 ) ) ;
#66071 = CARTESIAN_POINT ( 'NONE',  ( 12.48750000122903359, 4.330127018922191873, 2.499999999999999556 ) ) ;
#66072 = CARTESIAN_POINT ( 'NONE',  ( 23.52187500061451786, 3.027376345333611329, 5.243569643749999010 ) ) ;
#66073 = CARTESIAN_POINT ( 'NONE',  ( 15.98437500061451821, -4.541064518000419881, 2.621784821874995952 ) ) ;
#66074 = FACE_OUTER_BOUND ( 'NONE', #12348, .T. ) ;
#66075 = VERTEX_POINT ( 'NONE', #7475 ) ;
#66076 = CARTESIAN_POINT ( 'NONE',  ( 16.19062500061451715, 6.054752690667223547, 3.707466751127219781E-16 ) ) ;
#66077 = CARTESIAN_POINT ( 'NONE',  ( 2.840625000614518392, -3.027376345333614438, 5.243569643749998122 ) ) ;
#66078 = CARTESIAN_POINT ( 'NONE',  ( 16.62187500061451573, 3.027376345333613106, -5.243569643749998122 ) ) ;
#66079 = CARTESIAN_POINT ( 'NONE',  ( 5.278125000614516615, 6.421520780324663323E-16, -5.243569643749999010 ) ) ;
#66080 = CARTESIAN_POINT ( 'NONE',  ( 19.41562500061451146, 3.027376345333611329, 5.243569643749999010 ) ) ;
#66081 = CARTESIAN_POINT ( 'NONE',  ( -1.999999999999999112, 15.35000000000000142, 26.53589838486224650 ) ) ;
#66082 = CARTESIAN_POINT ( 'NONE',  ( 27.60937500061451644, 0.000000000000000000, 5.243569643749999010 ) ) ;
#66083 = CARTESIAN_POINT ( 'NONE',  ( -2.121784821874999949, 12.07812500061451821, 26.32496088578401938 ) ) ;
#66084 = CARTESIAN_POINT ( 'NONE',  ( 17.22187500061451715, 3.027376345333611329, 5.243569643749999010 ) ) ;
#66085 = CARTESIAN_POINT ( 'NONE',  ( 15.82500000122903216, -5.773502691896255534, -1.060575238724906372E-15 ) ) ;
#66086 = CARTESIAN_POINT ( 'NONE',  ( 10.09687500061451715, -2.746126346562646425, 4.756430356249996549 ) ) ;
#66087 = CARTESIAN_POINT ( 'NONE',  ( 8.849999999999999645, 0.000000000000000000, 4.999999999999998224 ) ) ;
#66088 = CARTESIAN_POINT ( 'NONE',  ( 21.45937500061451786, -4.541064518000417216, -2.621784821875001281 ) ) ;
#66089 = CARTESIAN_POINT ( 'NONE',  ( 21.82500000122903572, 2.886751345948129099, -4.999999999999998224 ) ) ;
#66090 = CARTESIAN_POINT ( 'NONE',  ( 23.16562500061451502, -6.054752690667223547, -1.112240025338166033E-15 ) ) ;
#66091 = CARTESIAN_POINT ( 'NONE',  ( 16.50937500061451502, -4.541064518000417216, -2.621784821875001281 ) ) ;
#66092 = CARTESIAN_POINT ( 'NONE',  ( 11.27812500061451573, 4.541064518000418104, 2.621784821874999949 ) ) ;
#66093 = CARTESIAN_POINT ( 'NONE',  ( -4.243569643749999898, 13.55937500061451750, 30.00000000000000000 ) ) ;
#66094 = CARTESIAN_POINT ( 'NONE',  ( 17.61562500061451786, 3.027376345333611329, 5.243569643749999010 ) ) ;
#66095 = CARTESIAN_POINT ( 'NONE',  ( 28.30312500061451431, 4.541064518000418104, -2.621784821874998173 ) ) ;
#66096 = ORIENTED_EDGE ( 'NONE', *, *, #22499, .F. ) ;
#66097 = ORIENTED_EDGE ( 'NONE', *, *, #70375, .T. ) ;
#66098 = CARTESIAN_POINT ( 'NONE',  ( 22.12500000000000000, 6.123233995736764310E-16, -4.999999999999998224 ) ) ;
#66099 = CARTESIAN_POINT ( 'NONE',  ( -4.243569643749999898, 19.37187500061451928, -32.45002607614398471 ) ) ;
#66100 = CARTESIAN_POINT ( 'NONE',  ( 45.00000000000000000, 9.426999614876460059E-14, 9.000000000000000000 ) ) ;
#66101 = CARTESIAN_POINT ( 'NONE',  ( 25.64062500061451644, 6.054752690667223547, 3.707466751127219781E-16 ) ) ;
#66102 = CARTESIAN_POINT ( 'NONE',  ( 5.690625000614516260, -3.027376345333610441, -5.243569643749999898 ) ) ;
#66103 = CARTESIAN_POINT ( 'NONE',  ( 16.80000000122903359, -2.886751345948125991, -5.000000000000000000 ) ) ;
#66104 = CARTESIAN_POINT ( 'NONE',  ( 21.74062500061451431, -3.027376345333614438, 5.243569643749998122 ) ) ;
#66105 = CARTESIAN_POINT ( 'NONE',  ( 23.36250000000000071, -5.773502691896255534, -1.060575238724906372E-15 ) ) ;
#66106 = CARTESIAN_POINT ( 'NONE',  ( 24.77812500061451217, 4.541064518000418104, 2.621784821874999949 ) ) ;
#66107 = CARTESIAN_POINT ( 'NONE',  ( 7.340625000614518392, -3.027376345333614438, 5.243569643749998122 ) ) ;
#66108 = EDGE_LOOP ( 'NONE', ( #36284, #18072 ) ) ;
#66109 = ADVANCED_FACE ( 'NONE', ( #15107 ), #65351, .F. ) ;
#66110 = CARTESIAN_POINT ( 'NONE',  ( 23.35312500061451857, 4.541064518000418104, -2.621784821874998173 ) ) ;
#66111 = CARTESIAN_POINT ( 'NONE',  ( 3.815625000614518036, -6.054752690667223547, -1.112240025338166033E-15 ) ) ;
#66112 = CARTESIAN_POINT ( 'NONE',  ( 12.72187500061451537, 2.746126346562643317, 4.756430356249998326 ) ) ;
#66113 = CARTESIAN_POINT ( 'NONE',  ( 11.10000000122903252, 5.773502691896255534, 3.535250795749688401E-16 ) ) ;
#66114 = CARTESIAN_POINT ( 'NONE',  ( -3.999999999999999112, 14.71250000122903501, -30.00000000000000000 ) ) ;
#66115 =( BOUNDED_CURVE ( )  B_SPLINE_CURVE ( 2, ( #24871, #69948, #2718, #25234, #46699, #24514, #34875, #52597, #64401 ),
 .UNSPECIFIED., .F., .F. ) 
 B_SPLINE_CURVE_WITH_KNOTS ( ( 3, 2, 2, 2, 3 ),
 ( 0.07608695652173913526, 0.07971014492753622505, 0.08695652173913043237, 0.09420289855072463969, 0.09782608695652174335 ),
 .UNSPECIFIED. ) 
 CURVE ( )  GEOMETRIC_REPRESENTATION_ITEM ( )  RATIONAL_B_SPLINE_CURVE ( ( 0.9330127018922192983, 0.9330127018922194093, 1.000000000000000000, 0.8660254037844387076, 1.000000000000000000, 0.8660254037844387076, 1.000000000000000000, 0.9330127018922194093, 0.9330127018922194093 ) ) 
 REPRESENTATION_ITEM ( '' )  );
#66116 = CARTESIAN_POINT ( 'NONE',  ( 10.65000000000000036, 0.000000000000000000, 4.999999999999998224 ) ) ;
#66117 = CARTESIAN_POINT ( 'NONE',  ( 10.43437500061451750, 4.541064518000418104, 2.621784821874999949 ) ) ;
#66118 = CARTESIAN_POINT ( 'NONE',  ( 5.325000001229033941, 2.886751345948126879, 4.999999999999999112 ) ) ;
#66119 = CARTESIAN_POINT ( 'NONE',  ( 15.23437500061451644, 6.421520780324663323E-16, -5.243569643749999010 ) ) ;
#66120 = CARTESIAN_POINT ( 'NONE',  ( 6.759375000614516793, 4.541064518000418104, -2.621784821874998173 ) ) ;
#66121 = CARTESIAN_POINT ( 'NONE',  ( 30.00000000000000000, 6.123233995736764310E-16, -4.999999999999998224 ) ) ;
#66122 = CARTESIAN_POINT ( 'NONE',  ( 0.000000000000000000, 20.00000000000000000, 30.00000000000000000 ) ) ;
#66123 = CARTESIAN_POINT ( 'NONE',  ( 12.87187500061451750, -6.054752690667223547, -1.112240025338166033E-15 ) ) ;
#66124 = CARTESIAN_POINT ( 'NONE',  ( 6.187500001229032875, 4.330127018922191873, 2.499999999999999556 ) ) ;
#66125 = CARTESIAN_POINT ( 'NONE',  ( 21.62812500061451360, 4.541064518000418104, 2.621784821874999949 ) ) ;
#66126 = CARTESIAN_POINT ( 'NONE',  ( -4.243569643749999898, 19.85937500061451644, 30.00000000000000000 ) ) ;
#66127 = CYLINDRICAL_SURFACE ( 'NONE', #30190, 3.999999999999996447 ) ;
#66128 = CARTESIAN_POINT ( 'NONE',  ( 22.73437500061451644, -4.541064518000419881, 2.621784821874995952 ) ) ;
#66129 = CARTESIAN_POINT ( 'NONE',  ( 4.092234022020802442, 2.872911538668597053, -4.251154360391494080 ) ) ;
#66130 =( BOUNDED_CURVE ( )  B_SPLINE_CURVE ( 2, ( #27218, #45204, #49753, #67737, #21659, #39669, #11585 ),
 .UNSPECIFIED., .F., .F. ) 
 B_SPLINE_CURVE_WITH_KNOTS ( ( 3, 2, 2, 3 ),
 ( 0.2916666666666667407, 0.2944444444444445086, 0.2972222222222222210, 0.2999999999999999889 ),
 .UNSPECIFIED. ) 
 CURVE ( )  GEOMETRIC_REPRESENTATION_ITEM ( )  RATIONAL_B_SPLINE_CURVE ( ( 0.9999999999999973355, 0.8660254037844413721, 1.000000000000000000, 0.8660254037844387076, 1.000000000000000000, 0.8660254037844387076, 1.000000000000000000 ) ) 
 REPRESENTATION_ITEM ( '' )  );
#66131 = CARTESIAN_POINT ( 'NONE',  ( 27.86250000122903359, 0.000000000000000000, 4.999999999999998224 ) ) ;
#66132 = CARTESIAN_POINT ( 'NONE',  ( 18.94687500061451857, 0.000000000000000000, 4.756430356249998326 ) ) ;
#66133 = CARTESIAN_POINT ( 'NONE',  ( 26.16562500061451502, 3.027376345333611329, 5.243569643749999010 ) ) ;
#66134 = CARTESIAN_POINT ( 'NONE',  ( 17.61562500061451786, 3.027376345333611329, 5.243569643749999010 ) ) ;
#66135 = CARTESIAN_POINT ( 'NONE',  ( 14.60625000122903216, 4.330127018922192761, -2.499999999999997780 ) ) ;
#66136 = CARTESIAN_POINT ( 'NONE',  ( 15.45937500061451608, 0.000000000000000000, 5.243569643749999010 ) ) ;
#66137 = CARTESIAN_POINT ( 'NONE',  ( -1.243387493232115393E-14, 15.76249999999999929, 26.00000000000000000 ) ) ;
#66138 = CARTESIAN_POINT ( 'NONE',  ( 28.46250000122903145, -4.330127018922190985, -2.500000000000001332 ) ) ;
#66139 = CARTESIAN_POINT ( 'NONE',  ( 5.709375000614517859, -4.541064518000417216, -2.621784821875001281 ) ) ;
#66140 = CARTESIAN_POINT ( 'NONE',  ( 16.05937500061451573, -4.541064518000417216, -2.621784821875001281 ) ) ;
#66141 = DIRECTION ( 'NONE',  ( 0.000000000000000000, 0.000000000000000000, 1.000000000000000000 ) ) ;
#66142 = CARTESIAN_POINT ( 'NONE',  ( 23.13749999999999929, 5.773502691896255534, 3.535250795749688894E-16 ) ) ;
#66143 = CARTESIAN_POINT ( 'NONE',  ( 16.76250000122903216, -4.330127018922190985, -2.500000000000001332 ) ) ;
#66144 = CARTESIAN_POINT ( 'NONE',  ( 25.17187500061451644, 3.027376345333613106, -5.243569643749998122 ) ) ;
#66145 = CARTESIAN_POINT ( 'NONE',  ( 15.64687500061451608, -3.027376345333610441, -5.243569643749999898 ) ) ;
#66146 = CARTESIAN_POINT ( 'NONE',  ( -3.756430356249999214, 13.39062499938548179, 27.83122392262697531 ) ) ;
#66147 = CARTESIAN_POINT ( 'NONE',  ( 28.80000000000000071, -4.330127018922190985, -2.500000000000001332 ) ) ;
#66148 = CARTESIAN_POINT ( 'NONE',  ( 6.299999999999999822, -4.330127018922190985, -2.500000000000001332 ) ) ;
#66149 = CARTESIAN_POINT ( 'NONE',  ( 9.046875000614514661, 0.000000000000000000, 4.756430356249998326 ) ) ;
#66150 = CARTESIAN_POINT ( 'NONE',  ( 20.61562500061451431, 3.027376345333613106, -5.243569643749998122 ) ) ;
#66151 = CARTESIAN_POINT ( 'NONE',  ( 9.037499999999999645, -2.886751345948125991, -5.000000000000000000 ) ) ;
#66152 = CARTESIAN_POINT ( 'NONE',  ( 4.078125000614517326, 4.541064518000418104, 2.621784821874999949 ) ) ;
#66153 = CARTESIAN_POINT ( 'NONE',  ( 19.23749999999999716, -2.886751345948129988, 4.999999999999997335 ) ) ;
#66154 = EDGE_CURVE ( 'NONE', #70620, #68959, #8452, .T. ) ;
#66155 = CARTESIAN_POINT ( 'NONE',  ( 15.52500000122903323, 2.886751345948129099, -4.999999999999997335 ) ) ;
#66156 = CARTESIAN_POINT ( 'NONE',  ( 24.03750000122903430, 6.123233995736764310E-16, -4.999999999999998224 ) ) ;
#66157 = CARTESIAN_POINT ( 'NONE',  ( 3.203040009831848334, 9.474684130322209796, 35.07722138099716602 ) ) ;
#66158 =( BOUNDED_CURVE ( )  B_SPLINE_CURVE ( 1, ( #67477, #45297 ),
 .UNSPECIFIED., .F., .F. ) 
 B_SPLINE_CURVE_WITH_KNOTS ( ( 2, 2 ),
 ( 0.000000000000000000, 1.000000000000000000 ),
 .UNSPECIFIED. ) 
 CURVE ( )  GEOMETRIC_REPRESENTATION_ITEM ( )  RATIONAL_B_SPLINE_CURVE ( ( 0.9401542295229587953, 0.9401542295229587953 ) ) 
 REPRESENTATION_ITEM ( '' )  );
#66159 = CARTESIAN_POINT ( 'NONE',  ( 3.187500000000002220, -2.886751345948125991, -5.000000000000000000 ) ) ;
#66160 = ORIENTED_EDGE ( 'NONE', *, *, #14417, .T. ) ;
#66161 = CARTESIAN_POINT ( 'NONE',  ( 17.99062500061451786, 6.054752690667223547, 3.707466751127219781E-16 ) ) ;
#66162 = CARTESIAN_POINT ( 'NONE',  ( 23.42812500061451786, 4.541064518000418104, 2.621784821874999949 ) ) ;
#66163 = CARTESIAN_POINT ( 'NONE',  ( 24.49687500061451573, -3.027376345333614438, 5.243569643749998122 ) ) ;
#66164 = CARTESIAN_POINT ( 'NONE',  ( 9.262499999999999289, 2.886751345948126879, 4.999999999999999112 ) ) ;
#66165 = CARTESIAN_POINT ( 'NONE',  ( 11.76562500061451644, 3.027376345333611329, 5.243569643749999010 ) ) ;
#66166 = CARTESIAN_POINT ( 'NONE',  ( 26.65312500061451573, 0.000000000000000000, 5.243569643749999010 ) ) ;
#66167 = CARTESIAN_POINT ( 'NONE',  ( 13.73437500061451821, -4.541064518000419881, 2.621784821874995952 ) ) ;
#66168 = CARTESIAN_POINT ( 'NONE',  ( 19.24687500061452283, -3.027376345333610441, -5.243569643749999898 ) ) ;
#66169 = CARTESIAN_POINT ( 'NONE',  ( 2.970509043979068231, -4.022057219312137555, 3.237209742923575106 ) ) ;
#66170 = CARTESIAN_POINT ( 'NONE',  ( 5.190092854996874117, 9.755146338944483020, 24.77581305162949832 ) ) ;
#66171 = CARTESIAN_POINT ( 'NONE',  ( 24.30000000122903359, -2.886751345948129988, 4.999999999999997335 ) ) ;
#66172 = CARTESIAN_POINT ( 'NONE',  ( 18.12187500061451928, 2.746126346562643317, 4.756430356249998326 ) ) ;
#66173 = CARTESIAN_POINT ( 'NONE',  ( 14.05312500061451431, 0.000000000000000000, 5.243569643749999010 ) ) ;
#66174 = CARTESIAN_POINT ( 'NONE',  ( 6.946875000614517681, -3.027376345333614438, 5.243569643749998122 ) ) ;
#66175 = CARTESIAN_POINT ( 'NONE',  ( 8.146875000614516082, 6.054752690667223547, 3.707466751127219781E-16 ) ) ;
#66176 = VERTEX_POINT ( 'NONE', #3312 ) ;
#66177 = CARTESIAN_POINT ( 'NONE',  ( 26.59687500061451360, 6.054752690667223547, 3.707466751127219781E-16 ) ) ;
#66178 = CARTESIAN_POINT ( 'NONE',  ( 20.50312500061451715, -4.541064518000417216, -2.621784821875001281 ) ) ;
#66179 = CARTESIAN_POINT ( 'NONE',  ( 3.384375000614517237, -4.541064518000419881, 2.621784821874995952 ) ) ;
#66180 = CARTESIAN_POINT ( 'NONE',  ( 24.87187500061451573, 3.027376345333611329, 5.243569643749999010 ) ) ;
#66181 = CARTESIAN_POINT ( 'NONE',  ( 19.45312500061451644, 0.000000000000000000, 5.243569643749999010 ) ) ;
#66182 = CARTESIAN_POINT ( 'NONE',  ( -3.999999999999997335, 11.48750000000000071, 32.30940107675850470 ) ) ;
#66183 = CARTESIAN_POINT ( 'NONE',  ( 24.55312500061451786, -4.541064518000417216, -2.621784821875001281 ) ) ;
#66184 = CARTESIAN_POINT ( 'NONE',  ( 7.612500001229035362, 0.000000000000000000, 4.999999999999998224 ) ) ;
#66185 = ORIENTED_EDGE ( 'NONE', *, *, #19403, .T. ) ;
#66186 = CARTESIAN_POINT ( 'NONE',  ( 2.662500001229036073, 0.000000000000000000, 4.999999999999998224 ) ) ;
#66187 = CARTESIAN_POINT ( 'NONE',  ( -3.999999999999997335, 15.98750000000000249, -27.69059892324149175 ) ) ;
#66188 = CARTESIAN_POINT ( 'NONE',  ( 22.08750000122903501, -4.330127018922194537, 2.499999999999995559 ) ) ;
#66189 = CARTESIAN_POINT ( 'NONE',  ( -1.878215178125001827, 15.75312499938548427, 33.25316411605952283 ) ) ;
#66190 = EDGE_CURVE ( 'NONE', #72082, #72537, #12651, .T. ) ;
#66191 = CARTESIAN_POINT ( 'NONE',  ( 4.696875000614518569, -3.027376345333614438, 5.243569643749998122 ) ) ;
#66192 = CARTESIAN_POINT ( 'NONE',  ( 29.31562500061451715, 3.027376345333611329, 5.243569643749999010 ) ) ;
#66193 = CARTESIAN_POINT ( 'NONE',  ( 12.74062500061451786, -3.027376345333614438, 5.243569643749998122 ) ) ;
#66194 = CARTESIAN_POINT ( 'NONE',  ( 5.896875000614518747, 6.054752690667223547, 3.707466751127219781E-16 ) ) ;
#66195 = CARTESIAN_POINT ( 'NONE',  ( 23.55000000122903359, -2.886751345948125991, -5.000000000000000000 ) ) ;
#66196 = CARTESIAN_POINT ( 'NONE',  ( 15.45937500061451608, 0.000000000000000000, 5.243569643749999010 ) ) ;
#66197 = CARTESIAN_POINT ( 'NONE',  ( 28.79062500061451502, 6.054752690667223547, 3.707466751127219781E-16 ) ) ;
#66198 = CARTESIAN_POINT ( 'NONE',  ( 29.32499999999999929, 6.123233995736764310E-16, -4.999999999999998224 ) ) ;
#66199 = CARTESIAN_POINT ( 'NONE',  ( 5.540625000614515905, -3.027376345333614438, 5.243569643749998122 ) ) ;
#66200 = CARTESIAN_POINT ( 'NONE',  ( 14.12812500061451715, -4.541064518000419881, 2.621784821874995952 ) ) ;
#66201 = ORIENTED_EDGE ( 'NONE', *, *, #58318, .T. ) ;
#66202 = CARTESIAN_POINT ( 'NONE',  ( 10.71562500061451928, 3.027376345333613106, -5.243569643749998122 ) ) ;
#66203 = CARTESIAN_POINT ( 'NONE',  ( 8.053125000614516082, 4.541064518000418104, -2.621784821874998173 ) ) ;
#66204 = CARTESIAN_POINT ( 'NONE',  ( 19.17187500061451999, -5.492252693125287522, -1.008910452111647106E-15 ) ) ;
#66205 = CARTESIAN_POINT ( 'NONE',  ( 7.762500000000001954, 2.886751345948129099, -4.999999999999998224 ) ) ;
#66206 = CARTESIAN_POINT ( 'NONE',  ( 4.500000001229034652, -2.886751345948129988, 4.999999999999997335 ) ) ;
#66207 = CARTESIAN_POINT ( 'NONE',  ( 18.93750000000000000, -2.886751345948125991, -5.000000000000000000 ) ) ;
#66208 = CARTESIAN_POINT ( 'NONE',  ( 18.23437500061451999, -4.541064518000419881, 2.621784821874995952 ) ) ;
#66209 = CARTESIAN_POINT ( 'NONE',  ( 13.72500000122903074, 2.886751345948129099, -4.999999999999998224 ) ) ;
#66210 = CARTESIAN_POINT ( 'NONE',  ( 21.82499999999999574, 4.330127018922191873, 2.499999999999999556 ) ) ;
#66211 = CARTESIAN_POINT ( 'NONE',  ( 4.243569643749999898, 17.32812500061451644, -30.00000000000000000 ) ) ;
#66212 = B_SPLINE_CURVE_WITH_KNOTS ( 'NONE', 3,
 ( #4982, #16411, #39330, #11610, #61844, #56667, #27514, #28597, #51133, #45599 ),
 .UNSPECIFIED., .F., .F.,
 ( 4, 3, 3, 4 ),
 ( 1.879119738154566656E-16, 0.0001572461267887791201, 0.0003144877809832584913, 0.0005153498092345547071 ),
 .UNSPECIFIED. ) ;
#66213 = CARTESIAN_POINT ( 'NONE',  ( 14.53125000122903288, 6.123233995736764310E-16, -4.999999999999998224 ) ) ;
#66214 = CARTESIAN_POINT ( 'NONE',  ( 29.61562500061451431, 3.027376345333613106, -5.243569643749998122 ) ) ;
#66215 = CARTESIAN_POINT ( 'NONE',  ( 28.19999999999999929, 0.000000000000000000, 4.999999999999998224 ) ) ;
#66216 = CARTESIAN_POINT ( 'NONE',  ( 24.26249999999999929, -5.773502691896255534, -1.060575238724906372E-15 ) ) ;
#66217 = CARTESIAN_POINT ( 'NONE',  ( 13.80937500061451750, -4.541064518000417216, -2.621784821875001281 ) ) ;
#66218 = CARTESIAN_POINT ( 'NONE',  ( 27.56250000000000000, 2.886751345948129099, -4.999999999999998224 ) ) ;
#66219 = CARTESIAN_POINT ( 'NONE',  ( 11.76562500061451644, 3.027376345333611329, 5.243569643749999010 ) ) ;
#66220 = CARTESIAN_POINT ( 'NONE',  ( 27.15937500061451360, -5.492252693125287522, -1.008910452111647106E-15 ) ) ;
#66221 = CARTESIAN_POINT ( 'NONE',  ( 22.20937500061451431, 0.000000000000000000, 5.243569643749999010 ) ) ;
#66222 = CARTESIAN_POINT ( 'NONE',  ( 14.22187500061451537, 5.824947211148865298E-16, -4.756430356249998326 ) ) ;
#66223 = CARTESIAN_POINT ( 'NONE',  ( 8.315625000614515372, -6.054752690667223547, -1.112240025338166033E-15 ) ) ;
#66224 = CARTESIAN_POINT ( 'NONE',  ( 13.95937500061451786, 4.541064518000418104, -2.621784821874998173 ) ) ;
#66225 = EDGE_LOOP ( 'NONE', ( #69536, #61822, #49121, #11730 ) ) ;
#66226 = CARTESIAN_POINT ( 'NONE',  ( 24.30937500061451573, 4.541064518000418104, -2.621784821874998173 ) ) ;
#66227 = CARTESIAN_POINT ( 'NONE',  ( -3.305247878049081707E-15, 5.000000000000034639, -34.00000000000004263 ) ) ;
#66228 = CARTESIAN_POINT ( 'NONE',  ( 24.82499999999999929, 6.123233995736764310E-16, -4.999999999999998224 ) ) ;
#66229 = CARTESIAN_POINT ( 'NONE',  ( 4.612500000000002487, 2.886751345948129099, -4.999999999999998224 ) ) ;
#66230 = CARTESIAN_POINT ( 'NONE',  ( 17.81250000122903288, 4.330127018922192761, -2.499999999999997780 ) ) ;
#66231 = FACE_OUTER_BOUND ( 'NONE', #8200, .T. ) ;
#66232 = CARTESIAN_POINT ( 'NONE',  ( 3.752440054025286909, -3.304420318444254878, 4.071342403668507082 ) ) ;
#66233 = AXIS2_PLACEMENT_3D ( 'NONE', #38462, #33639, #5207 ) ;
#66234 = ORIENTED_EDGE ( 'NONE', *, *, #19843, .F. ) ;
#66235 = CARTESIAN_POINT ( 'NONE',  ( 14.10000000000000142, 4.330127018922192761, -2.499999999999997780 ) ) ;
#66236 = CARTESIAN_POINT ( 'NONE',  ( 17.73750000000000071, 5.773502691896255534, 3.535250795749688894E-16 ) ) ;
#66237 = CARTESIAN_POINT ( 'NONE',  ( 11.24062500061451608, 6.054752690667223547, 3.707466751127219781E-16 ) ) ;
#66238 = EDGE_CURVE ( 'NONE', #11468, #29843, #62201, .T. ) ;
#66239 = ORIENTED_EDGE ( 'NONE', *, *, #30133, .F. ) ;
#66240 = CARTESIAN_POINT ( 'NONE',  ( 26.25000000000000000, 4.330127018922192761, -2.499999999999997780 ) ) ;
#66241 = CARTESIAN_POINT ( 'NONE',  ( -3.000416591977282496E-16, 17.49687500061451573, -34.90005215228797653 ) ) ;
#66242 = CARTESIAN_POINT ( 'NONE',  ( 4.415625000614518569, 3.027376345333613106, -5.243569643749998122 ) ) ;
#66243 = CARTESIAN_POINT ( 'NONE',  ( -7.967954043666661671E-16, 13.87812499938548250, 34.33755215474603517 ) ) ;
#66244 = CARTESIAN_POINT ( 'NONE',  ( 8.887499999999999289, -2.886751345948129988, 4.999999999999997335 ) ) ;
#66245 = CYLINDRICAL_SURFACE ( 'NONE', #57396, 4.999999999999998224 ) ;
#66246 = ORIENTED_EDGE ( 'NONE', *, *, #27328, .F. ) ;
#66247 = CARTESIAN_POINT ( 'NONE',  ( 23.27812500061451573, 6.421520780324663323E-16, -5.243569643749999010 ) ) ;
#66248 = CARTESIAN_POINT ( 'NONE',  ( 4.192336996406676342, -2.724758798235080715, 4.480034832487019614 ) ) ;
#66249 = CARTESIAN_POINT ( 'NONE',  ( 2.655984681222220721E-16, 19.50312499938548427, 25.66244784525396483 ) ) ;
#66250 = CARTESIAN_POINT ( 'NONE',  ( 21.45937500061451786, -4.541064518000417216, -2.621784821875001281 ) ) ;
#66251 = ADVANCED_FACE ( 'NONE', ( #67559 ), #56106, .F. ) ;
#66252 = CARTESIAN_POINT ( 'NONE',  ( 18.96562500061451573, 3.027376345333611329, 5.243569643749999010 ) ) ;
#66253 = CARTESIAN_POINT ( 'NONE',  ( -2.121784821874999949, 14.32812500061459282, -33.67503911421598417 ) ) ;
#66254 = CARTESIAN_POINT ( 'NONE',  ( 23.96250000122903145, -4.330127018922190985, -2.500000000000001332 ) ) ;
#66255 = CARTESIAN_POINT ( 'NONE',  ( 4.753125000614515372, -4.541064518000417216, -2.621784821875001281 ) ) ;
#66256 = CARTESIAN_POINT ( 'NONE',  ( 23.78437500061451360, 5.824947211148865298E-16, -4.756430356249998326 ) ) ;
#66257 = CARTESIAN_POINT ( 'NONE',  ( 22.64062500061451644, -3.027376345333614438, 5.243569643749998122 ) ) ;
#66258 = CARTESIAN_POINT ( 'NONE',  ( 9.046875000614518214, 5.492252693125287522, 3.363034840372157021E-16 ) ) ;
#66259 = CARTESIAN_POINT ( 'NONE',  ( -3.756430356250001434, 18.30312499938548143, 32.16877607737301048 ) ) ;
#66261 = EDGE_CURVE ( 'NONE', #11494, #29428, #38824, .T. ) ;
#66260 = CARTESIAN_POINT ( 'NONE',  ( 14.89687500061451786, 6.054752690667223547, 3.707466751127219781E-16 ) ) ;
#66262 = CARTESIAN_POINT ( 'NONE',  ( 13.73437500061451821, -4.541064518000419881, 2.621784821874995952 ) ) ;
#66263 = CARTESIAN_POINT ( 'NONE',  ( 23.37187500061451573, 3.027376345333613106, -5.243569643749998122 ) ) ;
#66264 = ORIENTED_EDGE ( 'NONE', *, *, #45500, .F. ) ;
#66265 = CARTESIAN_POINT ( 'NONE',  ( 9.001249775931846008E-16, 11.42187500061451644, 34.90005215228797653 ) ) ;
#66266 = CYLINDRICAL_SURFACE ( 'NONE', #58262, 4.999999999999998224 ) ;
#66267 = CARTESIAN_POINT ( 'NONE',  ( 27.44062500061451715, 6.054752690667223547, 3.707466751127219781E-16 ) ) ;
#66268 = CARTESIAN_POINT ( 'NONE',  ( 27.17812500061451786, -4.541064518000419881, 2.621784821874995952 ) ) ;
#66269 = CARTESIAN_POINT ( 'NONE',  ( 3.999999999999999112, 19.43750000122903288, -30.00000000000000000 ) ) ;
#66270 = DIRECTION ( 'NONE',  ( 0.000000000000000000, 0.000000000000000000, -1.000000000000000000 ) ) ;
#66271 = CARTESIAN_POINT ( 'NONE',  ( 6.046875000614519102, -3.027376345333614438, 5.243569643749998122 ) ) ;
#66272 = CARTESIAN_POINT ( 'NONE',  ( 0.000000000000000000, 0.000000000000000000, 0.000000000000000000 ) ) ;
#66273 = CARTESIAN_POINT ( 'NONE',  ( 14.77500000122903501, 2.886751345948126879, 4.999999999999999112 ) ) ;
#66274 = CARTESIAN_POINT ( 'NONE',  ( 9.975000001229034297, -5.773502691896255534, -1.060575238724906372E-15 ) ) ;
#66275 = CARTESIAN_POINT ( 'NONE',  ( 2.990625000614519191, -3.027376345333610441, -5.243569643749999898 ) ) ;
#66276 = CARTESIAN_POINT ( 'NONE',  ( 3.999999999999998668, 16.00624999877096499, 32.30940107675850470 ) ) ;
#66277 = CARTESIAN_POINT ( 'NONE',  ( 17.86875000122903145, 2.886751345948126879, 4.999999999999999112 ) ) ;
#66278 = CARTESIAN_POINT ( 'NONE',  ( 12.68437500061451573, 4.541064518000418104, 2.621784821874999949 ) ) ;
#66279 = DIRECTION ( 'NONE',  ( -0.000000000000000000, -1.000000000000000000, -0.000000000000000000 ) ) ;
#66280 = ORIENTED_EDGE ( 'NONE', *, *, #22854, .F. ) ;
#66281 = CARTESIAN_POINT ( 'NONE',  ( 20.84062500061451573, -3.027376345333614438, 5.243569643749998122 ) ) ;
#66282 = CARTESIAN_POINT ( 'NONE',  ( 15.08437500061451786, -4.541064518000419881, 2.621784821874995952 ) ) ;
#66283 = CARTESIAN_POINT ( 'NONE',  ( 5.240625000614516971, -3.027376345333610441, -5.243569643749999898 ) ) ;
#66284 = CARTESIAN_POINT ( 'NONE',  ( 21.00937500061451857, -4.541064518000417216, -2.621784821875001281 ) ) ;
#66285 = CARTESIAN_POINT ( 'NONE',  ( 5.990625000614517859, -3.027376345333614438, 5.243569643749998122 ) ) ;
#66286 = FACE_OUTER_BOUND ( 'NONE', #1155, .T. ) ;
#66287 = CARTESIAN_POINT ( 'NONE',  ( 6.937500001229033764, 6.123233995736764310E-16, -4.999999999999998224 ) ) ;
#66288 = CARTESIAN_POINT ( 'NONE',  ( 23.50312500061451360, 0.000000000000000000, 5.243569643749999010 ) ) ;
#66289 = CARTESIAN_POINT ( 'NONE',  ( -1.999999999999997113, 18.83750000122903501, -26.53589838486224295 ) ) ;
#66290 = CARTESIAN_POINT ( 'NONE',  ( 7.612500001229035362, 0.000000000000000000, 4.999999999999998224 ) ) ;
#66291 = CARTESIAN_POINT ( 'NONE',  ( 19.15312500061451573, -4.541064518000417216, -2.621784821875001281 ) ) ;
#66292 = CARTESIAN_POINT ( 'NONE',  ( 14.65312500061451573, -4.541064518000417216, -2.621784821875001281 ) ) ;
#66293 = CARTESIAN_POINT ( 'NONE',  ( 28.50937500061451502, 0.000000000000000000, 4.756430356249998326 ) ) ;
#66294 = CARTESIAN_POINT ( 'NONE',  ( 15.22500000000000142, -4.330127018922194537, 2.499999999999995559 ) ) ;
#66295 = CARTESIAN_POINT ( 'NONE',  ( 11.32500000122903394, -5.773502691896255534, -1.060575238724906372E-15 ) ) ;
#66296 = EDGE_CURVE ( 'NONE', #52378, #69635, #13620, .T. ) ;
#66297 = CARTESIAN_POINT ( 'NONE',  ( 9.140625000614518214, -3.027376345333614438, 5.243569643749998122 ) ) ;
#66298 = CARTESIAN_POINT ( 'NONE',  ( 11.65312500061451573, 4.541064518000418104, -2.621784821874998173 ) ) ;
#66299 =( BOUNDED_SURFACE ( )  B_SPLINE_SURFACE ( 1, 2, ( 
 ( #36923, #70913, #48750, #3322, #59444, #59078, #71274, #20652, #36194, #15115, #25099, #41735, #8851, #4054, #65730, #20284, #25474, #64263, #26580, #58712, #53927, #14019, #25848, #53549, #65360, #2946, #42475, #14750, #37652, #49120, #32116, #42110, #8124, #64633, #70546, #23116, #61919, #33475, #51930, #62644, #66095, #56024, #21021, #245, #22754, #68207, #40486, #46028, #5415, #16846, #39038, #10954, #33845, #17568, #73013, #6138, #39774, #12040, #57092, #27955, #50487, #28668, #11324, #22397, #6501, #34202, #50846, #29037, #51209, #44945, #67483, #39402, #16480, #51572, #56389, #63001, #34564, #61552, #971, #12395, #609, #5779, #28310, #45305, #67840, #17212, #62290, #68564, #40130, #23481, #11686, #56736, #6864, #34932, #17922, #45671, #57458, #29396, #43574, #13112, #70000, #52288, #58532, #19004, #41927, #36384, #35291, #12755, #7943, #63720, #57812, #58898, #13466, #30112, #8309, #30481, #7222, #29750, #63371, #46387, #30839, #1689, #19745, #64453, #18278, #13844, #64819, #53009, #68922, #46752, #69286, #24199, #18650, #7577, #47838, #19370, #53372, #24564, #41212, #59264, #2769, #25292, #42294, #35652, #23838, #36744, #64084, #58172, #52647, #70367, #2404, #14208, #36014, #2053, #69642, #47110, #8673, #41565, #40853, #24925, #47467, #31204, #1327, #26399, #38205, #20104, #59633, #71840, #66288, #43399, #3877, #72201, #25668, #55214, #65183, #48941, #60363, #49306, #15304, #71470, #71098, #21211, #32674, #48205, #27139, #14574, #53745, #20846, #16037, #60733, #32306, #37481, #3142, #66660, #70727, #65924, #26032, #37842, #20471, #9772, #48571, #31942, #54840, #43764, #38585, #15667, #42659, #10142, #4247, #21579, #26774, #43025, #37107, #10507, #4609, #9046, #31577, #54115, #54478, #49673, #44133, #65553, #3512, #14943, #60002, #61110, #9411, #51121, #56304, #72929, #17833, #518, #62557, #51483, #50405, #55575, #68471, #22668, #16761, #22311, #6413, #17124, #23029, #45219, #11237, #28229, #33759, #34478, #61471, #4969, #67752, #10866, #62203, #33035, #5693, #17483, #72562, #38953, #45584, #68117, #39684, #50759, #884, #27503, #57007, #44505, #162, #11599, #28584, #34116, #56655, #44863, #40044, #11953, #50036, #28945, #67038, #21948, #6050, #40394, #23391, #45940, #39319, #16398, #62913, #33399, #55936, #5331, #27872, #67400, #61831, #57729, #63637, #1969, #30394, #25198, #7858, #1243, #52923, #18920, #30751, #13380, #52201, #23748, #42208, #2321, #57369, #46296, #12307, #13026, #35565, #58447, #53283, #36299, #68836, #7135, #29309, #18193, #24113, #24836, #63278, #69559, #30019, #47384, #69914, #40763, #12670, #41480, #1602, #35207, #19284, #24478, #41126, #41835, #64000, #29665, #46662, #69201, #6777, #64366, #18561, #2682, #13756, #51840, #58812, #47744, #35923, #58084, #7492, #8223, #52563, #70281, #34843, #19652, #47024, #31856, #65462, #42937, #4524, #59917, #3048, #70641, #42569, #15578, #26312, #43313, #49583, #43677, #65097, #8586, #37021, #21491, #48850, #54031, #9687, #4156, #14487, #14854, #48486, #64732, #55126, #37393, #21124, #38120, #3426, #31116, #25946, #54391, #32587, #59545, #9323, #31490, #32220, #53654, #8957, #71010, #27053, #14119, #20386, #3789, #20755, #20016, #60641, #65833, #10054, #71380, #72107, #59177, #15215, #60273, #37755, #54754, #36657, #25578, #26688, #48118, #49221, #71755, #66200, #34027, #11505, #28144, #39229, #67664, #61741, #33671, #11142, #51389, #62467, #72470, #62112, #27415, #56564, #27780, #44779, #17030, #49946, #5239, #10779, #21855, #10418, #50319, #5608, #791, #44044, #38495, #44418, #56215, #66945, #50672, #76, #66567, #22581, #32949, #45492, #72842, #15947, #67313, #45130, #55486, #38866, #4879, #39588, #16313, #22224, #5960, #33312, #28494, #16671, #55850, #51030, #61383, #426, #61020, #68025, #22934, #17397, #39954, #11865, #34386, #56918, #6322, #28851, #63909, #62827, #23663, #68748, #36207, #53196, #18106, #46208, #52474, #51754, #69829, #1881, #47294, #35476, #58725, #17746, #18474, #18831, #41038, #69114, #23301, #8137, #63187, #12220, #7768, #30304, #30663, #13295, #35833, #7406, #63553, #46937, #12939, #57997, #29934, #45850, #41747, #1154, #41394, #6689, #58356, #7047, #24021, #69474, #29217, #57640, #12583, #40668, #34748, #29576, #24388, #68385, #40305, #57280, #35117, #52837, #52113, #2236, #24751, #1517, #19194, #46570, #64276, #13664, #32496, #3336, #59827, #64646, #70558, #14030, #9233, #36570, #36936, #15127, #42487, #43223, #48399, #65010, #8863, #8495, #19934, #9959, #4066, #37664, #31399, #31770, #25860, #65742, #2592, #60552, #19565, #42850, #70925, #53939, #15486, #20295, #59090, #31027, #53562, #26591, #37304, #54306, #25111, #54662, #2958, #42120, #48033, #47654, #3698, #14398, #20665, #60187, #25486, #65372, #59456, #70186, #66107, #14760, #32128, #49132, #26223, #48763, #9596, #71286, #71660, #21033, #43586, #38030, #33216, #11419, #5871, #44321, #21396, #66851, #44689, #22846, #55394, #55755, #21760, #22491, #43952, #4788, #27322, #67934, #11779, #49854, #72380, #11048, #10325, #28403, #33574, #50940, #67219, #17308, #49489, #50222, #50581, #72748, #27685, #55030, #39868, #16223, #66475, #39495, #62017, #62380, #45041, #67575, #39132, #22133, #5514, #16580, #61646, #56122, #4434, #337, #32859, #73109, #38398, #16940, #38774, #5149, #28053, #60923, #61294, #10686, #33936, #15852, #56479, #45398, #26962, #72020, #28762, #40221, #46486, #17660, #18387, #52028, #64187, #69025, #23211, #35752, #18025, #34295, #35030, #40954, #45764, #29133, #68300, #63469, #62743, #68661, #46852, #1070, #1795, #6961, #23579, #40582, #12136, #51666, #41665, #58273, #69392, #63101, #12856, #57558, #24305, #56827, #19110, #51301, #1430, #29491, #12502, #47210, #23937, #34661, #57190, #6603 ),
 ( #7680, #46124, #6233, #35389, #69742, #41311, #57912, #7321, #702, #29852, #52388, #18747, #63821, #13213, #30216, #52749, #2153, #24664, #3243, #31680, #26502, #9143, #2505, #54214, #20208, #32042, #14670, #53478, #25028, #43497, #3611, #58640, #47570, #13575, #64922, #14312, #59735, #54575, #37577, #70100, #8408, #30582, #19476, #25400, #26132, #64558, #70833, #31309, #48672, #71197, #42034, #13947, #42762, #2870, #36484, #20571, #25771, #42399, #43128, #65282, #59002, #30937, #47943, #8048, #65651, #70472, #3979, #15040, #53108, #60101, #49044, #37213, #19849, #36848, #59364, #8775, #53849, #48309, #9510, #71572, #20946, #36120, #38307, #44956, #72666, #61563, #27967, #15767, #15402, #67494, #16138, #32774, #60836, #5428, #61209, #22045, #38690, #27235, #44233, #49772, #33487, #49405, #37944, #10604, #71936, #33132, #66023, #55669, #10965, #4349, #43866, #67136, #56036, #5066, #66765, #22409, #32405, #50498, #26875, #27602, #50134, #21312, #4705, #73025, #55311, #16493, #44606, #72297, #21676, #66390, #10241, #60463, #16857, #9872, #39049, #54944, #9014, #26367, #15632, #43730, #2739, #26001, #59601, #37077, #71808, #54085, #70334, #64786, #36711, #9740, #20442, #37451, #66254, #37811, #59233, #25257, #31170, #58868, #42992, #48172, #3846, #71438, #8641, #31545, #42627, #8278, #49275, #3483, #15272, #32274, #70696, #47805, #20071, #48540, #26742, #53713, #71067, #25634, #48906, #19711, #3105, #65151, #21178, #30808, #14541, #65523, #14909, #14177, #54807, #59970, #4213, #9378, #53341, #42263, #31911, #54447, #20813, #43368, #65892, #60331, #70469, #42759, #8044, #19845, #65279, #48305, #35749, #19107, #41308, #13210, #36117, #42396, #2150, #8405, #42031, #64918, #59360, #58270, #7677, #30934, #13572, #30213, #8772, #36480, #53105, #31306, #53475, #52745, #24661, #47207, #69389, #53846, #69738, #14667, #14309, #63818, #36845, #37210, #2867, #18744, #41662, #64184, #58637, #30579, #2502, #70830, #3240, #25768, #25025, #47567, #58999, #54210, #31677, #70097, #19473, #25397, #64553, #47940, #13944, #24301, #20204, #59732, #9140, #46849, #33483, #4346, #60832, #65648, #71569, #15037, #10238, #37574, #37941, #16134, #43494, #44230, #49402, #66020, #9869, #9507, #20943, #10962, #5063, #38686, #32401, #32771, #26871, #66762, #3607, #61560, #20567, #43862, #71933, #54941, #16489, #21309, #60098, #32037, #54572, #27599, #38303, #55308, #26129, #55666, #3975, #43125, #49040, #22042, #26498, #4702, #72294, #27232, #66387, #15399, #21672, #50131, #71194, #72663, #60460, #48668, #15764, #39046, #10601, #49769, #61206, #33129, #44602, #67133, #28676, #28317, #17575, #253, #51216, #50854, #34209, #45679, #979, #68931, #51580, #44953, #23489, #62652, #1336, #57101, #22761, #67491, #12763, #46036, #27964, #16854, #29045, #23848, #39781, #68572, #46396, #6873, #39410, #45313, #73021, #61929, #67848, #17931, #33852, #40137, #616, #40494, #63010, #11334, #56396, #12049, #17220, #5786, #12406, #68214, #11693, #23124, #18289, #34941, #34573, #62297, #56033, #40862, #22406, #6510, #56743, #57467, #6146, #29405, #51939, #63379, #5425, #50495, #48212, #30846, #24208, #53380, #41934, #53752, #36393, #2061, #46761, #65191, #2776, #7230, #69295, #8317, #3149, #19012, #25299, #25675, #59272, #18658, #30120, #52296, #41220, #47117, #47846, #13119, #19377, #53017, #70374, #19752, #63728, #35660, #64460, #24572, #58180, #42301, #47476, #64091, #64827, #13851, #7585, #52654, #69649, #29759, #14217, #41573, #70734, #36752, #1697, #8680, #20112, #58907, #13473, #36022, #58539, #7951, #30489, #2411, #31212, #42667, #35299, #24932, #70007, #57820, #32682, #44140, #33042, #31949, #37114, #50042, #4256, #71478, #54485, #61118, #71847, #55221, #26781, #65931, #9779, #15311, #16044, #43032, #59641, #49313, #65561, #43771, #14581, #60370, #72209, #54123, #20479, #4616, #27146, #21218, #37849, #55582, #9053, #66295, #4975, #14950, #15675, #10150, #38212, #32313, #3886, #49680, #66667, #31584, #10515, #26040, #3519, #54847, #60740, #21586, #21954, #27509, #37488, #38592, #71106, #72568, #20854, #44511, #48579, #60009, #48949, #26406, #9419, #43406, #170, #28591, #23755, #1250, #61477, #72935, #6057, #50411, #51128, #11605, #67045, #525, #55942, #68478, #50765, #16405, #67758, #23036, #5338, #61838, #27878, #45591, #22317, #28235, #6420, #33766, #34485, #39691, #56310, #22674, #44870, #11243, #38959, #17840, #28952, #45225, #68125, #17130, #57015, #10872, #51847, #33405, #34122, #62209, #56662, #6784, #17490, #67406, #16767, #39325, #40401, #40052, #62564, #5699, #45947, #11960, #51491, #891, #57377, #23398, #62920, #12315, #34850, #29316, #69566, #30027, #3055, #36665, #24486, #2689, #70288, #35572, #12678, #58091, #35931, #14127, #46669, #47030, #13033, #13764, #35214, #69210, #18568, #59184, #46304, #41135, #63644, #2327, #1609, #19660, #24844, #42215, #58453, #8594, #40771, #41486, #41844, #64006, #18926, #68843, #58820, #13386, #7865, #30401, #53291, #31123, #36306, #8231, #52930, #47390, #69920, #19290, #30759, #57736, #52208, #64373, #25205, #47753, #64739, #53663, #18200, #63285, #7142, #24120, #29672, #7499, #52570, #1977, #42944, #43683, #4531, #20023, #72114, #37029, #25586, #20763, #61027, #32594, #4164, #9330, #48125, #38501, #42577, #71389, #71017, #60280, #65471, #43320, #20395, #3797, #15223, #66206, #10424, #21130, #14494, #15584, #32226, #44050, #26694, #14861, #59553, #55492, #38126, #70648, #8964, #71761, #66574, #31863, #60647, #15953, #49589, #31498, #37400, #65105, #54038, #59924, #10062, #3434, #9693, #65840, #55132, #27059, #25953, #48493, #54760, #54398, #26319, #21497, #37762, #48858, #32956, #49228, #38872, #61390, #66951, #49952, #62473, #33317, #23307, #45501, #21863 ) ),
 .UNSPECIFIED., .F., .F., .F. ) 
 B_SPLINE_SURFACE_WITH_KNOTS ( ( 2, 2 ),
 ( 3, 2, 2, 2, 2, 2, 2, 2, 2, 2, 2, 2, 2, 2, 2, 2, 2, 2, 2, 2, 2, 2, 2, 2, 2, 2, 2, 2, 2, 2, 2, 2, 2, 2, 2, 2, 2, 2, 2, 2, 2, 2, 2, 2, 2, 2, 2, 2, 2, 2, 2, 2, 2, 2, 2, 2, 2, 2, 2, 2, 2, 2, 2, 2, 2, 2, 2, 2, 2, 2, 2, 2, 2, 2, 2, 2, 2, 2, 2, 2, 2, 2, 2, 2, 2, 2, 2, 2, 2, 2, 2, 2, 2, 2, 2, 2, 2, 2, 2, 2, 2, 2, 2, 2, 2, 2, 2, 2, 2, 2, 2, 2, 2, 2, 2, 2, 2, 2, 2, 2, 2, 2, 2, 2, 2, 2, 2, 2, 2, 2, 2, 2, 2, 2, 2, 2, 2, 2, 2, 2, 2, 2, 2, 2, 2, 2, 2, 2, 2, 2, 2, 2, 2, 2, 2, 2, 2, 2, 2, 2, 2, 2, 2, 2, 2, 2, 2, 2, 2, 2, 2, 2, 2, 2, 2, 2, 2, 2, 2, 2, 2, 2, 2, 2, 2, 2, 2, 2, 2, 2, 2, 2, 2, 2, 2, 2, 2, 2, 2, 2, 2, 2, 2, 2, 2, 2, 2, 2, 2, 2, 2, 2, 2, 2, 2, 2, 2, 2, 2, 2, 2, 2, 2, 2, 2, 2, 2, 2, 2, 2, 2, 2, 2, 2, 2, 2, 2, 2, 2, 2, 2, 2, 2, 2, 2, 2, 2, 2, 2, 2, 2, 2, 2, 2, 2, 2, 2, 2, 2, 2, 2, 2, 2, 2, 2, 2, 2, 2, 2, 2, 2, 2, 2, 2, 2, 2, 2, 2, 2, 2, 2, 2, 2, 2, 2, 2, 2, 2, 2, 2, 2, 2, 2, 2, 2, 2, 2, 2, 2, 2, 2, 2, 2, 2, 2, 2, 2, 2, 2, 2, 2, 2, 2, 2, 2, 2, 2, 2, 2, 2, 2, 2, 2, 2, 2, 2, 2, 2, 2, 2, 2, 2, 2, 2, 2, 2, 2, 2, 2, 2, 2, 2, 2, 2, 2, 2, 2, 2, 2, 2, 2, 2, 2, 2, 2, 2, 2, 2, 2, 2, 3 ),
 ( 0.000000000000000000, 1.000000000000000000 ),
 ( 0.000000000000000000, 0.002777777777777777884, 0.005555555555555555768, 0.008333333333333333218, 0.01111111111111111154, 0.01388888888888888812, 0.01666666666666666644, 0.01944444444444444475, 0.02222222222222222307, 0.02500000000000000139, 0.02777777777777777624, 0.03055555555555555455, 0.03333333333333333287, 0.03611111111111110772, 0.03888888888888888951, 0.04166666666666666435, 0.04444444444444444614, 0.04722222222222222099, 0.05000000000000000278, 0.05277777777777777762, 0.05555555555555555247, 0.05833333333333333426, 0.06111111111111110911, 0.06388888888888888395, 0.06666666666666666574, 0.06944444444444444753, 0.07222222222222221544, 0.07499999999999999722, 0.07777777777777777901, 0.08055555555555556080, 0.08333333333333332871, 0.08611111111111111049, 0.08888888888888889228, 0.09166666666666666019, 0.09444444444444444198, 0.09722222222222222376, 0.1000000000000000056, 0.1027777777777777735, 0.1055555555555555552, 0.1083333333333333370, 0.1111111111111111049, 0.1138888888888888867, 0.1166666666666666685, 0.1194444444444444503, 0.1222222222222222182, 0.1250000000000000000, 0.1277777777777777679, 0.1305555555555555636, 0.1333333333333333315, 0.1361111111111110994, 0.1388888888888888951, 0.1416666666666666630, 0.1444444444444444309, 0.1472222222222222265, 0.1499999999999999944, 0.1527777777777777901, 0.1555555555555555580, 0.1583333333333333259, 0.1611111111111111216, 0.1638888888888888895, 0.1666666666666666574, 0.1694444444444444531, 0.1722222222222222210, 0.1749999999999999889, 0.1777777777777777846, 0.1805555555555555525, 0.1833333333333333204, 0.1861111111111111160, 0.1888888888888888840, 0.1916666666666666796, 0.1944444444444444475, 0.1972222222222222154, 0.2000000000000000111, 0.2027777777777777790, 0.2055555555555555469, 0.2083333333333333426, 0.2111111111111111105, 0.2138888888888888784, 0.2166666666666666741, 0.2194444444444444420, 0.2222222222222222099, 0.2250000000000000056, 0.2277777777777777735, 0.2305555555555555691, 0.2333333333333333370, 0.2361111111111111049, 0.2388888888888889006, 0.2416666666666666685, 0.2444444444444444364, 0.2472222222222222321, 0.2500000000000000000, 0.2527777777777777679, 0.2555555555555555358, 0.2583333333333333592, 0.2611111111111111271, 0.2638888888888888951, 0.2666666666666666630, 0.2694444444444444309, 0.2722222222222221988, 0.2750000000000000222, 0.2777777777777777901, 0.2805555555555555580, 0.2833333333333333259, 0.2861111111111110938, 0.2888888888888888618, 0.2916666666666666852, 0.2944444444444444531, 0.2972222222222222210, 0.2999999999999999889, 0.3027777777777777568, 0.3055555555555555802, 0.3083333333333333481, 0.3111111111111111160, 0.3138888888888888840, 0.3166666666666666519, 0.3194444444444444198, 0.3222222222222222432, 0.3250000000000000111, 0.3277777777777777790, 0.3305555555555555469, 0.3333333333333333148, 0.3361111111111111382, 0.3388888888888889062, 0.3416666666666666741, 0.3444444444444444420, 0.3472222222222222099, 0.3499999999999999778, 0.3527777777777778012, 0.3555555555555555691, 0.3583333333333333370, 0.3611111111111111049, 0.3638888888888888729, 0.3666666666666666408, 0.3694444444444444642, 0.3722222222222222321, 0.3750000000000000000, 0.3777777777777777679, 0.3805555555555555358, 0.3833333333333333592, 0.3861111111111111271, 0.3888888888888888951, 0.3916666666666666630, 0.3944444444444444309, 0.3972222222222221988, 0.4000000000000000222, 0.4027777777777777901, 0.4055555555555555580, 0.4083333333333333259, 0.4111111111111110938, 0.4138888888888888618, 0.4166666666666666852, 0.4194444444444444531, 0.4222222222222222210, 0.4249999999999999889, 0.4277777777777777568, 0.4305555555555555802, 0.4333333333333333481, 0.4361111111111111160, 0.4388888888888888840, 0.4416666666666666519, 0.4444444444444444198, 0.4472222222222222432, 0.4500000000000000111, 0.4527777777777777790, 0.4555555555555555469, 0.4583333333333333148, 0.4611111111111111382, 0.4638888888888889062, 0.4666666666666666741, 0.4694444444444444420, 0.4722222222222222099, 0.4749999999999999778, 0.4777777777777778012, 0.4805555555555555691, 0.4833333333333333370, 0.4861111111111111049, 0.4888888888888888729, 0.4916666666666666408, 0.4944444444444444642, 0.4972222222222222321, 0.5000000000000000000, 0.5027777777777777679, 0.5055555555555555358, 0.5083333333333333037, 0.5111111111111110716, 0.5138888888888888395, 0.5166666666666667185, 0.5194444444444444864, 0.5222222222222222543, 0.5250000000000000222, 0.5277777777777777901, 0.5305555555555555580, 0.5333333333333333259, 0.5361111111111110938, 0.5388888888888888618, 0.5416666666666666297, 0.5444444444444443976, 0.5472222222222222765, 0.5500000000000000444, 0.5527777777777778123, 0.5555555555555555802, 0.5583333333333333481, 0.5611111111111111160, 0.5638888888888888840, 0.5666666666666666519, 0.5694444444444444198, 0.5722222222222221877, 0.5749999999999999556, 0.5777777777777777235, 0.5805555555555556024, 0.5833333333333333703, 0.5861111111111111382, 0.5888888888888889062, 0.5916666666666666741, 0.5944444444444444420, 0.5972222222222222099, 0.5999999999999999778, 0.6027777777777777457, 0.6055555555555555136, 0.6083333333333332815, 0.6111111111111111605, 0.6138888888888889284, 0.6166666666666666963, 0.6194444444444444642, 0.6222222222222222321, 0.6250000000000000000, 0.6277777777777777679, 0.6305555555555555358, 0.6333333333333333037, 0.6361111111111110716, 0.6388888888888888395, 0.6416666666666667185, 0.6444444444444444864, 0.6472222222222222543, 0.6500000000000000222, 0.6527777777777777901, 0.6555555555555555580, 0.6583333333333333259, 0.6611111111111110938, 0.6638888888888888618, 0.6666666666666666297, 0.6694444444444443976, 0.6722222222222222765, 0.6750000000000000444, 0.6777777777777778123, 0.6805555555555555802, 0.6833333333333333481, 0.6861111111111111160, 0.6888888888888888840, 0.6916666666666666519, 0.6944444444444444198, 0.6972222222222221877, 0.6999999999999999556, 0.7027777777777777235, 0.7055555555555556024, 0.7083333333333333703, 0.7111111111111111382, 0.7138888888888889062, 0.7166666666666666741, 0.7194444444444444420, 0.7222222222222222099, 0.7249999999999999778, 0.7277777777777777457, 0.7305555555555555136, 0.7333333333333332815, 0.7361111111111111605, 0.7388888888888889284, 0.7416666666666666963, 0.7444444444444444642, 0.7472222222222222321, 0.7500000000000000000, 0.7527777777777777679, 0.7555555555555555358, 0.7583333333333333037, 0.7611111111111110716, 0.7638888888888888395, 0.7666666666666667185, 0.7694444444444444864, 0.7722222222222222543, 0.7750000000000000222, 0.7777777777777777901, 0.7805555555555555580, 0.7833333333333333259, 0.7861111111111110938, 0.7888888888888888618, 0.7916666666666666297, 0.7944444444444443976, 0.7972222222222222765, 0.8000000000000000444, 0.8027777777777778123, 0.8055555555555555802, 0.8083333333333333481, 0.8111111111111111160, 0.8138888888888888840, 0.8166666666666666519, 0.8194444444444444198, 0.8222222222222221877, 0.8249999999999999556, 0.8277777777777777235, 0.8305555555555556024, 0.8333333333333333703, 0.8361111111111111382, 0.8388888888888889062, 0.8416666666666666741, 0.8444444444444444420, 0.8472222222222222099, 0.8499999999999999778, 0.8527777777777777457, 0.8555555555555555136, 0.8583333333333332815, 0.8611111111111111605, 0.8638888888888889284, 0.8666666666666666963, 0.8694444444444444642, 0.8722222222222222321, 0.8750000000000000000, 0.8777777777777777679, 0.8805555555555555358, 0.8833333333333333037, 0.8861111111111110716, 0.8888888888888888395, 0.8916666666666667185, 0.8944444444444444864, 0.8972222222222222543, 0.9000000000000000222, 0.9027777777777777901, 0.9055555555555555580, 0.9083333333333333259, 0.9111111111111110938, 0.9138888888888888618, 0.9166666666666666297, 0.9194444444444443976, 0.9222222222222222765, 0.9250000000000000444, 0.9277777777777778123, 0.9305555555555555802, 0.9333333333333333481, 0.9361111111111111160, 0.9388888888888888840, 0.9416666666666666519, 0.9444444444444444198, 0.9472222222222221877, 0.9499999999999999556, 0.9527777777777777235, 0.9555555555555556024, 0.9583333333333333703, 0.9611111111111111382, 0.9638888888888889062, 0.9666666666666666741, 0.9694444444444444420, 0.9722222222222222099, 0.9749999999999999778, 0.9777777777777777457, 0.9805555555555555136, 0.9833333333333332815, 0.9861111111111111605, 0.9888888888888889284, 0.9916666666666666963, 0.9944444444444444642, 0.9972222222222222321, 1.000000000000000000 ),
 .UNSPECIFIED. ) 
 GEOMETRIC_REPRESENTATION_ITEM ( )  RATIONAL_B_SPLINE_SURFACE ( (
 ( 1.000000000000000000, 0.8660254037844387076, 1.000000000000000000, 0.8660254037844387076, 1.000000000000000000, 0.8660254037844387076, 1.000000000000000000, 0.8660254037844387076, 1.000000000000000000, 0.8660254037844387076, 1.000000000000000000, 0.8660254037844387076, 1.000000000000000000, 0.8660254037844387076, 1.000000000000000000, 0.8660254037844387076, 1.000000000000000000, 0.8660254037844387076, 1.000000000000000000, 0.8660254037844387076, 1.000000000000000000, 0.8660254037844387076, 1.000000000000000000, 0.8660254037844387076, 1.000000000000000000, 0.8660254037844387076, 1.000000000000000000, 0.8660254037844387076, 1.000000000000000000, 0.8660254037844387076, 1.000000000000000000, 0.8660254037844387076, 1.000000000000000000, 0.8660254037844387076, 1.000000000000000000, 0.8660254037844387076, 1.000000000000000000, 0.8660254037844387076, 1.000000000000000000, 0.8660254037844387076, 1.000000000000000000, 0.8660254037844387076, 1.000000000000000000, 0.8660254037844387076, 1.000000000000000000, 0.8660254037844387076, 1.000000000000000000, 0.8660254037844387076, 1.000000000000000000, 0.8660254037844387076, 1.000000000000000000, 0.8660254037844387076, 1.000000000000000000, 0.8660254037844387076, 1.000000000000000000, 0.8660254037844387076, 1.000000000000000000, 0.8660254037844387076, 1.000000000000000000, 0.8660254037844387076, 1.000000000000000000, 0.8660254037844387076, 1.000000000000000000, 0.8660254037844387076, 1.000000000000000000, 0.8660254037844387076, 1.000000000000000000, 0.8660254037844387076, 1.000000000000000000, 0.8660254037844387076, 1.000000000000000000, 0.8660254037844387076, 1.000000000000000000, 0.8660254037844387076, 1.000000000000000000, 0.8660254037844387076, 1.000000000000000000, 0.8660254037844387076, 1.000000000000000000, 0.8660254037844387076, 1.000000000000000000, 0.8660254037844387076, 1.000000000000000000, 0.8660254037844387076, 1.000000000000000000, 0.8660254037844387076, 1.000000000000000000, 0.8660254037844387076, 1.000000000000000000, 0.8660254037844387076, 1.000000000000000000, 0.8660254037844387076, 1.000000000000000000, 0.8660254037844387076, 1.000000000000000000, 0.8660254037844387076, 1.000000000000000000, 0.8660254037844387076, 1.000000000000000000, 0.8660254037844387076, 1.000000000000000000, 0.8660254037844387076, 1.000000000000000000, 0.8660254037844387076, 1.000000000000000000, 0.8660254037844387076, 1.000000000000000000, 0.8660254037844387076, 1.000000000000000000, 0.8660254037844387076, 1.000000000000000000, 0.8660254037844387076, 1.000000000000000000, 0.8660254037844387076, 1.000000000000000000, 0.8660254037844387076, 1.000000000000000000, 0.8660254037844387076, 1.000000000000000000, 0.8660254037844387076, 1.000000000000000000, 0.8660254037844387076, 1.000000000000000000, 0.8660254037844387076, 1.000000000000000000, 0.8660254037844387076, 1.000000000000000000, 0.8660254037844387076, 1.000000000000000000, 0.8660254037844387076, 1.000000000000000000, 0.8660254037844387076, 1.000000000000000000, 0.8660254037844387076, 1.000000000000000000, 0.8660254037844387076, 1.000000000000000000, 0.8660254037844387076, 1.000000000000000000, 0.8660254037844387076, 1.000000000000000000, 0.8660254037844387076, 1.000000000000000000, 0.8660254037844387076, 1.000000000000000000, 0.8660254037844387076, 1.000000000000000000, 0.8660254037844387076, 1.000000000000000000, 0.8660254037844387076, 1.000000000000000000, 0.8660254037844387076, 1.000000000000000000, 0.8660254037844387076, 1.000000000000000000, 0.8660254037844387076, 1.000000000000000000, 0.8660254037844387076, 1.000000000000000000, 0.8660254037844387076, 1.000000000000000000, 0.8660254037844387076, 1.000000000000000000, 0.8660254037844387076, 1.000000000000000000, 0.8660254037844387076, 1.000000000000000000, 0.8660254037844387076, 1.000000000000000000, 0.8660254037844387076, 1.000000000000000000, 0.8660254037844387076, 1.000000000000000000, 0.8660254037844387076, 1.000000000000000000, 0.8660254037844387076, 1.000000000000000000, 0.8660254037844387076, 1.000000000000000000, 0.8660254037844387076, 1.000000000000000000, 0.8660254037844387076, 1.000000000000000000, 0.8660254037844387076, 1.000000000000000000, 0.8660254037844387076, 1.000000000000000000, 0.8660254037844387076, 1.000000000000000000, 0.8660254037844387076, 1.000000000000000000, 0.8660254037844387076, 1.000000000000000000, 0.8660254037844387076, 1.000000000000000000, 0.8660254037844387076, 1.000000000000000000, 0.8660254037844387076, 1.000000000000000000, 0.8660254037844387076, 1.000000000000000000, 0.8660254037844387076, 1.000000000000000000, 0.8660254037844387076, 1.000000000000000000, 0.8660254037844387076, 1.000000000000000000, 0.8660254037844387076, 1.000000000000000000, 0.8660254037844387076, 1.000000000000000000, 0.8660254037844387076, 1.000000000000000000, 0.8660254037844387076, 1.000000000000000000, 0.8660254037844387076, 1.000000000000000000, 0.8660254037844387076, 1.000000000000000000, 0.8660254037844387076, 1.000000000000000000, 0.8660254037844387076, 1.000000000000000000, 0.8660254037844387076, 1.000000000000000000, 0.8660254037844387076, 1.000000000000000000, 0.8660254037844387076, 1.000000000000000000, 0.8660254037844387076, 1.000000000000000000, 0.8660254037844387076, 1.000000000000000000, 0.8660254037844387076, 1.000000000000000000, 0.8660254037844387076, 1.000000000000000000, 0.8660254037844387076, 1.000000000000000000, 0.8660254037844387076, 1.000000000000000000, 0.8660254037844387076, 1.000000000000000000, 0.8660254037844387076, 1.000000000000000000, 0.8660254037844387076, 1.000000000000000000, 0.8660254037844387076, 1.000000000000000000, 0.8660254037844387076, 1.000000000000000000, 0.8660254037844387076, 1.000000000000000000, 0.8660254037844387076, 1.000000000000000000, 0.8660254037844387076, 1.000000000000000000, 0.8660254037844387076, 1.000000000000000000, 0.8660254037844387076, 1.000000000000000000, 0.8660254037844387076, 1.000000000000000000, 0.8660254037844387076, 1.000000000000000000, 0.8660254037844387076, 1.000000000000000000, 0.8660254037844387076, 1.000000000000000000, 0.8660254037844387076, 1.000000000000000000, 0.8660254037844387076, 1.000000000000000000, 0.8660254037844387076, 1.000000000000000000, 0.8660254037844387076, 1.000000000000000000, 0.8660254037844387076, 1.000000000000000000, 0.8660254037844387076, 1.000000000000000000, 0.8660254037844387076, 1.000000000000000000, 0.8660254037844387076, 1.000000000000000000, 0.8660254037844387076, 1.000000000000000000, 0.8660254037844387076, 1.000000000000000000, 0.8660254037844387076, 1.000000000000000000, 0.8660254037844387076, 1.000000000000000000, 0.8660254037844387076, 1.000000000000000000, 0.8660254037844387076, 1.000000000000000000, 0.8660254037844387076, 1.000000000000000000, 0.8660254037844387076, 1.000000000000000000, 0.8660254037844387076, 1.000000000000000000, 0.8660254037844387076, 1.000000000000000000, 0.8660254037844387076, 1.000000000000000000, 0.8660254037844387076, 1.000000000000000000, 0.8660254037844387076, 1.000000000000000000, 0.8660254037844387076, 1.000000000000000000, 0.8660254037844387076, 1.000000000000000000, 0.8660254037844387076, 1.000000000000000000, 0.8660254037844387076, 1.000000000000000000, 0.8660254037844387076, 1.000000000000000000, 0.8660254037844387076, 1.000000000000000000, 0.8660254037844387076, 1.000000000000000000, 0.8660254037844387076, 1.000000000000000000, 0.8660254037844387076, 1.000000000000000000, 0.8660254037844387076, 1.000000000000000000, 0.8660254037844387076, 1.000000000000000000, 0.8660254037844387076, 1.000000000000000000, 0.8660254037844387076, 1.000000000000000000, 0.8660254037844387076, 1.000000000000000000, 0.8660254037844387076, 1.000000000000000000, 0.8660254037844387076, 1.000000000000000000, 0.8660254037844387076, 1.000000000000000000, 0.8660254037844387076, 1.000000000000000000, 0.8660254037844387076, 1.000000000000000000, 0.8660254037844387076, 1.000000000000000000, 0.8660254037844387076, 1.000000000000000000, 0.8660254037844387076, 1.000000000000000000, 0.8660254037844387076, 1.000000000000000000, 0.8660254037844387076, 1.000000000000000000, 0.8660254037844387076, 1.000000000000000000, 0.8660254037844387076, 1.000000000000000000, 0.8660254037844387076, 1.000000000000000000, 0.8660254037844387076, 1.000000000000000000, 0.8660254037844387076, 1.000000000000000000, 0.8660254037844387076, 1.000000000000000000, 0.8660254037844387076, 1.000000000000000000, 0.8660254037844387076, 1.000000000000000000, 0.8660254037844387076, 1.000000000000000000, 0.8660254037844387076, 1.000000000000000000, 0.8660254037844387076, 1.000000000000000000, 0.8660254037844387076, 1.000000000000000000, 0.8660254037844387076, 1.000000000000000000, 0.8660254037844387076, 1.000000000000000000, 0.8660254037844387076, 1.000000000000000000, 0.8660254037844387076, 1.000000000000000000, 0.8660254037844387076, 1.000000000000000000, 0.8660254037844387076, 1.000000000000000000, 0.8660254037844387076, 1.000000000000000000, 0.8660254037844387076, 1.000000000000000000, 0.8660254037844387076, 1.000000000000000000, 0.8660254037844387076, 1.000000000000000000, 0.8660254037844387076, 1.000000000000000000, 0.8660254037844387076, 1.000000000000000000, 0.8660254037844387076, 1.000000000000000000, 0.8660254037844387076, 1.000000000000000000, 0.8660254037844387076, 1.000000000000000000, 0.8660254037844387076, 1.000000000000000000, 0.8660254037844387076, 1.000000000000000000, 0.8660254037844387076, 1.000000000000000000, 0.8660254037844387076, 1.000000000000000000, 0.8660254037844387076, 1.000000000000000000, 0.8660254037844387076, 1.000000000000000000, 0.8660254037844387076, 1.000000000000000000, 0.8660254037844387076, 1.000000000000000000, 0.8660254037844387076, 1.000000000000000000, 0.8660254037844387076, 1.000000000000000000, 0.8660254037844387076, 1.000000000000000000, 0.8660254037844387076, 1.000000000000000000, 0.8660254037844387076, 1.000000000000000000, 0.8660254037844387076, 1.000000000000000000, 0.8660254037844387076, 1.000000000000000000, 0.8660254037844387076, 1.000000000000000000, 0.8660254037844387076, 1.000000000000000000, 0.8660254037844387076, 1.000000000000000000, 0.8660254037844387076, 1.000000000000000000, 0.8660254037844387076, 1.000000000000000000, 0.8660254037844387076, 1.000000000000000000, 0.8660254037844387076, 1.000000000000000000, 0.8660254037844387076, 1.000000000000000000, 0.8660254037844387076, 1.000000000000000000, 0.8660254037844387076, 1.000000000000000000, 0.8660254037844387076, 1.000000000000000000, 0.8660254037844387076, 1.000000000000000000, 0.8660254037844387076, 1.000000000000000000, 0.8660254037844387076, 1.000000000000000000, 0.8660254037844387076, 1.000000000000000000, 0.8660254037844387076, 1.000000000000000000, 0.8660254037844387076, 1.000000000000000000, 0.8660254037844387076, 1.000000000000000000, 0.8660254037844387076, 1.000000000000000000, 0.8660254037844387076, 1.000000000000000000, 0.8660254037844387076, 1.000000000000000000, 0.8660254037844387076, 1.000000000000000000, 0.8660254037844387076, 1.000000000000000000, 0.8660254037844387076, 1.000000000000000000, 0.8660254037844387076, 1.000000000000000000, 0.8660254037844387076, 1.000000000000000000, 0.8660254037844387076, 1.000000000000000000, 0.8660254037844387076, 1.000000000000000000, 0.8660254037844387076, 1.000000000000000000, 0.8660254037844387076, 1.000000000000000000, 0.8660254037844387076, 1.000000000000000000, 0.8660254037844387076, 1.000000000000000000, 0.8660254037844387076, 1.000000000000000000, 0.8660254037844387076, 1.000000000000000000, 0.8660254037844387076, 1.000000000000000000, 0.8660254037844387076, 1.000000000000000000, 0.8660254037844387076, 1.000000000000000000, 0.8660254037844387076, 1.000000000000000000, 0.8660254037844387076, 1.000000000000000000, 0.8660254037844387076, 1.000000000000000000, 0.8660254037844387076, 1.000000000000000000, 0.8660254037844387076, 1.000000000000000000, 0.8660254037844387076, 1.000000000000000000, 0.8660254037844387076, 1.000000000000000000, 0.8660254037844387076, 1.000000000000000000, 0.8660254037844387076, 1.000000000000000000, 0.8660254037844387076, 1.000000000000000000, 0.8660254037844387076, 1.000000000000000000, 0.8660254037844387076, 1.000000000000000000, 0.8660254037844387076, 1.000000000000000000, 0.8660254037844387076, 1.000000000000000000, 0.8660254037844387076, 1.000000000000000000, 0.8660254037844387076, 1.000000000000000000, 0.8660254037844387076, 1.000000000000000000, 0.8660254037844387076, 1.000000000000000000, 0.8660254037844387076, 1.000000000000000000, 0.8660254037844387076, 1.000000000000000000, 0.8660254037844387076, 1.000000000000000000, 0.8660254037844387076, 1.000000000000000000, 0.8660254037844387076, 1.000000000000000000, 0.8660254037844387076, 1.000000000000000000, 0.8660254037844387076, 1.000000000000000000, 0.8660254037844387076, 1.000000000000000000, 0.8660254037844387076, 1.000000000000000000, 0.8660254037844387076, 1.000000000000000000, 0.8660254037844387076, 1.000000000000000000, 0.8660254037844387076, 1.000000000000000000, 0.8660254037844387076, 1.000000000000000000, 0.8660254037844387076, 1.000000000000000000, 0.8660254037844387076, 1.000000000000000000, 0.8660254037844387076, 1.000000000000000000, 0.8660254037844387076, 1.000000000000000000, 0.8660254037844387076, 1.000000000000000000, 0.8660254037844387076, 1.000000000000000000, 0.8660254037844387076, 1.000000000000000000, 0.8660254037844387076, 1.000000000000000000, 0.8660254037844387076, 1.000000000000000000, 0.8660254037844387076, 1.000000000000000000, 0.8660254037844387076, 1.000000000000000000, 0.8660254037844387076, 1.000000000000000000, 0.8660254037844387076, 1.000000000000000000, 0.8660254037844387076, 1.000000000000000000, 0.8660254037844387076, 1.000000000000000000, 0.8660254037844387076, 1.000000000000000000, 0.8660254037844387076, 1.000000000000000000, 0.8660254037844387076, 1.000000000000000000, 0.8660254037844387076, 1.000000000000000000, 0.8660254037844387076, 1.000000000000000000, 0.8660254037844387076, 1.000000000000000000, 0.8660254037844387076, 1.000000000000000000, 0.8660254037844387076, 1.000000000000000000, 0.8660254037844387076, 1.000000000000000000, 0.8660254037844387076, 1.000000000000000000, 0.8660254037844387076, 1.000000000000000000, 0.8660254037844387076, 1.000000000000000000, 0.8660254037844387076, 1.000000000000000000, 0.8660254037844387076, 1.000000000000000000, 0.8660254037844387076, 1.000000000000000000, 0.8660254037844387076, 1.000000000000000000, 0.8660254037844387076, 1.000000000000000000, 0.8660254037844387076, 1.000000000000000000, 0.8660254037844387076, 1.000000000000000000, 0.8660254037844387076, 1.000000000000000000, 0.8660254037844387076, 1.000000000000000000, 0.8660254037844387076, 1.000000000000000000, 0.8660254037844387076, 1.000000000000000000, 0.8660254037844387076, 1.000000000000000000, 0.8660254037844387076, 1.000000000000000000, 0.8660254037844387076, 1.000000000000000000, 0.8660254037844387076, 1.000000000000000000, 0.8660254037844387076, 1.000000000000000000, 0.8660254037844387076, 1.000000000000000000, 0.8660254037844387076, 1.000000000000000000, 0.8660254037844387076, 1.000000000000000000, 0.8660254037844387076, 1.000000000000000000, 0.8660254037844387076, 1.000000000000000000, 0.8660254037844387076, 1.000000000000000000, 0.8660254037844387076, 1.000000000000000000, 0.8660254037844387076, 1.000000000000000000, 0.8660254037844387076, 1.000000000000000000, 0.8660254037844387076, 1.000000000000000000, 0.8660254037844387076, 1.000000000000000000, 0.8660254037844387076, 1.000000000000000000, 0.8660254037844387076, 1.000000000000000000, 0.8660254037844387076, 1.000000000000000000, 0.8660254037844387076, 1.000000000000000000, 0.8660254037844387076, 1.000000000000000000, 0.8660254037844387076, 1.000000000000000000, 0.8660254037844387076, 1.000000000000000000, 0.8660254037844387076, 1.000000000000000000, 0.8660254037844387076, 1.000000000000000000, 0.8660254037844387076, 1.000000000000000000, 0.8660254037844387076, 1.000000000000000000, 0.8660254037844387076, 1.000000000000000000, 0.8660254037844387076, 1.000000000000000000, 0.8660254037844387076, 1.000000000000000000, 0.8660254037844387076, 1.000000000000000000, 0.8660254037844387076, 1.000000000000000000, 0.8660254037844387076, 1.000000000000000000),
 ( 1.000000000000000000, 0.8660254037844387076, 1.000000000000000000, 0.8660254037844387076, 1.000000000000000000, 0.8660254037844387076, 1.000000000000000000, 0.8660254037844387076, 1.000000000000000000, 0.8660254037844387076, 1.000000000000000000, 0.8660254037844387076, 1.000000000000000000, 0.8660254037844387076, 1.000000000000000000, 0.8660254037844387076, 1.000000000000000000, 0.8660254037844387076, 1.000000000000000000, 0.8660254037844387076, 1.000000000000000000, 0.8660254037844387076, 1.000000000000000000, 0.8660254037844387076, 1.000000000000000000, 0.8660254037844387076, 1.000000000000000000, 0.8660254037844387076, 1.000000000000000000, 0.8660254037844387076, 1.000000000000000000, 0.8660254037844387076, 1.000000000000000000, 0.8660254037844387076, 1.000000000000000000, 0.8660254037844387076, 1.000000000000000000, 0.8660254037844387076, 1.000000000000000000, 0.8660254037844387076, 1.000000000000000000, 0.8660254037844387076, 1.000000000000000000, 0.8660254037844387076, 1.000000000000000000, 0.8660254037844387076, 1.000000000000000000, 0.8660254037844387076, 1.000000000000000000, 0.8660254037844387076, 1.000000000000000000, 0.8660254037844387076, 1.000000000000000000, 0.8660254037844387076, 1.000000000000000000, 0.8660254037844387076, 1.000000000000000000, 0.8660254037844387076, 1.000000000000000000, 0.8660254037844387076, 1.000000000000000000, 0.8660254037844387076, 1.000000000000000000, 0.8660254037844387076, 1.000000000000000000, 0.8660254037844387076, 1.000000000000000000, 0.8660254037844387076, 1.000000000000000000, 0.8660254037844387076, 1.000000000000000000, 0.8660254037844387076, 1.000000000000000000, 0.8660254037844387076, 1.000000000000000000, 0.8660254037844387076, 1.000000000000000000, 0.8660254037844387076, 1.000000000000000000, 0.8660254037844387076, 1.000000000000000000, 0.8660254037844387076, 1.000000000000000000, 0.8660254037844387076, 1.000000000000000000, 0.8660254037844387076, 1.000000000000000000, 0.8660254037844387076, 1.000000000000000000, 0.8660254037844387076, 1.000000000000000000, 0.8660254037844387076, 1.000000000000000000, 0.8660254037844387076, 1.000000000000000000, 0.8660254037844387076, 1.000000000000000000, 0.8660254037844387076, 1.000000000000000000, 0.8660254037844387076, 1.000000000000000000, 0.8660254037844387076, 1.000000000000000000, 0.8660254037844387076, 1.000000000000000000, 0.8660254037844387076, 1.000000000000000000, 0.8660254037844387076, 1.000000000000000000, 0.8660254037844387076, 1.000000000000000000, 0.8660254037844387076, 1.000000000000000000, 0.8660254037844387076, 1.000000000000000000, 0.8660254037844387076, 1.000000000000000000, 0.8660254037844387076, 1.000000000000000000, 0.8660254037844387076, 1.000000000000000000, 0.8660254037844387076, 1.000000000000000000, 0.8660254037844387076, 1.000000000000000000, 0.8660254037844387076, 1.000000000000000000, 0.8660254037844387076, 1.000000000000000000, 0.8660254037844387076, 1.000000000000000000, 0.8660254037844387076, 1.000000000000000000, 0.8660254037844387076, 1.000000000000000000, 0.8660254037844387076, 1.000000000000000000, 0.8660254037844387076, 1.000000000000000000, 0.8660254037844387076, 1.000000000000000000, 0.8660254037844387076, 1.000000000000000000, 0.8660254037844387076, 1.000000000000000000, 0.8660254037844387076, 1.000000000000000000, 0.8660254037844387076, 1.000000000000000000, 0.8660254037844387076, 1.000000000000000000, 0.8660254037844387076, 1.000000000000000000, 0.8660254037844387076, 1.000000000000000000, 0.8660254037844387076, 1.000000000000000000, 0.8660254037844387076, 1.000000000000000000, 0.8660254037844387076, 1.000000000000000000, 0.8660254037844387076, 1.000000000000000000, 0.8660254037844387076, 1.000000000000000000, 0.8660254037844387076, 1.000000000000000000, 0.8660254037844387076, 1.000000000000000000, 0.8660254037844387076, 1.000000000000000000, 0.8660254037844387076, 1.000000000000000000, 0.8660254037844387076, 1.000000000000000000, 0.8660254037844387076, 1.000000000000000000, 0.8660254037844387076, 1.000000000000000000, 0.8660254037844387076, 1.000000000000000000, 0.8660254037844387076, 1.000000000000000000, 0.8660254037844387076, 1.000000000000000000, 0.8660254037844387076, 1.000000000000000000, 0.8660254037844387076, 1.000000000000000000, 0.8660254037844387076, 1.000000000000000000, 0.8660254037844387076, 1.000000000000000000, 0.8660254037844387076, 1.000000000000000000, 0.8660254037844387076, 1.000000000000000000, 0.8660254037844387076, 1.000000000000000000, 0.8660254037844387076, 1.000000000000000000, 0.8660254037844387076, 1.000000000000000000, 0.8660254037844387076, 1.000000000000000000, 0.8660254037844387076, 1.000000000000000000, 0.8660254037844387076, 1.000000000000000000, 0.8660254037844387076, 1.000000000000000000, 0.8660254037844387076, 1.000000000000000000, 0.8660254037844387076, 1.000000000000000000, 0.8660254037844387076, 1.000000000000000000, 0.8660254037844387076, 1.000000000000000000, 0.8660254037844387076, 1.000000000000000000, 0.8660254037844387076, 1.000000000000000000, 0.8660254037844387076, 1.000000000000000000, 0.8660254037844387076, 1.000000000000000000, 0.8660254037844387076, 1.000000000000000000, 0.8660254037844387076, 1.000000000000000000, 0.8660254037844387076, 1.000000000000000000, 0.8660254037844387076, 1.000000000000000000, 0.8660254037844387076, 1.000000000000000000, 0.8660254037844387076, 1.000000000000000000, 0.8660254037844387076, 1.000000000000000000, 0.8660254037844387076, 1.000000000000000000, 0.8660254037844387076, 1.000000000000000000, 0.8660254037844387076, 1.000000000000000000, 0.8660254037844387076, 1.000000000000000000, 0.8660254037844387076, 1.000000000000000000, 0.8660254037844387076, 1.000000000000000000, 0.8660254037844387076, 1.000000000000000000, 0.8660254037844387076, 1.000000000000000000, 0.8660254037844387076, 1.000000000000000000, 0.8660254037844387076, 1.000000000000000000, 0.8660254037844387076, 1.000000000000000000, 0.8660254037844387076, 1.000000000000000000, 0.8660254037844387076, 1.000000000000000000, 0.8660254037844387076, 1.000000000000000000, 0.8660254037844387076, 1.000000000000000000, 0.8660254037844387076, 1.000000000000000000, 0.8660254037844387076, 1.000000000000000000, 0.8660254037844387076, 1.000000000000000000, 0.8660254037844387076, 1.000000000000000000, 0.8660254037844387076, 1.000000000000000000, 0.8660254037844387076, 1.000000000000000000, 0.8660254037844387076, 1.000000000000000000, 0.8660254037844387076, 1.000000000000000000, 0.8660254037844387076, 1.000000000000000000, 0.8660254037844387076, 1.000000000000000000, 0.8660254037844387076, 1.000000000000000000, 0.8660254037844387076, 1.000000000000000000, 0.8660254037844387076, 1.000000000000000000, 0.8660254037844387076, 1.000000000000000000, 0.8660254037844387076, 1.000000000000000000, 0.8660254037844387076, 1.000000000000000000, 0.8660254037844387076, 1.000000000000000000, 0.8660254037844387076, 1.000000000000000000, 0.8660254037844387076, 1.000000000000000000, 0.8660254037844387076, 1.000000000000000000, 0.8660254037844387076, 1.000000000000000000, 0.8660254037844387076, 1.000000000000000000, 0.8660254037844387076, 1.000000000000000000, 0.8660254037844387076, 1.000000000000000000, 0.8660254037844387076, 1.000000000000000000, 0.8660254037844387076, 1.000000000000000000, 0.8660254037844387076, 1.000000000000000000, 0.8660254037844387076, 1.000000000000000000, 0.8660254037844387076, 1.000000000000000000, 0.8660254037844387076, 1.000000000000000000, 0.8660254037844387076, 1.000000000000000000, 0.8660254037844387076, 1.000000000000000000, 0.8660254037844387076, 1.000000000000000000, 0.8660254037844387076, 1.000000000000000000, 0.8660254037844387076, 1.000000000000000000, 0.8660254037844387076, 1.000000000000000000, 0.8660254037844387076, 1.000000000000000000, 0.8660254037844387076, 1.000000000000000000, 0.8660254037844387076, 1.000000000000000000, 0.8660254037844387076, 1.000000000000000000, 0.8660254037844387076, 1.000000000000000000, 0.8660254037844387076, 1.000000000000000000, 0.8660254037844387076, 1.000000000000000000, 0.8660254037844387076, 1.000000000000000000, 0.8660254037844387076, 1.000000000000000000, 0.8660254037844387076, 1.000000000000000000, 0.8660254037844387076, 1.000000000000000000, 0.8660254037844387076, 1.000000000000000000, 0.8660254037844387076, 1.000000000000000000, 0.8660254037844387076, 1.000000000000000000, 0.8660254037844387076, 1.000000000000000000, 0.8660254037844387076, 1.000000000000000000, 0.8660254037844387076, 1.000000000000000000, 0.8660254037844387076, 1.000000000000000000, 0.8660254037844387076, 1.000000000000000000, 0.8660254037844387076, 1.000000000000000000, 0.8660254037844387076, 1.000000000000000000, 0.8660254037844387076, 1.000000000000000000, 0.8660254037844387076, 1.000000000000000000, 0.8660254037844387076, 1.000000000000000000, 0.8660254037844387076, 1.000000000000000000, 0.8660254037844387076, 1.000000000000000000, 0.8660254037844387076, 1.000000000000000000, 0.8660254037844387076, 1.000000000000000000, 0.8660254037844387076, 1.000000000000000000, 0.8660254037844387076, 1.000000000000000000, 0.8660254037844387076, 1.000000000000000000, 0.8660254037844387076, 1.000000000000000000, 0.8660254037844387076, 1.000000000000000000, 0.8660254037844387076, 1.000000000000000000, 0.8660254037844387076, 1.000000000000000000, 0.8660254037844387076, 1.000000000000000000, 0.8660254037844387076, 1.000000000000000000, 0.8660254037844387076, 1.000000000000000000, 0.8660254037844387076, 1.000000000000000000, 0.8660254037844387076, 1.000000000000000000, 0.8660254037844387076, 1.000000000000000000, 0.8660254037844387076, 1.000000000000000000, 0.8660254037844387076, 1.000000000000000000, 0.8660254037844387076, 1.000000000000000000, 0.8660254037844387076, 1.000000000000000000, 0.8660254037844387076, 1.000000000000000000, 0.8660254037844387076, 1.000000000000000000, 0.8660254037844387076, 1.000000000000000000, 0.8660254037844387076, 1.000000000000000000, 0.8660254037844387076, 1.000000000000000000, 0.8660254037844387076, 1.000000000000000000, 0.8660254037844387076, 1.000000000000000000, 0.8660254037844387076, 1.000000000000000000, 0.8660254037844387076, 1.000000000000000000, 0.8660254037844387076, 1.000000000000000000, 0.8660254037844387076, 1.000000000000000000, 0.8660254037844387076, 1.000000000000000000, 0.8660254037844387076, 1.000000000000000000, 0.8660254037844387076, 1.000000000000000000, 0.8660254037844387076, 1.000000000000000000, 0.8660254037844387076, 1.000000000000000000, 0.8660254037844387076, 1.000000000000000000, 0.8660254037844387076, 1.000000000000000000, 0.8660254037844387076, 1.000000000000000000, 0.8660254037844387076, 1.000000000000000000, 0.8660254037844387076, 1.000000000000000000, 0.8660254037844387076, 1.000000000000000000, 0.8660254037844387076, 1.000000000000000000, 0.8660254037844387076, 1.000000000000000000, 0.8660254037844387076, 1.000000000000000000, 0.8660254037844387076, 1.000000000000000000, 0.8660254037844387076, 1.000000000000000000, 0.8660254037844387076, 1.000000000000000000, 0.8660254037844387076, 1.000000000000000000, 0.8660254037844387076, 1.000000000000000000, 0.8660254037844387076, 1.000000000000000000, 0.8660254037844387076, 1.000000000000000000, 0.8660254037844387076, 1.000000000000000000, 0.8660254037844387076, 1.000000000000000000, 0.8660254037844387076, 1.000000000000000000, 0.8660254037844387076, 1.000000000000000000, 0.8660254037844387076, 1.000000000000000000, 0.8660254037844387076, 1.000000000000000000, 0.8660254037844387076, 1.000000000000000000, 0.8660254037844387076, 1.000000000000000000, 0.8660254037844387076, 1.000000000000000000, 0.8660254037844387076, 1.000000000000000000, 0.8660254037844387076, 1.000000000000000000, 0.8660254037844387076, 1.000000000000000000, 0.8660254037844387076, 1.000000000000000000, 0.8660254037844387076, 1.000000000000000000, 0.8660254037844387076, 1.000000000000000000, 0.8660254037844387076, 1.000000000000000000, 0.8660254037844387076, 1.000000000000000000, 0.8660254037844387076, 1.000000000000000000, 0.8660254037844387076, 1.000000000000000000, 0.8660254037844387076, 1.000000000000000000, 0.8660254037844387076, 1.000000000000000000, 0.8660254037844387076, 1.000000000000000000, 0.8660254037844387076, 1.000000000000000000, 0.8660254037844387076, 1.000000000000000000, 0.8660254037844387076, 1.000000000000000000, 0.8660254037844387076, 1.000000000000000000, 0.8660254037844387076, 1.000000000000000000, 0.8660254037844387076, 1.000000000000000000, 0.8660254037844387076, 1.000000000000000000, 0.8660254037844387076, 1.000000000000000000, 0.8660254037844387076, 1.000000000000000000, 0.8660254037844387076, 1.000000000000000000, 0.8660254037844387076, 1.000000000000000000, 0.8660254037844387076, 1.000000000000000000, 0.8660254037844387076, 1.000000000000000000, 0.8660254037844387076, 1.000000000000000000, 0.8660254037844387076, 1.000000000000000000, 0.8660254037844387076, 1.000000000000000000, 0.8660254037844387076, 1.000000000000000000, 0.8660254037844387076, 1.000000000000000000, 0.8660254037844387076, 1.000000000000000000, 0.8660254037844387076, 1.000000000000000000, 0.8660254037844387076, 1.000000000000000000, 0.8660254037844387076, 1.000000000000000000, 0.8660254037844387076, 1.000000000000000000, 0.8660254037844387076, 1.000000000000000000, 0.8660254037844387076, 1.000000000000000000, 0.8660254037844387076, 1.000000000000000000, 0.8660254037844387076, 1.000000000000000000, 0.8660254037844387076, 1.000000000000000000, 0.8660254037844387076, 1.000000000000000000, 0.8660254037844387076, 1.000000000000000000, 0.8660254037844387076, 1.000000000000000000, 0.8660254037844387076, 1.000000000000000000, 0.8660254037844387076, 1.000000000000000000, 0.8660254037844387076, 1.000000000000000000, 0.8660254037844387076, 1.000000000000000000, 0.8660254037844387076, 1.000000000000000000, 0.8660254037844387076, 1.000000000000000000, 0.8660254037844387076, 1.000000000000000000, 0.8660254037844387076, 1.000000000000000000, 0.8660254037844387076, 1.000000000000000000, 0.8660254037844387076, 1.000000000000000000, 0.8660254037844387076, 1.000000000000000000, 0.8660254037844387076, 1.000000000000000000, 0.8660254037844387076, 1.000000000000000000, 0.8660254037844387076, 1.000000000000000000, 0.8660254037844387076, 1.000000000000000000, 0.8660254037844387076, 1.000000000000000000, 0.8660254037844387076, 1.000000000000000000, 0.8660254037844387076, 1.000000000000000000, 0.8660254037844387076, 1.000000000000000000, 0.8660254037844387076, 1.000000000000000000, 0.8660254037844387076, 1.000000000000000000, 0.8660254037844387076, 1.000000000000000000, 0.8660254037844387076, 1.000000000000000000, 0.8660254037844387076, 1.000000000000000000, 0.8660254037844387076, 1.000000000000000000, 0.8660254037844387076, 1.000000000000000000, 0.8660254037844387076, 1.000000000000000000, 0.8660254037844387076, 1.000000000000000000, 0.8660254037844387076, 1.000000000000000000, 0.8660254037844387076, 1.000000000000000000, 0.8660254037844387076, 1.000000000000000000, 0.8660254037844387076, 1.000000000000000000, 0.8660254037844387076, 1.000000000000000000, 0.8660254037844387076, 1.000000000000000000, 0.8660254037844387076, 1.000000000000000000, 0.8660254037844387076, 1.000000000000000000, 0.8660254037844387076, 1.000000000000000000, 0.8660254037844387076, 1.000000000000000000, 0.8660254037844387076, 1.000000000000000000, 0.8660254037844387076, 1.000000000000000000, 0.8660254037844387076, 1.000000000000000000, 0.8660254037844387076, 1.000000000000000000, 0.8660254037844387076, 1.000000000000000000, 0.8660254037844387076, 1.000000000000000000, 0.8660254037844387076, 1.000000000000000000, 0.8660254037844387076, 1.000000000000000000, 0.8660254037844387076, 1.000000000000000000, 0.8660254037844387076, 1.000000000000000000, 0.8660254037844387076, 1.000000000000000000, 0.8660254037844387076, 1.000000000000000000, 0.8660254037844387076, 1.000000000000000000, 0.8660254037844387076, 1.000000000000000000, 0.8660254037844387076, 1.000000000000000000, 0.8660254037844387076, 1.000000000000000000, 0.8660254037844387076, 1.000000000000000000, 0.8660254037844387076, 1.000000000000000000, 0.8660254037844387076, 1.000000000000000000, 0.8660254037844387076, 1.000000000000000000, 0.8660254037844387076, 1.000000000000000000) ) ) 
 REPRESENTATION_ITEM ( '' )  SURFACE ( )  );
#66300 = AXIS2_PLACEMENT_3D ( 'NONE', #65551, #55933, #27870 ) ;
#66301 = CARTESIAN_POINT ( 'NONE',  ( 20.77500000122903145, -5.773502691896255534, -1.060575238724906372E-15 ) ) ;
#66302 = CARTESIAN_POINT ( 'NONE',  ( 4.243569643749999898, 14.68437500061451750, -30.00000000000000000 ) ) ;
#66303 = CARTESIAN_POINT ( 'NONE',  ( 20.63437500061451857, 6.421520780324663323E-16, -5.243569643749999010 ) ) ;
#66304 = CARTESIAN_POINT ( 'NONE',  ( 7.331250001229031810, 6.123233995736764310E-16, -4.999999999999998224 ) ) ;
#66305 = CARTESIAN_POINT ( 'NONE',  ( 5.100000001229034297, -2.886751345948125991, -5.000000000000000000 ) ) ;
#66306 = CARTESIAN_POINT ( 'NONE',  ( 4.321875000614517681, -6.054752690667223547, -1.112240025338166033E-15 ) ) ;
#66307 = CARTESIAN_POINT ( 'NONE',  ( 19.95937500061451786, 0.000000000000000000, 5.243569643749999010 ) ) ;
#66308 = CARTESIAN_POINT ( 'NONE',  ( 5.250000000000000888, 0.000000000000000000, 4.999999999999998224 ) ) ;
#66309 = CARTESIAN_POINT ( 'NONE',  ( 18.47812500061451857, 4.541064518000418104, 2.621784821874999949 ) ) ;
#66310 = CARTESIAN_POINT ( 'NONE',  ( 10.96875000122903465, 2.886751345948129099, -4.999999999999998224 ) ) ;
#66311 = CARTESIAN_POINT ( 'NONE',  ( 0.000000000000000000, 20.00000000000000000, 26.00000000000000000 ) ) ;
#66312 = DIRECTION ( 'NONE',  ( -0.000000000000000000, -1.000000000000000000, -0.000000000000000000 ) ) ;
#66313 = CARTESIAN_POINT ( 'NONE',  ( 27.64687500061452141, -3.027376345333614438, 5.243569643749998122 ) ) ;
#66314 = CARTESIAN_POINT ( 'NONE',  ( 20.25937500061451502, 2.746126346562643317, 4.756430356249998326 ) ) ;
#66315 = CARTESIAN_POINT ( 'NONE',  ( 15.14062500061451644, -3.027376345333610441, -5.243569643749999898 ) ) ;
#66316 = CARTESIAN_POINT ( 'NONE',  ( 13.13437500061451857, 4.541064518000418104, 2.621784821874999949 ) ) ;
#66317 = ORIENTED_EDGE ( 'NONE', *, *, #49986, .T. ) ;
#66318 = CARTESIAN_POINT ( 'NONE',  ( -1.487416814333745711E-14, 16.96250000000000213, -26.00000000000000000 ) ) ;
#66319 = CARTESIAN_POINT ( 'NONE',  ( 23.39062500061451289, 6.054752690667223547, 3.707466751127219781E-16 ) ) ;
#66320 = DIRECTION ( 'NONE',  ( 0.000000000000000000, 1.000000000000000000, 0.000000000000000000 ) ) ;
#66321 = CARTESIAN_POINT ( 'NONE',  ( -1.071796769724488563, 18.40490381179670365, 34.00000000000000000 ) ) ;
#66322 = CARTESIAN_POINT ( 'NONE',  ( 13.01249999999999929, -5.773502691896255534, -1.060575238724906372E-15 ) ) ;
#66323 = CARTESIAN_POINT ( 'NONE',  ( 25.20000000122903216, -2.886751345948129988, 4.999999999999997335 ) ) ;
#66324 = CARTESIAN_POINT ( 'NONE',  ( 17.72812500061451502, -4.541064518000419881, 2.621784821874995952 ) ) ;
#66325 = ORIENTED_EDGE ( 'NONE', *, *, #14684, .F. ) ;
#66326 = CARTESIAN_POINT ( 'NONE',  ( 21.48750000000000071, -2.886751345948129988, 4.999999999999997335 ) ) ;
#66327 = CARTESIAN_POINT ( 'NONE',  ( 22.80937500061451573, -4.541064518000417216, -2.621784821875001281 ) ) ;
#66328 = ORIENTED_EDGE ( 'NONE', *, *, #72661, .T. ) ;
#66329 = CARTESIAN_POINT ( 'NONE',  ( 21.20625000122903359, -4.330127018922190985, -2.500000000000001332 ) ) ;
#66330 = CARTESIAN_POINT ( 'NONE',  ( 10.07812500061451644, -4.541064518000419881, 2.621784821874995952 ) ) ;
#66331 = CARTESIAN_POINT ( 'NONE',  ( 3.263151822586646933, 3.788417924198219655, 3.593707371173769261 ) ) ;
#66332 = CARTESIAN_POINT ( 'NONE',  ( 14.48437500061451644, -2.746126346562646425, 4.756430356249996549 ) ) ;
#66333 = CARTESIAN_POINT ( 'NONE',  ( 17.10000000000000142, -4.330127018922190985, -2.500000000000001332 ) ) ;
#66334 = CARTESIAN_POINT ( 'NONE',  ( 25.16249999999999432, -5.773502691896255534, -1.060575238724906372E-15 ) ) ;
#66335 = CARTESIAN_POINT ( 'NONE',  ( 7.762500000000001066, 2.886751345948062486, -5.000000000000113687 ) ) ;
#66336 = CARTESIAN_POINT ( 'NONE',  ( 4.321875000614517681, -6.054752690667223547, -1.112240025338166033E-15 ) ) ;
#66337 = CARTESIAN_POINT ( 'NONE',  ( 16.39687500061451786, -3.027376345333614438, 5.243569643749998122 ) ) ;
#66338 = CARTESIAN_POINT ( 'NONE',  ( 27.75937500061451502, -4.541064518000417216, -2.621784821875001281 ) ) ;
#66339 = ORIENTED_EDGE ( 'NONE', *, *, #22055, .T. ) ;
#66340 = CARTESIAN_POINT ( 'NONE',  ( 26.65312500061451573, 0.000000000000000000, 5.243569643749999010 ) ) ;
#66341 = CARTESIAN_POINT ( 'NONE',  ( 28.88437500061451502, 4.541064518000418104, 2.621784821874999949 ) ) ;
#66342 = CARTESIAN_POINT ( 'NONE',  ( 5.810221930991193690E-16, 17.56250000000000000, 26.00000000000000000 ) ) ;
#66343 = CARTESIAN_POINT ( 'NONE',  ( 14.51250000000000107, 2.886751345948129099, -4.999999999999998224 ) ) ;
#66344 = CARTESIAN_POINT ( 'NONE',  ( 10.49062500061451431, -3.027376345333614438, 5.243569643749998122 ) ) ;
#66345 = CARTESIAN_POINT ( 'NONE',  ( 5.962500000000002132, 2.886751345948129099, -4.999999999999997335 ) ) ;
#66346 = CARTESIAN_POINT ( 'NONE',  ( 7.275000000000000355, 6.123233995736764310E-16, -4.999999999999998224 ) ) ;
#66347 = CARTESIAN_POINT ( 'NONE',  ( 28.64062500061451644, -3.027376345333610441, -5.243569643749999898 ) ) ;
#66348 = CARTESIAN_POINT ( 'NONE',  ( 17.02500000122903145, 2.886751345948126879, 4.999999999999999112 ) ) ;
#66349 = CARTESIAN_POINT ( 'NONE',  ( 26.90625000122902932, 0.000000000000000000, 4.999999999999998224 ) ) ;
#66350 = CARTESIAN_POINT ( 'NONE',  ( 15.04687500061451644, -2.746126346562646425, 4.756430356249996549 ) ) ;
#66351 = CARTESIAN_POINT ( 'NONE',  ( 4.565625000614516260, 3.027376345333611329, 5.243569643749999010 ) ) ;
#66352 = CARTESIAN_POINT ( 'NONE',  ( 21.38437500061451502, -4.541064518000419881, 2.621784821874995952 ) ) ;
#66353 = CARTESIAN_POINT ( 'NONE',  ( 9.001249775931846008E-16, 15.92187500061451821, 34.90005215228797653 ) ) ;
#66354 = EDGE_CURVE ( 'NONE', #65915, #27313, #53305, .T. ) ;
#66355 = CARTESIAN_POINT ( 'NONE',  ( 21.30937500061451573, 0.000000000000000000, 5.243569643749999010 ) ) ;
#66356 = CARTESIAN_POINT ( 'NONE',  ( 28.62187500061451573, -6.054752690667223547, -1.112240025338166033E-15 ) ) ;
#66357 = CARTESIAN_POINT ( 'NONE',  ( 9.001249775931846008E-16, 19.52187500061451786, 34.90005215228797653 ) ) ;
#66358 = CARTESIAN_POINT ( 'NONE',  ( 11.35312500061451679, 0.000000000000000000, 5.243569643749999010 ) ) ;
#66360 =( BOUNDED_CURVE ( )  B_SPLINE_CURVE ( 2, ( #29331, #63657, #40064, #7157, #8891, #29686, #46322 ),
 .UNSPECIFIED., .F., .F. ) 
 B_SPLINE_CURVE_WITH_KNOTS ( ( 3, 2, 2, 3 ),
 ( 0.5083333333333334147, 0.5111111111111110716, 0.5138888888888888395, 0.5166666666666666075 ),
 .UNSPECIFIED. ) 
 CURVE ( )  GEOMETRIC_REPRESENTATION_ITEM ( )  RATIONAL_B_SPLINE_CURVE ( ( 0.9999999999999946709, 0.8660254037844440367, 1.000000000000000000, 0.8660254037844387076, 1.000000000000000000, 0.8660254037844440367, 0.9999999999999946709 ) ) 
 REPRESENTATION_ITEM ( '' )  );
#66359 = CARTESIAN_POINT ( 'NONE',  ( -1.071796769724488563, 15.25490381179670152, 34.00000000000000000 ) ) ;
#66361 = AXIS2_PLACEMENT_3D ( 'NONE', #67781, #61499, #5360 ) ;
#66362 = CARTESIAN_POINT ( 'NONE',  ( 7.059375000614518392, -4.541064518000417216, -2.621784821875001281 ) ) ;
#66363 = CARTESIAN_POINT ( 'NONE',  ( 1.071796769724489895, 15.81740381056766509, -34.00000000000000000 ) ) ;
#66364 = CARTESIAN_POINT ( 'NONE',  ( 10.75312500061451715, 4.541064518000418104, -2.621784821874998173 ) ) ;
#66365 = CARTESIAN_POINT ( 'NONE',  ( 14.78437500061451715, 6.421520780324663323E-16, -5.243569643749999010 ) ) ;
#66366 = CARTESIAN_POINT ( 'NONE',  ( 22.61250000122903003, -4.330127018922190985, -2.500000000000001332 ) ) ;
#66367 = CARTESIAN_POINT ( 'NONE',  ( 8.334375000614516082, -4.541064518000419881, 2.621784821874995952 ) ) ;
#66368 = B_SPLINE_CURVE_WITH_KNOTS ( 'NONE', 3,
 ( #63559, #6695, #29940, #7055, #58004, #24028, #47299, #23669, #29583, #52121 ),
 .UNSPECIFIED., .F., .F.,
 ( 4, 3, 3, 4 ),
 ( 2.168404344971008868E-19, 5.625121263557876196E-05, 0.0001067941766033528262, 0.0001573439915068947906 ),
 .UNSPECIFIED. ) ;
#66369 = CARTESIAN_POINT ( 'NONE',  ( 9.028125000614517504, 4.541064518000418104, 2.621784821874999949 ) ) ;
#66370 = CARTESIAN_POINT ( 'NONE',  ( 24.65625000122903288, 0.000000000000000000, 4.999999999999998224 ) ) ;
#66371 = CARTESIAN_POINT ( 'NONE',  ( 21.27187500061451786, 3.027376345333611329, 5.243569643749999010 ) ) ;
#66372 = CARTESIAN_POINT ( 'NONE',  ( -5.810221930991193690E-16, 13.58750000000000036, 26.00000000000000355 ) ) ;
#66373 = CARTESIAN_POINT ( 'NONE',  ( -1.349117715399773321, 4.821506530989291939, 33.77511393033235976 ) ) ;
#66374 = CARTESIAN_POINT ( 'NONE',  ( 29.25937500061451502, 4.541064518000418104, -2.621784821874998173 ) ) ;
#66375 = CARTESIAN_POINT ( 'NONE',  ( -4.243569643749999898, 11.75937500061451857, -30.00000000000000000 ) ) ;
#66376 = CARTESIAN_POINT ( 'NONE',  ( 14.21250000122903323, 4.330127018922192761, -2.499999999999997780 ) ) ;
#66377 = CARTESIAN_POINT ( 'NONE',  ( -2.121784821874999949, 16.57812500061451644, -33.67503911421598417 ) ) ;
#66378 = CARTESIAN_POINT ( 'NONE',  ( 18.63750000122903216, 6.123233995736764310E-16, -4.999999999999998224 ) ) ;
#66379 = CARTESIAN_POINT ( 'NONE',  ( 11.12812500061451715, 6.421520780324663323E-16, -5.243569643749999010 ) ) ;
#66380 = VERTEX_POINT ( 'NONE', #46385 ) ;
#66381 = CARTESIAN_POINT ( 'NONE',  ( 13.91249999999999964, -5.773502691896255534, -1.060575238724906372E-15 ) ) ;
#66382 = CARTESIAN_POINT ( 'NONE',  ( 13.78125000122903288, 4.330127018922191873, 2.499999999999999556 ) ) ;
#66383 = CARTESIAN_POINT ( 'NONE',  ( 23.91562500061451502, 3.027376345333611329, 5.243569643749999010 ) ) ;
#66384 = CARTESIAN_POINT ( 'NONE',  ( 10.50937500061451679, 0.000000000000000000, 5.243569643749999010 ) ) ;
#66385 = CARTESIAN_POINT ( 'NONE',  ( -1.071796769724491005, 14.17009619066136672, 26.00000000000000355 ) ) ;
#66386 = CARTESIAN_POINT ( 'NONE',  ( 10.50000000122903465, -2.886751345948125991, -5.000000000000000000 ) ) ;
#66387 = CARTESIAN_POINT ( 'NONE',  ( 17.96250000122903501, 0.000000000000000000, 4.999999999999998224 ) ) ;
#66388 = CARTESIAN_POINT ( 'NONE',  ( 15.51562500061451644, -6.054752690667223547, -1.112240025338166033E-15 ) ) ;
#66389 = CARTESIAN_POINT ( 'NONE',  ( 17.80312500061451786, -4.541064518000417216, -2.621784821875001281 ) ) ;
#66390 = CARTESIAN_POINT ( 'NONE',  ( 24.82500000122902861, -5.773502691896255534, -1.060575238724906372E-15 ) ) ;
#66391 = CARTESIAN_POINT ( 'NONE',  ( 27.37500000122903288, 2.886751345948126879, 4.999999999999999112 ) ) ;
#66392 = CARTESIAN_POINT ( 'NONE',  ( 23.13749999999999929, 5.773502691896255534, 3.535250795749688894E-16 ) ) ;
#66393 = CARTESIAN_POINT ( 'NONE',  ( 1.878215178124997609, 13.01562499938548356, 33.25316411605952993 ) ) ;
#66394 = CARTESIAN_POINT ( 'NONE',  ( 25.02187500061451431, -6.054752690667223547, -1.112240025338166033E-15 ) ) ;
#66395 = CARTESIAN_POINT ( 'NONE',  ( 3.999999999999998668, 12.61250000000000249, -32.30940107675850470 ) ) ;
#66396 = EDGE_CURVE ( 'NONE', #14534, #54755, #14054, .T. ) ;
#66397 = CARTESIAN_POINT ( 'NONE',  ( 12.03750000122903430, 4.330127018922191873, 2.499999999999999556 ) ) ;
#66398 = CARTESIAN_POINT ( 'NONE',  ( 4.537500000000000533, -2.886751345948125991, -5.000000000000000000 ) ) ;
#66399 = CARTESIAN_POINT ( 'NONE',  ( -1.071796769724490339, 18.42634618820330061, 26.00000000000000000 ) ) ;
#66400 = CARTESIAN_POINT ( 'NONE',  ( 5.821875000614519458, 3.027376345333613106, -5.243569643749998122 ) ) ;
#66401 = PRESENTATION_LAYER_ASSIGNMENT (  '', '', ( #46204 ) ) ;
#66402 = CARTESIAN_POINT ( 'NONE',  ( 26.01562500061451289, 3.027376345333613106, -5.243569643749998122 ) ) ;
#66403 = CARTESIAN_POINT ( 'NONE',  ( 2.393811435568372112E-14, 16.88750000000000284, 34.00000000000000000 ) ) ;
#66404 = DIRECTION ( 'NONE',  ( 0.000000000000000000, 0.000000000000000000, 1.000000000000000000 ) ) ;
#66405 = CARTESIAN_POINT ( 'NONE',  ( 11.40937500061451892, 0.000000000000000000, 5.243569643749999010 ) ) ;
#66406 = CARTESIAN_POINT ( 'NONE',  ( 4.259027106289364539, -2.619388203951992455, 4.518412407730628466 ) ) ;
#66407 = CARTESIAN_POINT ( 'NONE',  ( 3.346875000614518036, -3.027376345333614438, 5.243569643749998122 ) ) ;
#66408 = CARTESIAN_POINT ( 'NONE',  ( 7.959375000614516971, -4.541064518000417216, -2.621784821875001281 ) ) ;
#66409 = CARTESIAN_POINT ( 'NONE',  ( 28.35937500061451289, 4.541064518000418104, -2.621784821874998173 ) ) ;
#66410 = CARTESIAN_POINT ( 'NONE',  ( 2.121784821874999061, 13.35312500061459318, 26.32496088578401583 ) ) ;
#66411 = CARTESIAN_POINT ( 'NONE',  ( 22.61250000000000071, 2.886751345948129099, -4.999999999999998224 ) ) ;
#66412 = EDGE_LOOP ( 'NONE', ( #20982, #56283, #41637, #27323 ) ) ;
#66413 = CARTESIAN_POINT ( 'NONE',  ( 29.73750000000000071, -2.886751345948125991, -5.000000000000000000 ) ) ;
#66414 = CARTESIAN_POINT ( 'NONE',  ( 3.337499999999999911, 5.773502691896255534, 3.535250795749688894E-16 ) ) ;
#66415 = ORIENTED_EDGE ( 'NONE', *, *, #3065, .F. ) ;
#66416 = CARTESIAN_POINT ( 'NONE',  ( 17.57812500061451644, 4.541064518000418104, 2.621784821874999949 ) ) ;
#66417 = CARTESIAN_POINT ( 'NONE',  ( 11.76562500061451644, 3.027376345333611329, 5.243569643749999010 ) ) ;
#66418 = CARTESIAN_POINT ( 'NONE',  ( 21.30937500061451217, -5.492252693125287522, -1.008910452111647106E-15 ) ) ;
#66419 = CARTESIAN_POINT ( 'NONE',  ( 6.459375000614518747, 0.000000000000000000, 5.243569643749999010 ) ) ;
#66420 = CARTESIAN_POINT ( 'NONE',  ( 19.20000000122903572, 5.773502691896255534, 3.535250795749688894E-16 ) ) ;
#66421 = DIRECTION ( 'NONE',  ( 1.000000000000000000, 0.000000000000000000, 0.000000000000000000 ) ) ;
#66422 = CARTESIAN_POINT ( 'NONE',  ( 6.121875000614517504, -6.054752690667223547, -1.112240025338166033E-15 ) ) ;
#66423 = CARTESIAN_POINT ( 'NONE',  ( 15.19687500061451857, -3.027376345333610441, -5.243569643749999898 ) ) ;
#66424 = CARTESIAN_POINT ( 'NONE',  ( 24.38437500061451502, 4.541064518000418104, 2.621784821874999949 ) ) ;
#66425 = CARTESIAN_POINT ( 'NONE',  ( -2.000000000000000000, 14.52500000000000036, -33.46410161513775705 ) ) ;
#66426 = ORIENTED_EDGE ( 'NONE', *, *, #3972, .T. ) ;
#66427 = CARTESIAN_POINT ( 'NONE',  ( 13.57500000000000107, 6.123233995736764310E-16, -4.999999999999998224 ) ) ;
#66428 = CARTESIAN_POINT ( 'NONE',  ( 17.85937500061451999, -4.541064518000417216, -2.621784821875001281 ) ) ;
#66429 = CARTESIAN_POINT ( 'NONE',  ( 10.43437500061451750, 4.541064518000418104, 2.621784821874999949 ) ) ;
#66430 = CARTESIAN_POINT ( 'NONE',  ( -7.967954043666661671E-16, 15.67812499938548321, 34.33755215474603517 ) ) ;
#66431 = CARTESIAN_POINT ( 'NONE',  ( 21.07499999999999929, -4.330127018922194537, 2.499999999999995559 ) ) ;
#66432 = CARTESIAN_POINT ( 'NONE',  ( -4.000000000000000000, 16.77499999999999858, 30.00000000000000000 ) ) ;
#66433 = CARTESIAN_POINT ( 'NONE',  ( 4.243569643749999898, 10.63437500061451857, -30.00000000000000000 ) ) ;
#66434 = CARTESIAN_POINT ( 'NONE',  ( 22.13437500061451502, 4.119189519843966529, 2.378215178124999607 ) ) ;
#66435 = CARTESIAN_POINT ( 'NONE',  ( 13.19062500061451537, -3.027376345333614438, 5.243569643749998122 ) ) ;
#66436 = CARTESIAN_POINT ( 'NONE',  ( 28.47187500061451715, 3.027376345333611329, 5.243569643749999010 ) ) ;
#66437 = CARTESIAN_POINT ( 'NONE',  ( 6.750000001229033764, -2.886751345948130876, 4.999999999999996447 ) ) ;
#66438 = CARTESIAN_POINT ( 'NONE',  ( 27.64687500061452141, -3.027376345333614438, 5.243569643749998122 ) ) ;
#66439 = CARTESIAN_POINT ( 'NONE',  ( 10.35000000000000142, -4.330127018922190985, -2.500000000000001332 ) ) ;
#66440 = EDGE_CURVE ( 'NONE', #31771, #9134, #922, .T. ) ;
#66441 = CARTESIAN_POINT ( 'NONE',  ( -2.828200636599751609E-16, 15.50000000122903465, 25.38119784648299770 ) ) ;
#66442 = CARTESIAN_POINT ( 'NONE',  ( 11.55000000122903181, 5.773502691896255534, 3.535250795749688894E-16 ) ) ;
#66443 = CARTESIAN_POINT ( 'NONE',  ( 23.33437500061451786, 6.421520780324663323E-16, -5.243569643749999010 ) ) ;
#66444 = CARTESIAN_POINT ( 'NONE',  ( 13.84687500061451537, -3.027376345333610441, -5.243569643749999898 ) ) ;
#66445 = CARTESIAN_POINT ( 'NONE',  ( 1.071796769724484344, 16.64509619066136992, 34.00000000000000000 ) ) ;
#66446 = VERTEX_POINT ( 'NONE', #62642 ) ;
#66447 = CARTESIAN_POINT ( 'NONE',  ( 16.41562500061451857, -6.054752690667223547, -1.112240025338166033E-15 ) ) ;
#66448 = CARTESIAN_POINT ( 'NONE',  ( 29.58750000122903501, 4.330127018922191873, 2.499999999999999556 ) ) ;
#66449 = CARTESIAN_POINT ( 'NONE',  ( 14.10937500061451644, 0.000000000000000000, 5.243569643749999010 ) ) ;
#66450 = CARTESIAN_POINT ( 'NONE',  ( 4.765820465973555464, 8.794739343793304798, -26.33488593128669919 ) ) ;
#66451 = CARTESIAN_POINT ( 'NONE',  ( 19.64062500061451644, -3.027376345333610441, -5.243569643749999898 ) ) ;
#66452 = CARTESIAN_POINT ( 'NONE',  ( 1.999999999999998668, 16.69999999999999929, -33.46410161513775705 ) ) ;
#66453 = CARTESIAN_POINT ( 'NONE',  ( 29.22187500061451715, 3.027376345333613106, -5.243569643749998122 ) ) ;
#66454 = CARTESIAN_POINT ( 'NONE',  ( -2.121784821874996840, 13.12812500061451715, 33.67503911421598417 ) ) ;
#66455 = CARTESIAN_POINT ( 'NONE',  ( 17.44687500061451857, -3.027376345333610441, -5.243569643749999898 ) ) ;
#66456 = CARTESIAN_POINT ( 'NONE',  ( 14.36250000122903359, 0.000000000000000000, 4.999999999999998224 ) ) ;
#66457 = CARTESIAN_POINT ( 'NONE',  ( 10.20937500061451786, -4.119189519843965641, -2.378215178125001383 ) ) ;
#66458 = CARTESIAN_POINT ( 'NONE',  ( 4.243569643749999010, 18.32187500061451502, -32.45002607614398471 ) ) ;
#66459 = CARTESIAN_POINT ( 'NONE',  ( 21.12187500061451573, 3.027376345333613106, -5.243569643749998122 ) ) ;
#66460 = CARTESIAN_POINT ( 'NONE',  ( 23.21250000122903501, 4.330127018922192761, -2.499999999999997780 ) ) ;
#66461 = CARTESIAN_POINT ( 'NONE',  ( 16.09687500061452070, -3.027376345333610441, -5.243569643749999898 ) ) ;
#66462 = CARTESIAN_POINT ( 'NONE',  ( 12.25312500061451537, 0.000000000000000000, 5.243569643749999010 ) ) ;
#66463 = CARTESIAN_POINT ( 'NONE',  ( -4.243569643749999898, 11.30937500061451928, 30.00000000000000000 ) ) ;
#66464 = CARTESIAN_POINT ( 'NONE',  ( 17.42812500061451786, 6.421520780324663323E-16, -5.243569643749999010 ) ) ;
#66465 = ORIENTED_EDGE ( 'NONE', *, *, #13122, .T. ) ;
#66466 = EDGE_LOOP ( 'NONE', ( #37293, #70548 ) ) ;
#66467 = CARTESIAN_POINT ( 'NONE',  ( 19.76250000000000639, -5.773502691896255534, -1.060575238724906372E-15 ) ) ;
#66468 = CYLINDRICAL_SURFACE ( 'NONE', #59772, 4.000000000000000000 ) ;
#66469 = CARTESIAN_POINT ( 'NONE',  ( 23.87812500061451715, 4.541064518000418104, 2.621784821874999949 ) ) ;
#66470 = CARTESIAN_POINT ( 'NONE',  ( 6.290625000614517681, 6.054752690667223547, 3.707466751127219781E-16 ) ) ;
#66471 = CARTESIAN_POINT ( 'NONE',  ( 17.32500000122903216, 2.886751345948129099, -4.999999999999998224 ) ) ;
#66472 = CARTESIAN_POINT ( 'NONE',  ( 22.60312500061451857, 0.000000000000000000, 5.243569643749999010 ) ) ;
#66473 = CARTESIAN_POINT ( 'NONE',  ( 23.88749999999999929, -2.886751345948125991, -5.000000000000000000 ) ) ;
#66474 = CARTESIAN_POINT ( 'NONE',  ( 24.89062500061451644, -3.027376345333614438, 5.243569643749998122 ) ) ;
#66475 = CARTESIAN_POINT ( 'NONE',  ( 5.615625000614517859, -6.054752690667223547, -1.112240025338166033E-15 ) ) ;
#66476 = ORIENTED_EDGE ( 'NONE', *, *, #44600, .T. ) ;
#66477 = CARTESIAN_POINT ( 'NONE',  ( 24.25312500061451715, 4.541064518000418104, -2.621784821874998173 ) ) ;
#66478 = CARTESIAN_POINT ( 'NONE',  ( -1.071796769724490783, 13.21115380933863293, 34.00000000000000711 ) ) ;
#66479 = CARTESIAN_POINT ( 'NONE',  ( 11.18437500061451928, 5.824947211148865298E-16, -4.756430356249998326 ) ) ;
#66480 = DIRECTION ( 'NONE',  ( 0.000000000000000000, 0.000000000000000000, -1.000000000000000000 ) ) ;
#66481 = CARTESIAN_POINT ( 'NONE',  ( -3.999999999999997335, 13.40000000122903323, -27.69059892324149175 ) ) ;
#66482 = CARTESIAN_POINT ( 'NONE',  ( -1.071796769724491005, 10.12009619066136956, 26.00000000000000355 ) ) ;
#66483 = CARTESIAN_POINT ( 'NONE',  ( 10.76250000000000107, -5.773502691896255534, -1.060575238724906372E-15 ) ) ;
#66484 = CARTESIAN_POINT ( 'NONE',  ( 11.03437500061451715, -4.541064518000419881, 2.621784821874995952 ) ) ;
#66485 = CARTESIAN_POINT ( 'NONE',  ( 6.637500001229035718, 4.330127018922191873, 2.499999999999999556 ) ) ;
#66486 = CARTESIAN_POINT ( 'NONE',  ( 15.15937500061451715, -4.541064518000417216, -2.621784821875001281 ) ) ;
#66487 = CARTESIAN_POINT ( 'NONE',  ( 5.109375000614518214, 0.000000000000000000, 5.243569643749999010 ) ) ;
#66488 = CARTESIAN_POINT ( 'NONE',  ( 45.00000000000000000, 0.000000000000000000, 0.000000000000000000 ) ) ;
#66489 = CARTESIAN_POINT ( 'NONE',  ( 12.75937500061451857, 0.000000000000000000, 5.243569643749999010 ) ) ;
#66490 = CARTESIAN_POINT ( 'NONE',  ( 30.00000000000000000, 0.000000000000000000, 0.000000000000000000 ) ) ;
#66491 = CARTESIAN_POINT ( 'NONE',  ( 19.79062500061451502, 6.054752690667223547, 3.707466751127219781E-16 ) ) ;
#66492 = LINE ( 'NONE', #21780, #9985 ) ;
#66493 = CARTESIAN_POINT ( 'NONE',  ( 24.42187500061451999, 3.027376345333611329, 5.243569643749999010 ) ) ;
#66494 =( BOUNDED_CURVE ( )  B_SPLINE_CURVE ( 2, ( #10707, #33595, #28071, #26982, #4453, #72767, #55415 ),
 .UNSPECIFIED., .F., .F. ) 
 B_SPLINE_CURVE_WITH_KNOTS ( ( 3, 2, 2, 3 ),
 ( 0.4916666666666666408, 0.4944444444444444642, 0.4972222222222222321, 0.5000000000000000000 ),
 .UNSPECIFIED. ) 
 CURVE ( )  GEOMETRIC_REPRESENTATION_ITEM ( )  RATIONAL_B_SPLINE_CURVE ( ( 1.000000000000000000, 0.8660254037844387076, 1.000000000000000000, 0.8660254037844387076, 1.000000000000000000, 0.8660254037844387076, 1.000000000000000000 ) ) 
 REPRESENTATION_ITEM ( '' )  );
#66495 = CARTESIAN_POINT ( 'NONE',  ( 1.071796769724490117, 19.23259618943233917, 33.99999999999999289 ) ) ;
#66496 = CARTESIAN_POINT ( 'NONE',  ( 29.62500000122903288, 2.886751345948126879, 4.999999999999999112 ) ) ;
#66497 = EDGE_CURVE ( 'NONE', #69242, #28919, #66953, .T. ) ;
#66498 = CARTESIAN_POINT ( 'NONE',  ( 20.67187500061451289, 4.119189519843966529, 2.378215178124999607 ) ) ;
#66499 = CARTESIAN_POINT ( 'NONE',  ( 25.49062500061451786, -3.027376345333610441, -5.243569643749999898 ) ) ;
#66500 = CARTESIAN_POINT ( 'NONE',  ( 17.39062500061451644, -3.027376345333610441, -5.243569643749999898 ) ) ;
#66501 = CARTESIAN_POINT ( 'NONE',  ( 13.70625000122903359, 4.330127018922192761, -2.499999999999997780 ) ) ;
#66502 = CARTESIAN_POINT ( 'NONE',  ( 13.84687500061451537, -3.027376345333610441, -5.243569643749999898 ) ) ;
#66503 = CARTESIAN_POINT ( 'NONE',  ( 26.25000000122903288, -2.886751345948126435, -5.000000000000000000 ) ) ;
#66504 = CARTESIAN_POINT ( 'NONE',  ( 27.33750000122903145, 4.330127018922191873, 2.499999999999999556 ) ) ;
#66505 = CARTESIAN_POINT ( 'NONE',  ( 4.284375000614518925, -4.541064518000419881, 2.621784821874995952 ) ) ;
#66506 = CARTESIAN_POINT ( 'NONE',  ( 14.18437500061451750, -4.541064518000419881, 2.621784821874995952 ) ) ;
#66507 = CARTESIAN_POINT ( 'NONE',  ( 16.08750000000000213, -2.886751345948197045, 4.999999999999880096 ) ) ;
#66508 = FACE_OUTER_BOUND ( 'NONE', #58245, .T. ) ;
#66509 = CARTESIAN_POINT ( 'NONE',  ( 4.575000001229033941, -5.773502691896255534, -1.060575238724906372E-15 ) ) ;
#66510 = CARTESIAN_POINT ( 'NONE',  ( 24.04687500061451644, -3.027376345333614438, 5.243569643749998122 ) ) ;
#66511 = CARTESIAN_POINT ( 'NONE',  ( 16.69687500061451502, 6.054752690667223547, 3.707466751127219781E-16 ) ) ;
#66512 = CARTESIAN_POINT ( 'NONE',  ( -7.967954043666661671E-16, 16.69062499938548427, 34.33755215474603517 ) ) ;
#66513 = CARTESIAN_POINT ( 'NONE',  ( 27.89999999999999858, -4.330127018922190985, -2.500000000000001332 ) ) ;
#66514 = FACE_OUTER_BOUND ( 'NONE', #33188, .T. ) ;
#66515 = CARTESIAN_POINT ( 'NONE',  ( 5.775000000000002132, -4.330127018922194537, 2.499999999999995559 ) ) ;
#66516 = CARTESIAN_POINT ( 'NONE',  ( 28.50937500061451502, 0.000000000000000000, 4.756430356249998326 ) ) ;
#66517 = CARTESIAN_POINT ( 'NONE',  ( 20.42812500061451431, -4.541064518000419881, 2.621784821874995952 ) ) ;
#66518 = CARTESIAN_POINT ( 'NONE',  ( 9.750000000000001776, 0.000000000000000000, 4.999999999999998224 ) ) ;
#66519 = CARTESIAN_POINT ( 'NONE',  ( 4.453125000614517326, 4.541064518000418104, -2.621784821874998173 ) ) ;
#66520 = CARTESIAN_POINT ( 'NONE',  ( 20.17499999999999716, -4.330127018922194537, 2.499999999999995559 ) ) ;
#66521 = EDGE_CURVE ( 'NONE', #63984, #59354, #29394, .T. ) ;
#66522 = DIRECTION ( 'NONE',  ( 1.000000000000000000, 0.000000000000000000, 0.000000000000000000 ) ) ;
#66523 = CARTESIAN_POINT ( 'NONE',  ( 23.66250000122903430, 4.330127018922192761, -2.499999999999997780 ) ) ;
#66524 = CARTESIAN_POINT ( 'NONE',  ( 3.750000000000000000, 4.330127018922192761, -2.499999999999997780 ) ) ;
#66525 = ORIENTED_EDGE ( 'NONE', *, *, #29318, .T. ) ;
#66526 = CARTESIAN_POINT ( 'NONE',  ( 16.52812500061451573, 6.421520780324663323E-16, -5.243569643749999010 ) ) ;
#66527 = CARTESIAN_POINT ( 'NONE',  ( 25.41562500061451146, -6.054752690667223547, -1.112240025338166033E-15 ) ) ;
#66528 = CARTESIAN_POINT ( 'NONE',  ( 23.18437500061451573, -4.541064518000419881, 2.621784821874995952 ) ) ;
#66529 = CARTESIAN_POINT ( 'NONE',  ( 6.750000000000002665, -4.330127018922190985, -2.500000000000001332 ) ) ;
#66530 = CARTESIAN_POINT ( 'NONE',  ( 10.60312500061451679, -4.541064518000417216, -2.621784821875001281 ) ) ;
#66531 = CARTESIAN_POINT ( 'NONE',  ( 25.52812500061451573, 6.421520780324663323E-16, -5.243569643749999010 ) ) ;
#66532 = CARTESIAN_POINT ( 'NONE',  ( 14.52187500061451608, 3.027376345333611329, 5.243569643749999010 ) ) ;
#66533 = CARTESIAN_POINT ( 'NONE',  ( 20.29687500061451644, 6.054752690667223547, 3.707466751127219781E-16 ) ) ;
#66534 = CARTESIAN_POINT ( 'NONE',  ( -1.626862140677534273E-15, 19.58750000000000213, 34.00000000000000000 ) ) ;
#66535 = CARTESIAN_POINT ( 'NONE',  ( -4.243569643749997233, 19.39062500061451999, 32.45002607614398471 ) ) ;
#66536 = CARTESIAN_POINT ( 'NONE',  ( 21.22500000122903074, -5.773502691896255534, -1.060575238724906372E-15 ) ) ;
#66537 = CARTESIAN_POINT ( 'NONE',  ( 18.23437500061451999, -4.119189519843968306, 2.378215178124996054 ) ) ;
#66538 = CARTESIAN_POINT ( 'NONE',  ( 11.20312500061451644, 4.541064518000418104, -2.621784821874998173 ) ) ;
#66539 = CARTESIAN_POINT ( 'NONE',  ( 8.934375000614517504, 6.421520780324663323E-16, -5.243569643749999010 ) ) ;
#66540 = CARTESIAN_POINT ( 'NONE',  ( 7.659375000614518036, 4.541064518000418104, -2.621784821874998173 ) ) ;
#66541 = EDGE_CURVE ( 'NONE', #65176, #61955, #72116, .T. ) ;
#66542 = VERTEX_POINT ( 'NONE', #53370 ) ;
#66543 = CARTESIAN_POINT ( 'NONE',  ( 26.63437500061451857, 4.541064518000418104, 2.621784821874999949 ) ) ;
#66544 = CARTESIAN_POINT ( 'NONE',  ( 19.00312500061451715, 0.000000000000000000, 5.243569643749999010 ) ) ;
#66545 = CARTESIAN_POINT ( 'NONE',  ( 28.65000000122903145, 5.773502691896255534, 3.535250795749688894E-16 ) ) ;
#66546 = CARTESIAN_POINT ( 'NONE',  ( 29.16562500061451502, 3.027376345333613106, -5.243569643749998122 ) ) ;
#66547 = CARTESIAN_POINT ( 'NONE',  ( 24.19687500061451857, -3.027376345333610441, -5.243569643749999898 ) ) ;
#66548 = CARTESIAN_POINT ( 'NONE',  ( 20.16562500061451146, 3.027376345333613106, -5.243569643749998122 ) ) ;
#66549 = CARTESIAN_POINT ( 'NONE',  ( -1.999999999999997113, 12.42500000000000249, 33.46410161513775705 ) ) ;
#66550 = CARTESIAN_POINT ( 'NONE',  ( 24.25312500061451715, 4.541064518000418104, -2.621784821874998173 ) ) ;
#66551 = CARTESIAN_POINT ( 'NONE',  ( 4.350000001229033408, 5.773502691896255534, 3.535250795749688894E-16 ) ) ;
#66552 = ORIENTED_EDGE ( 'NONE', *, *, #41750, .F. ) ;
#66553 = CARTESIAN_POINT ( 'NONE',  ( 30.00000000000000000, 0.000000000000000000, 0.000000000000000000 ) ) ;
#66554 = CARTESIAN_POINT ( 'NONE',  ( -3.999999999999999112, 16.40000000000000213, -30.00000000000000000 ) ) ;
#66555 = CARTESIAN_POINT ( 'NONE',  ( -3.756430356249999214, 14.29062499938548214, 27.83122392262697531 ) ) ;
#66556 = CARTESIAN_POINT ( 'NONE',  ( 5.484375000614518214, 4.541064518000418104, 2.621784821874999949 ) ) ;
#66557 = LINE ( 'NONE', #15937, #47886 ) ;
#66558 = CARTESIAN_POINT ( 'NONE',  ( 12.59062500061451573, 6.054752690667223547, 3.707466751127219781E-16 ) ) ;
#66559 = CARTESIAN_POINT ( 'NONE',  ( 5.559375000614517504, 0.000000000000000000, 5.243569643749999010 ) ) ;
#66560 = CARTESIAN_POINT ( 'NONE',  ( 25.68750000122903288, -4.330127018922194537, 2.499999999999995559 ) ) ;
#66561 =( BOUNDED_CURVE ( )  B_SPLINE_CURVE ( 2, ( #21239, #71499, #3907, #33062, #32705, #55242, #14600, #54144, #66318 ),
 .UNSPECIFIED., .F., .F. ) 
 B_SPLINE_CURVE_WITH_KNOTS ( ( 3, 2, 2, 2, 3 ),
 ( 0.2717391304347826497, 0.2753623188405797118, 0.2826086956521738913, 0.2898550724637681264, 0.2934782608695652439 ),
 .UNSPECIFIED. ) 
 CURVE ( )  GEOMETRIC_REPRESENTATION_ITEM ( )  RATIONAL_B_SPLINE_CURVE ( ( 0.9330127018922194093, 0.9330127018922198534, 1.000000000000000000, 0.8660254037844387076, 1.000000000000000000, 0.8660254037844387076, 1.000000000000000000, 0.9330127018922188542, 0.9330127018922194093 ) ) 
 REPRESENTATION_ITEM ( '' )  );
#66562 = CARTESIAN_POINT ( 'NONE',  ( 15.34687500061451892, 6.054752690667223547, 3.707466751127219781E-16 ) ) ;
#66563 = CARTESIAN_POINT ( 'NONE',  ( 28.60312500061451502, -4.541064518000417216, -2.621784821875001281 ) ) ;
#66564 = CARTESIAN_POINT ( 'NONE',  ( -3.999999999999997335, 11.03749999999999964, 32.30940107675850470 ) ) ;
#66565 = CARTESIAN_POINT ( 'NONE',  ( 27.12187500061451573, 3.027376345333611329, 5.243569643749999010 ) ) ;
#66566 = CARTESIAN_POINT ( 'NONE',  ( 3.665625000614517681, 3.027376345333611329, 5.243569643749999010 ) ) ;
#66567 = CARTESIAN_POINT ( 'NONE',  ( 12.89062500061451821, -3.027376345333610441, -5.243569643749999898 ) ) ;
#66568 = ORIENTED_EDGE ( 'NONE', *, *, #58543, .F. ) ;
#66569 = CARTESIAN_POINT ( 'NONE',  ( 9.440625000614517148, 6.054752690667223547, 3.707466751127219781E-16 ) ) ;
#66570 = VECTOR ( 'NONE', #23551, 1000.000000000000000 ) ;
#66571 = CARTESIAN_POINT ( 'NONE',  ( 8.728125000614518569, -4.541064518000419881, 2.621784821874995952 ) ) ;
#66572 = CARTESIAN_POINT ( 'NONE',  ( 19.50937500061451857, 0.000000000000000000, 4.756430356249998326 ) ) ;
#66573 = CARTESIAN_POINT ( 'NONE',  ( 8.962500000000002132, -5.773502691896255534, -1.060575238724906372E-15 ) ) ;
#66574 = CARTESIAN_POINT ( 'NONE',  ( 3.937500001229034208, 4.330127018922191873, 2.499999999999999556 ) ) ;
#66575 = CARTESIAN_POINT ( 'NONE',  ( 17.81250000000000355, 2.886751345948126879, 4.999999999999999112 ) ) ;
#66576 = EDGE_CURVE ( 'NONE', #35463, #40816, #3721, .T. ) ;
#66577 =( BOUNDED_CURVE ( )  B_SPLINE_CURVE ( 2, ( #49597, #4895, #43690, #10432, #5254, #9700, #10792 ),
 .UNSPECIFIED., .F., .F. ) 
 B_SPLINE_CURVE_WITH_KNOTS ( ( 3, 2, 2, 3 ),
 ( 0.2399999999999999634, 0.2433333333333333182, 0.2466666666666666452, 0.2499999999999999722 ),
 .UNSPECIFIED. ) 
 CURVE ( )  GEOMETRIC_REPRESENTATION_ITEM ( )  RATIONAL_B_SPLINE_CURVE ( ( 1.000000000000001110, 0.8660254037844374864, 1.000000000000000000, 0.8660254037844387076, 1.000000000000000000, 0.8660254037844398178, 0.9999999999999988898 ) ) 
 REPRESENTATION_ITEM ( '' )  );
#66578 = CARTESIAN_POINT ( 'NONE',  ( 19.39687500061451786, 6.054752690667223547, 3.707466751127219781E-16 ) ) ;
#66579 = CARTESIAN_POINT ( 'NONE',  ( 13.31250000122903288, 4.330127018922192761, -2.499999999999997780 ) ) ;
#66580 = CARTESIAN_POINT ( 'NONE',  ( 20.32499999999999929, 6.123233995736764310E-16, -4.999999999999998224 ) ) ;
#66581 = CARTESIAN_POINT ( 'NONE',  ( 4.243569643749999898, 15.94062500061451537, -27.54997392385601529 ) ) ;
#66582 = CYLINDRICAL_SURFACE ( 'NONE', #71319, 1.500000000000000444 ) ;
#66583 = CARTESIAN_POINT ( 'NONE',  ( 3.507483327083503521, -3.563363679198468859, 3.507483327083555924 ) ) ;
#66584 = CARTESIAN_POINT ( 'NONE',  ( 28.79062500061451502, 6.054752690667223547, 3.707466751127219781E-16 ) ) ;
#66585 = LINE ( 'NONE', #38883, #51702 ) ;
#66586 = LINE ( 'NONE', #21874, #72735 ) ;
#66587 = CARTESIAN_POINT ( 'NONE',  ( 12.75937500061451857, 0.000000000000000000, 5.243569643749999010 ) ) ;
#66588 = CARTESIAN_POINT ( 'NONE',  ( 27.67499999999999716, 4.330127018922191873, 2.499999999999999556 ) ) ;
#66589 = CARTESIAN_POINT ( 'NONE',  ( 9.440625000614517148, 6.054752690667223547, 3.707466751127219781E-16 ) ) ;
#66590 = B_SPLINE_CURVE_WITH_KNOTS ( 'NONE', 1,
 ( #44681, #28046 ),
 .UNSPECIFIED., .F., .F.,
 ( 2, 2 ),
 ( 0.000000000000000000, 1.000000000000000000 ),
 .UNSPECIFIED. ) ;
#66591 = CARTESIAN_POINT ( 'NONE',  ( 27.04687500061451289, 0.000000000000000000, 4.756430356249998326 ) ) ;
#66592 =( BOUNDED_CURVE ( )  B_SPLINE_CURVE ( 3, ( #24496, #67144, #47039, #41494 ),
 .UNSPECIFIED., .F., .F. ) 
 B_SPLINE_CURVE_WITH_KNOTS ( ( 4, 4 ),
 ( 2.449615925479262657, 2.486570309407579948 ),
 .UNSPECIFIED. ) 
 CURVE ( )  GEOMETRIC_REPRESENTATION_ITEM ( )  RATIONAL_B_SPLINE_CURVE ( ( 1.000000000000000000, 0.9998862010300719749, 0.9998862010300719749, 1.000000000000000000 ) ) 
 REPRESENTATION_ITEM ( '' )  );
#66593 = CARTESIAN_POINT ( 'NONE',  ( 21.75937500061451502, 0.000000000000000000, 5.243569643749999010 ) ) ;
#66594 = CARTESIAN_POINT ( 'NONE',  ( 14.14687500061451431, -4.119189519843965641, -2.378215178125001383 ) ) ;
#66595 = CARTESIAN_POINT ( 'NONE',  ( 7.190625000614518036, 6.054752690667223547, 3.707466751127219781E-16 ) ) ;
#66596 = CARTESIAN_POINT ( 'NONE',  ( 12.27187500061451786, 3.027376345333611329, 5.243569643749999010 ) ) ;
#66597 = ORIENTED_EDGE ( 'NONE', *, *, #29725, .T. ) ;
#66598 = CARTESIAN_POINT ( 'NONE',  ( 24.94687500061451502, -3.027376345333614438, 5.243569643749998122 ) ) ;
#66599 = DIRECTION ( 'NONE',  ( 0.000000000000000000, 0.000000000000000000, 1.000000000000000000 ) ) ;
#66600 = EDGE_CURVE ( 'NONE', #25555, #17152, #71683, .T. ) ;
#66601 = EDGE_CURVE ( 'NONE', #14829, #39133, #20100, .T. ) ;
#66602 = CARTESIAN_POINT ( 'NONE',  ( 8.662499999999999645, 2.886751345948129099, -4.999999999999997335 ) ) ;
#66603 = CARTESIAN_POINT ( 'NONE',  ( 4.425000000000001599, -4.330127018922194537, 2.499999999999995559 ) ) ;
#66604 = CARTESIAN_POINT ( 'NONE',  ( 14.21250000122903323, 4.330127018922192761, -2.499999999999997780 ) ) ;
#66605 = CARTESIAN_POINT ( 'NONE',  ( 17.32499999999999929, 4.330127018922191873, 2.499999999999999556 ) ) ;
#66606 = ORIENTED_EDGE ( 'NONE', *, *, #53813, .T. ) ;
#66607 = CARTESIAN_POINT ( 'NONE',  ( 12.26249999999999929, 2.886751345948129099, -4.999999999999998224 ) ) ;
#66608 = CARTESIAN_POINT ( 'NONE',  ( 17.32499999999999929, 4.330127018922191873, 2.499999999999999556 ) ) ;
#66609 = CARTESIAN_POINT ( 'NONE',  ( 13.80000000122903181, 5.773502691896255534, 3.535250795749688894E-16 ) ) ;
#66610 = CARTESIAN_POINT ( 'NONE',  ( 12.10312500061451857, 4.541064518000418104, -2.621784821874998173 ) ) ;
#66611 = EDGE_LOOP ( 'NONE', ( #44464, #920, #55020, #20464 ) ) ;
#66612 = CARTESIAN_POINT ( 'NONE',  ( 9.637499999999999289, 5.773502691896255534, 3.535250795749688894E-16 ) ) ;
#66613 = CARTESIAN_POINT ( 'NONE',  ( 16.83750000122903145, 6.123233995736764310E-16, -4.999999999999998224 ) ) ;
#66614 = CARTESIAN_POINT ( 'NONE',  ( -2.121784821874996840, 14.08437500061451786, -26.32496088578401583 ) ) ;
#66615 = CARTESIAN_POINT ( 'NONE',  ( 3.365625000614516082, -6.054752690667223547, -1.112240025338166033E-15 ) ) ;
#66616 = CARTESIAN_POINT ( 'NONE',  ( -3.756430356249999214, 15.07812499938548356, 27.83122392262697176 ) ) ;
#66617 = CARTESIAN_POINT ( 'NONE',  ( 8.812500000000000000, 2.886751345948126879, 4.999999999999999112 ) ) ;
#66618 = DIRECTION ( 'NONE',  ( 0.000000000000000000, 0.000000000000000000, -1.000000000000000000 ) ) ;
#66619 = ORIENTED_EDGE ( 'NONE', *, *, #12168, .T. ) ;
#66620 = CARTESIAN_POINT ( 'NONE',  ( 24.29062500061451502, 6.054752690667223547, 3.707466751127219781E-16 ) ) ;
#66621 = CARTESIAN_POINT ( 'NONE',  ( 29.40000000122903501, -2.886751345948115777, -5.000000000000017764 ) ) ;
#66622 = CARTESIAN_POINT ( 'NONE',  ( 1.878215178125000495, 20.36562499938548143, 26.74683588394047007 ) ) ;
#66623 = CARTESIAN_POINT ( 'NONE',  ( 21.08437500061451786, 6.421520780324663323E-16, -5.243569643749999010 ) ) ;
#66624 = CARTESIAN_POINT ( 'NONE',  ( 18.59062500061451573, -3.027376345333614438, 5.243569643749998122 ) ) ;
#66625 = CARTESIAN_POINT ( 'NONE',  ( -2.121784821874996840, 12.67812500061459424, -26.32496088578401583 ) ) ;
#66626 = CARTESIAN_POINT ( 'NONE',  ( 7.490625000614516082, -3.027376345333610441, -5.243569643749999898 ) ) ;
#66627 = CARTESIAN_POINT ( 'NONE',  ( 3.815625000614518036, -6.054752690667223547, -1.112240025338166033E-15 ) ) ;
#66628 = CARTESIAN_POINT ( 'NONE',  ( 25.24687500061451573, 5.492252693125287522, 3.363034840372157021E-16 ) ) ;
#66629 = CARTESIAN_POINT ( 'NONE',  ( 18.70312500061451644, -4.541064518000417216, -2.621784821875001281 ) ) ;
#66630 = FACE_OUTER_BOUND ( 'NONE', #37602, .T. ) ;
#66631 = CARTESIAN_POINT ( 'NONE',  ( 1.878215178125000495, 17.66562499938548214, 26.74683588394047007 ) ) ;
#66632 = CARTESIAN_POINT ( 'NONE',  ( 15.23437500061451644, 6.421520780324663323E-16, -5.243569643749999010 ) ) ;
#66633 = CARTESIAN_POINT ( 'NONE',  ( 15.45937500061451608, 0.000000000000000000, 5.243569643749999010 ) ) ;
#66634 = CARTESIAN_POINT ( 'NONE',  ( 21.94687500061451857, -3.027376345333610441, -5.243569643749999898 ) ) ;
#66635 = VERTEX_POINT ( 'NONE', #42657 ) ;
#66636 = CARTESIAN_POINT ( 'NONE',  ( 9.001249775931846008E-16, 12.77187500061451786, 34.90005215228797653 ) ) ;
#66637 = CARTESIAN_POINT ( 'NONE',  ( 3.665625000614517681, 3.027376345333611329, 5.243569643749999010 ) ) ;
#66638 = CARTESIAN_POINT ( 'NONE',  ( 26.20312500061451644, 0.000000000000000000, 5.243569643749999010 ) ) ;
#66639 = AXIS2_PLACEMENT_3D ( 'NONE', #32150, #44345, #4454 ) ;
#66640 = CARTESIAN_POINT ( 'NONE',  ( 25.60312500061451502, 4.541064518000418104, -2.621784821874998173 ) ) ;
#66641 = CARTESIAN_POINT ( 'NONE',  ( 4.000000000000000000, 15.19999999999999929, 30.00000000000000000 ) ) ;
#66642 = CARTESIAN_POINT ( 'NONE',  ( -2.828200636599751609E-16, 18.98749999999999716, 25.38119784648299770 ) ) ;
#66643 = CARTESIAN_POINT ( 'NONE',  ( 5.184375000614516615, -4.541064518000419881, 2.621784821874995952 ) ) ;
#66644 = DIRECTION ( 'NONE',  ( 0.000000000000000000, 0.000000000000000000, 1.000000000000000000 ) ) ;
#66645 = CARTESIAN_POINT ( 'NONE',  ( 11.40000000122903501, -2.886751345948125991, -5.000000000000000000 ) ) ;
#66646 = CARTESIAN_POINT ( 'NONE',  ( 9.300000001229035362, 5.773502691896255534, 3.535250795749688894E-16 ) ) ;
#66647 = CARTESIAN_POINT ( 'NONE',  ( 3.178125000614515638, 4.541064518000418104, 2.621784821874999949 ) ) ;
#66648 = CARTESIAN_POINT ( 'NONE',  ( 2.000000000000000444, 17.01874999877096428, 26.53589838486224650 ) ) ;
#66649 = CARTESIAN_POINT ( 'NONE',  ( 17.68125000122903501, 6.123233995736764310E-16, -4.999999999999998224 ) ) ;
#66650 = CARTESIAN_POINT ( 'NONE',  ( 12.30937500061451573, 0.000000000000000000, 5.243569643749999010 ) ) ;
#66651 = CARTESIAN_POINT ( 'NONE',  ( 4.000000000000000000, 14.78750000000000142, -27.69059892324149885 ) ) ;
#66652 = EDGE_LOOP ( 'NONE', ( #58210, #44419, #64768, #48525 ) ) ;
#66653 = CARTESIAN_POINT ( 'NONE',  ( 18.62812500061451715, -4.541064518000419881, 2.621784821874995952 ) ) ;
#66654 = CARTESIAN_POINT ( 'NONE',  ( 12.42187500061451821, -6.054752690667223547, -1.112240025338166033E-15 ) ) ;
#66655 = CARTESIAN_POINT ( 'NONE',  ( 5.540625000614515905, -3.027376345333614438, 5.243569643749998122 ) ) ;
#66656 = CARTESIAN_POINT ( 'NONE',  ( 22.50937500061451857, 4.541064518000418104, -2.621784821874998173 ) ) ;
#66657 = CARTESIAN_POINT ( 'NONE',  ( 5.765625000614519102, 3.027376345333613106, -5.243569643749998122 ) ) ;
#66658 = CARTESIAN_POINT ( 'NONE',  ( 0.000000000000000000, 20.00000000000000000, -30.00000000000000000 ) ) ;
#66659 = CARTESIAN_POINT ( 'NONE',  ( 6.487500001229034474, 6.123233995736764310E-16, -4.999999999999998224 ) ) ;
#66660 = CARTESIAN_POINT ( 'NONE',  ( 22.56562500061451715, 3.027376345333611329, 5.243569643749999010 ) ) ;
#66661 = CARTESIAN_POINT ( 'NONE',  ( 2.000000000000001332, 18.91250000122903430, -26.53589838486224650 ) ) ;
#66662 = CARTESIAN_POINT ( 'NONE',  ( 8.887500001229033941, 4.330127018922191873, 2.499999999999999556 ) ) ;
#66663 = CARTESIAN_POINT ( 'NONE',  ( 18.21562500061451573, -6.054752690667223547, -1.112240025338166033E-15 ) ) ;
#66664 = CARTESIAN_POINT ( 'NONE',  ( 16.22812500061451857, 4.541064518000418104, 2.621784821874999949 ) ) ;
#66665 = CARTESIAN_POINT ( 'NONE',  ( 25.77187500061451075, 2.746126346562643317, 4.756430356249998326 ) ) ;
#66666 = CARTESIAN_POINT ( 'NONE',  ( 14.92500000000000071, 6.123233995736764310E-16, -4.999999999999998224 ) ) ;
#66667 = CARTESIAN_POINT ( 'NONE',  ( 10.98750000122903536, 6.123233995736764310E-16, -4.999999999999998224 ) ) ;
#66668 = CARTESIAN_POINT ( 'NONE',  ( 7.265625000614516438, 3.027376345333611329, 5.243569643749999010 ) ) ;
#66669 = CARTESIAN_POINT ( 'NONE',  ( 10.90312500061451928, 0.000000000000000000, 5.243569643749999010 ) ) ;
#66670 = ADVANCED_FACE ( 'NONE', ( #19002 ), #25289, .F. ) ;
#66671 = CARTESIAN_POINT ( 'NONE',  ( 19.68750000122903288, 4.330127018922191873, 2.499999999999999556 ) ) ;
#66672 = AXIS2_PLACEMENT_3D ( 'NONE', #30187, #27574, #60072 ) ;
#66673 = CARTESIAN_POINT ( 'NONE',  ( -4.243569643749999898, 14.45937500061451964, -30.00000000000000000 ) ) ;
#66674 = CARTESIAN_POINT ( 'NONE',  ( 20.18437500061451573, 6.421520780324663323E-16, -5.243569643749999010 ) ) ;
#66675 = DIRECTION ( 'NONE',  ( -1.000000000000000000, -0.000000000000000000, -0.000000000000000000 ) ) ;
#66676 = CARTESIAN_POINT ( 'NONE',  ( 6.375000001229031987, -5.773502691896255534, -1.060575238724906372E-15 ) ) ;
#66677 = VECTOR ( 'NONE', #44904, 1000.000000000000000 ) ;
#66678 = CARTESIAN_POINT ( 'NONE',  ( 3.009375000614516793, -4.541064518000417216, -2.621784821875001281 ) ) ;
#66679 = CARTESIAN_POINT ( 'NONE',  ( 20.59687500061451360, -3.027376345333610441, -5.243569643749999898 ) ) ;
#66680 = CARTESIAN_POINT ( 'NONE',  ( 8.699999999999999289, 4.330127018922192761, -2.499999999999997780 ) ) ;
#66681 = CARTESIAN_POINT ( 'NONE',  ( 17.42812500061451786, 6.421520780324663323E-16, -5.243569643749999010 ) ) ;
#66682 = CARTESIAN_POINT ( 'NONE',  ( 12.05625000122903145, 0.000000000000000000, 4.999999999999998224 ) ) ;
#66683 = CARTESIAN_POINT ( 'NONE',  ( -3.999999999999999112, 14.71250000122903501, 30.00000000000000000 ) ) ;
#66684 = CARTESIAN_POINT ( 'NONE',  ( -2.000000000000000000, 15.42500000000000071, 26.53589838486224650 ) ) ;
#66685 = CARTESIAN_POINT ( 'NONE',  ( 28.92187500061451644, 3.027376345333611329, 5.243569643749999010 ) ) ;
#66686 = CARTESIAN_POINT ( 'NONE',  ( 20.89687500061451786, -4.119189519843965641, -2.378215178125001383 ) ) ;
#66687 = CARTESIAN_POINT ( 'NONE',  ( 14.65312500061451573, -4.541064518000417216, -2.621784821875001281 ) ) ;
#66688 = CIRCLE ( 'NONE', #63134, 9.999999999999998224 ) ;
#66689 = CARTESIAN_POINT ( 'NONE',  ( 12.94687500061451857, -3.027376345333610441, -5.243569643749999898 ) ) ;
#66690 = ORIENTED_EDGE ( 'NONE', *, *, #67682, .F. ) ;
#66691 = CARTESIAN_POINT ( 'NONE',  ( 22.34999999999999787, 0.000000000000000000, 4.999999999999998224 ) ) ;
#66692 = CARTESIAN_POINT ( 'NONE',  ( 22.97812500061451857, 4.541064518000418104, 2.621784821874999949 ) ) ;
#66693 = CARTESIAN_POINT ( 'NONE',  ( 2.000000000000001332, 11.15000000000000213, -26.53589838486224650 ) ) ;
#66694 = ADVANCED_FACE ( 'NONE', ( #19743 ), #65181, .F. ) ;
#66695 = CARTESIAN_POINT ( 'NONE',  ( 1.626862140677534273E-15, 18.42500000122903359, 34.00000000000000000 ) ) ;
#66696 = CARTESIAN_POINT ( 'NONE',  ( 13.38750000000000107, -2.886751345948129988, 4.999999999999997335 ) ) ;
#66697 = CARTESIAN_POINT ( 'NONE',  ( 24.52500000122903145, 2.886751345948129099, -4.999999999999998224 ) ) ;
#66698 = CARTESIAN_POINT ( 'NONE',  ( 19.22812500061451502, 6.421520780324663323E-16, -5.243569643749999010 ) ) ;
#66699 = CARTESIAN_POINT ( 'NONE',  ( 13.58437500061451431, -2.746126346562646425, 4.756430356249996549 ) ) ;
#66700 = ORIENTED_EDGE ( 'NONE', *, *, #9386, .T. ) ;
#66701 = CARTESIAN_POINT ( 'NONE',  ( 21.15000000000000213, -4.330127018922190985, -2.500000000000001332 ) ) ;
#66702 = CARTESIAN_POINT ( 'NONE',  ( 20.40937500061451715, 0.000000000000000000, 5.243569643749999010 ) ) ;
#66703 = CARTESIAN_POINT ( 'NONE',  ( 27.96562500061451928, 3.027376345333611329, 5.243569643749999010 ) ) ;
#66704 = VERTEX_POINT ( 'NONE', #35648 ) ;
#66705 = CARTESIAN_POINT ( 'NONE',  ( 1.071796769724493892, 18.06740381056766864, -34.00000000000000000 ) ) ;
#66706 = CARTESIAN_POINT ( 'NONE',  ( 11.80312500061451608, 0.000000000000000000, 5.243569643749999010 ) ) ;
#66707 = CARTESIAN_POINT ( 'NONE',  ( 17.47500000122903430, 2.886751345948193936, 4.999999999999883649 ) ) ;
#66708 = CARTESIAN_POINT ( 'NONE',  ( 14.59687500061451537, -4.119189519843965641, -2.378215178125001383 ) ) ;
#66709 = CARTESIAN_POINT ( 'NONE',  ( 15.90000000000000036, 4.330127018922192761, -2.499999999999997780 ) ) ;
#66710 = CARTESIAN_POINT ( 'NONE',  ( 24.75000000000000000, -4.330127018922190985, -2.500000000000001332 ) ) ;
#66711 = LINE ( 'NONE', #32350, #58043 ) ;
#66712 = CARTESIAN_POINT ( 'NONE',  ( 5.371875000614516615, 3.027376345333613106, -5.243569643749998122 ) ) ;
#66713 = CARTESIAN_POINT ( 'NONE',  ( 27.79687500061451999, -3.027376345333610441, -5.243569643749999898 ) ) ;
#66714 = ORIENTED_EDGE ( 'NONE', *, *, #2252, .F. ) ;
#66715 = CARTESIAN_POINT ( 'NONE',  ( 25.22812500061451502, 4.541064518000418104, 2.621784821874999949 ) ) ;
#66716 = CARTESIAN_POINT ( 'NONE',  ( 27.53437500061451360, 4.541064518000418104, 2.621784821874999949 ) ) ;
#66718 = EDGE_CURVE ( 'NONE', #47560, #17531, #64816, .T. ) ;
#66717 = CARTESIAN_POINT ( 'NONE',  ( 30.00000000000000000, 0.000000000000000000, 4.999999999999998224 ) ) ;
#66719 = CARTESIAN_POINT ( 'NONE',  ( 12.71250000000000036, 2.886751345948129099, -4.999999999999998224 ) ) ;
#66720 = CARTESIAN_POINT ( 'NONE',  ( 11.84062500061451750, -3.027376345333614438, 5.243569643749998122 ) ) ;
#66721 = CARTESIAN_POINT ( 'NONE',  ( -5.810221930991193690E-16, 14.60000000122903252, -34.00000000000000000 ) ) ;
#66722 = CARTESIAN_POINT ( 'NONE',  ( 0.000000000000000000, 20.00000000000000000, 30.00000000000000000 ) ) ;
#66723 = CARTESIAN_POINT ( 'NONE',  ( 27.62812500061451360, -4.541064518000419881, 2.621784821874995952 ) ) ;
#66724 = CARTESIAN_POINT ( 'NONE',  ( 16.57500000122903216, 2.886751345948126879, 4.999999999999999112 ) ) ;
#66725 = CARTESIAN_POINT ( 'NONE',  ( 28.92187500061451644, -4.119189519843968306, 2.378215178124996054 ) ) ;
#66726 = CARTESIAN_POINT ( 'NONE',  ( 15.15937500061451715, -4.119189519843965641, -2.378215178125001383 ) ) ;
#66727 = CARTESIAN_POINT ( 'NONE',  ( 4.340625000614515727, -3.027376345333610441, -5.243569643749999898 ) ) ;
#66728 = CARTESIAN_POINT ( 'NONE',  ( 22.24687500061451217, -3.027376345333614438, 5.243569643749998122 ) ) ;
#66729 = CARTESIAN_POINT ( 'NONE',  ( 9.001249775931846008E-16, 14.12187500061451750, 34.90005215228797653 ) ) ;
#66730 = CARTESIAN_POINT ( 'NONE',  ( 21.53437500061451715, 6.421520780324663323E-16, -5.243569643749999010 ) ) ;
#66731 = CARTESIAN_POINT ( 'NONE',  ( 28.69687500061451502, -3.027376345333610441, -5.243569643749999898 ) ) ;
#66732 = CARTESIAN_POINT ( 'NONE',  ( 2.121784821875001281, 19.10937500061451644, 33.67503911421598417 ) ) ;
#66733 = CARTESIAN_POINT ( 'NONE',  ( 9.965625000614517504, 3.027376345333611329, 5.243569643749999010 ) ) ;
#66734 = CARTESIAN_POINT ( 'NONE',  ( 2.887500001229035274, 6.123233995736764310E-16, -4.999999999999998224 ) ) ;
#66735 = CARTESIAN_POINT ( 'NONE',  ( 6.459375000614518747, 0.000000000000000000, 5.243569643749999010 ) ) ;
#66736 = PLANE ( 'NONE',  #34799 ) ;
#66737 = VECTOR ( 'NONE', #32383, 1000.000000000000000 ) ;
#66738 = CARTESIAN_POINT ( 'NONE',  ( 7.865625000614516971, -6.054752690667223547, -1.112240025338166033E-15 ) ) ;
#66739 = CARTESIAN_POINT ( 'NONE',  ( 12.19687500061451679, 6.054752690667223547, 3.707466751127219781E-16 ) ) ;
#66740 = FACE_OUTER_BOUND ( 'NONE', #14283, .T. ) ;
#66741 = CARTESIAN_POINT ( 'NONE',  ( 21.90000000122903145, 5.773502691896255534, 3.535250795749688894E-16 ) ) ;
#66742 = CARTESIAN_POINT ( 'NONE',  ( 7.434375000614519280, -4.541064518000419881, 2.621784821874995952 ) ) ;
#66743 = CARTESIAN_POINT ( 'NONE',  ( 10.52812500061451750, -4.541064518000419881, 2.621784821874995952 ) ) ;
#66744 = CARTESIAN_POINT ( 'NONE',  ( 7.378125000614518036, -4.541064518000419881, 2.621784821874995952 ) ) ;
#66745 = CARTESIAN_POINT ( 'NONE',  ( 25.18125000122903145, -4.330127018922194537, 2.499999999999995559 ) ) ;
#66746 = CARTESIAN_POINT ( 'NONE',  ( 20.29687500061451644, 6.054752690667223547, 3.707466751127219781E-16 ) ) ;
#66747 = CARTESIAN_POINT ( 'NONE',  ( 18.14999999999999858, 4.330127018922192761, -2.499999999999997780 ) ) ;
#66748 = CARTESIAN_POINT ( 'NONE',  ( 11.91562500061451857, -6.054752690667223547, -1.112240025338166033E-15 ) ) ;
#66749 = CARTESIAN_POINT ( 'NONE',  ( 28.69687500061451502, -3.027376345333610441, -5.243569643749999898 ) ) ;
#66750 = CARTESIAN_POINT ( 'NONE',  ( 4.243569643749999898, 11.94687500061451857, -27.54997392385601529 ) ) ;
#66751 = CARTESIAN_POINT ( 'NONE',  ( 15.15000000122903323, 5.773502691896255534, 3.535250795749688894E-16 ) ) ;
#66752 = AXIS2_PLACEMENT_3D ( 'NONE', #23612, #58306, #19512 ) ;
#66753 = CARTESIAN_POINT ( 'NONE',  ( 2.121784821874999061, 16.05312500061451786, -33.67503911421598417 ) ) ;
#66754 = CARTESIAN_POINT ( 'NONE',  ( 15.37500000122903465, -5.773502691896255534, -1.060575238724906372E-15 ) ) ;
#66755 = CARTESIAN_POINT ( 'NONE',  ( 9.928125000614517859, 4.541064518000418104, 2.621784821874999949 ) ) ;
#66756 = VERTEX_POINT ( 'NONE', #14206 ) ;
#66757 = CARTESIAN_POINT ( 'NONE',  ( 13.31250000000000178, 2.886751345948126879, 4.999999999999999112 ) ) ;
#66758 = CARTESIAN_POINT ( 'NONE',  ( 13.81875000122903074, 2.886751345948238789, 4.999999999999807265 ) ) ;
#66759 = CARTESIAN_POINT ( 'NONE',  ( 23.20312500061451644, -4.541064518000417216, -2.621784821875001281 ) ) ;
#66760 = CARTESIAN_POINT ( 'NONE',  ( 8.109375000614518214, 4.541064518000418104, -2.621784821874998173 ) ) ;
#66761 = CARTESIAN_POINT ( 'NONE',  ( 10.76250000122903572, 0.000000000000000000, 4.999999999999998224 ) ) ;
#66762 = CARTESIAN_POINT ( 'NONE',  ( 18.90000000122902790, -2.886751345948129988, 4.999999999999997335 ) ) ;
#66763 = CARTESIAN_POINT ( 'NONE',  ( 16.37812500061451715, -4.541064518000419881, 2.621784821874995952 ) ) ;
#66764 = CARTESIAN_POINT ( 'NONE',  ( 19.00312500061451715, 0.000000000000000000, 5.243569643749999010 ) ) ;
#66765 = CARTESIAN_POINT ( 'NONE',  ( 25.38750000122903216, 6.123233995736764310E-16, -4.999999999999998224 ) ) ;
#66766 = CARTESIAN_POINT ( 'NONE',  ( 29.06250000122903288, 4.330127018922192761, -2.499999999999997780 ) ) ;
#66767 = CARTESIAN_POINT ( 'NONE',  ( 23.47499999999999787, 6.123233995736764310E-16, -4.999999999999998224 ) ) ;
#66768 = CARTESIAN_POINT ( 'NONE',  ( -1.878215178125001827, 14.29062499938548392, 33.25316411605952283 ) ) ;
#66769 = CARTESIAN_POINT ( 'NONE',  ( 26.48437500061451644, 6.421520780324663323E-16, -5.243569643749999010 ) ) ;
#66770 = FACE_OUTER_BOUND ( 'NONE', #51440, .T. ) ;
#66771 = CARTESIAN_POINT ( 'NONE',  ( 13.38750000122903394, 4.330127018922191873, 2.499999999999999556 ) ) ;
#66772 = CARTESIAN_POINT ( 'NONE',  ( 28.95937500061451431, 0.000000000000000000, 5.243569643749999010 ) ) ;
#66773 = EDGE_CURVE ( 'NONE', #71220, #60301, #71393, .T. ) ;
#66774 = DIRECTION ( 'NONE',  ( 1.000000000000000000, 0.000000000000000000, 0.000000000000000000 ) ) ;
#66775 = CARTESIAN_POINT ( 'NONE',  ( 4.321875000614517681, -6.054752690667223547, -1.112240025338166033E-15 ) ) ;
#66776 = CARTESIAN_POINT ( 'NONE',  ( 25.22812500061451502, 4.541064518000418104, 2.621784821874999949 ) ) ;
#66777 = CARTESIAN_POINT ( 'NONE',  ( -7.967954043666661671E-16, 14.89062499938548179, 34.33755215474603517 ) ) ;
#66778 = CARTESIAN_POINT ( 'NONE',  ( -4.000000000000000888, 15.40624999877096535, 32.30940107675850470 ) ) ;
#66779 = CARTESIAN_POINT ( 'NONE',  ( 10.13437500061451679, -4.541064518000419881, 2.621784821874995952 ) ) ;
#66780 = DIRECTION ( 'NONE',  ( -1.000000000000000000, -0.000000000000000000, -0.000000000000000000 ) ) ;
#66781 = CARTESIAN_POINT ( 'NONE',  ( 3.909375000614518481, -4.541064518000417216, -2.621784821875001281 ) ) ;
#66782 = CARTESIAN_POINT ( 'NONE',  ( 5.521875000614517859, 3.027376345333611329, 5.243569643749999010 ) ) ;
#66783 = CARTESIAN_POINT ( 'NONE',  ( 27.79687500061451999, -3.027376345333610441, -5.243569643749999898 ) ) ;
#66784 = CARTESIAN_POINT ( 'NONE',  ( -2.121784821874996840, 10.42812500061459424, 33.67503911421598417 ) ) ;
#66785 = CARTESIAN_POINT ( 'NONE',  ( 19.20000000000000284, 0.000000000000000000, 4.999999999999998224 ) ) ;
#66786 =( REPRESENTATION_RELATIONSHIP ('NONE','NONE', #33485, #46217 ) REPRESENTATION_RELATIONSHIP_WITH_TRANSFORMATION ( #27856 )SHAPE_REPRESENTATION_RELATIONSHIP( ) );
#66787 = VERTEX_POINT ( 'NONE', #36742 ) ;
#66788 = CARTESIAN_POINT ( 'NONE',  ( 28.64999999999999858, 0.000000000000000000, 4.999999999999998224 ) ) ;
#66789 =( BOUNDED_CURVE ( )  B_SPLINE_CURVE ( 2, ( #3631, #27260, #31699, #66043, #54234, #53872, #71958, #21334, #8796 ),
 .UNSPECIFIED., .F., .F. ) 
 B_SPLINE_CURVE_WITH_KNOTS ( ( 3, 2, 2, 2, 3 ),
 ( 0.2065217391304347838, 0.2101449275362318736, 0.2173913043478260809, 0.2246376811594202882, 0.2282608695652174058 ),
 .UNSPECIFIED. ) 
 CURVE ( )  GEOMETRIC_REPRESENTATION_ITEM ( )  RATIONAL_B_SPLINE_CURVE ( ( 0.9330127018922194093, 0.9330127018922194093, 1.000000000000000000, 0.8660254037844387076, 1.000000000000000000, 0.8660254037844387076, 1.000000000000000000, 0.9330127018922190762, 0.9330127018922194093 ) ) 
 REPRESENTATION_ITEM ( '' )  );
#66790 = CARTESIAN_POINT ( 'NONE',  ( 28.95937500061451431, 0.000000000000000000, 5.243569643749999010 ) ) ;
#66791 = VERTEX_POINT ( 'NONE', #24923 ) ;
#66792 = CARTESIAN_POINT ( 'NONE',  ( 16.79062500061451857, -3.027376345333614438, 5.243569643749998122 ) ) ;
#66793 = CARTESIAN_POINT ( 'NONE',  ( 7.753125000614518036, 0.000000000000000000, 5.243569643749999010 ) ) ;
#66794 = CARTESIAN_POINT ( 'NONE',  ( 21.68437500061451573, -2.746126346562646425, 4.756430356249996549 ) ) ;
#66795 = CARTESIAN_POINT ( 'NONE',  ( 6.121875000614517504, -6.054752690667223547, -1.112240025338166033E-15 ) ) ;
#66796 = CARTESIAN_POINT ( 'NONE',  ( 17.92500000122903359, 2.886751345948126879, 4.999999999999999112 ) ) ;
#66797 = CARTESIAN_POINT ( 'NONE',  ( 4.000000000000000000, 19.70000000000000284, 30.00000000000000000 ) ) ;
#66798 = CARTESIAN_POINT ( 'NONE',  ( 5.934375000614517504, 4.541064518000418104, 2.621784821874999949 ) ) ;
#66799 = CARTESIAN_POINT ( 'NONE',  ( 11.33437500061451608, 4.541064518000418104, 2.621784821874999949 ) ) ;
#66800 = CARTESIAN_POINT ( 'NONE',  ( 23.03437500061451715, 4.541064518000418104, 2.621784821874999949 ) ) ;
#66801 = CARTESIAN_POINT ( 'NONE',  ( 1.592000809091587073E-14, 15.95000000122903394, -34.00000000000000000 ) ) ;
#66802 = EDGE_LOOP ( 'NONE', ( #30164, #43942, #5505, #22839 ) ) ;
#66803 = CARTESIAN_POINT ( 'NONE',  ( 9.712500000000002132, 2.886751345948126879, 4.999999999999999112 ) ) ;
#66804 = CARTESIAN_POINT ( 'NONE',  ( 16.92187500061451999, -6.054752690667223547, -1.112240025338166033E-15 ) ) ;
#66805 = CARTESIAN_POINT ( 'NONE',  ( 9.159375000614515372, 0.000000000000000000, 5.243569643749999010 ) ) ;
#66806 = CARTESIAN_POINT ( 'NONE',  ( 3.756430356250000546, 14.92812499938548321, 27.83122392262697886 ) ) ;
#66807 = CARTESIAN_POINT ( 'NONE',  ( 20.36249999999999716, 2.886751345948129099, -4.999999999999998224 ) ) ;
#66808 = CARTESIAN_POINT ( 'NONE',  ( 4.000000000000000000, 17.00000000000000000, 30.00000000000000000 ) ) ;
#66809 = CARTESIAN_POINT ( 'NONE',  ( -1.071796769724488563, 9.854903811796701163, -26.00000000000000000 ) ) ;
#66810 = CARTESIAN_POINT ( 'NONE',  ( 21.75937500061451502, 0.000000000000000000, 4.756430356249998326 ) ) ;
#66811 = CARTESIAN_POINT ( 'NONE',  ( 12.36562500061451608, -6.054752690667223547, -1.112240025338166033E-15 ) ) ;
#66812 = CARTESIAN_POINT ( 'NONE',  ( 28.05937500061451573, 0.000000000000000000, 5.243569643749999010 ) ) ;
#66813 = CARTESIAN_POINT ( 'NONE',  ( 28.50937500061451502, 0.000000000000000000, 5.243569643749999010 ) ) ;
#66814 = CARTESIAN_POINT ( 'NONE',  ( 10.16249999999999964, 2.886751345948126879, 4.999999999999999112 ) ) ;
#66815 = CARTESIAN_POINT ( 'NONE',  ( 2.000000000000001332, 15.31250000122903465, 33.46410161513774995 ) ) ;
#66816 = CARTESIAN_POINT ( 'NONE',  ( 9.750000001229032875, 5.773502691896255534, 3.535250795749688894E-16 ) ) ;
#66817 = CARTESIAN_POINT ( 'NONE',  ( 19.95937500061451786, 0.000000000000000000, 5.243569643749999010 ) ) ;
#66818 = CARTESIAN_POINT ( 'NONE',  ( 14.59687500061452070, -3.027376345333614438, 5.243569643749998122 ) ) ;
#66819 = CARTESIAN_POINT ( 'NONE',  ( 4.008114575609427632, 2.989161209909902972, -4.308132060747937864 ) ) ;
#66820 = VERTEX_POINT ( 'NONE', #64081 ) ;
#66821 = CARTESIAN_POINT ( 'NONE',  ( 16.97812500061451502, 6.421520780324663323E-16, -5.243569643749999010 ) ) ;
#66822 = CARTESIAN_POINT ( 'NONE',  ( 27.60000000122903430, -2.886751345948125991, -5.000000000000000000 ) ) ;
#66823 = CARTESIAN_POINT ( 'NONE',  ( 15.64687500061451608, -3.027376345333610441, -5.243569643749999898 ) ) ;
#66824 = CARTESIAN_POINT ( 'NONE',  ( 3.290625000614516793, -3.027376345333614438, 5.243569643749998122 ) ) ;
#66825 = CARTESIAN_POINT ( 'NONE',  ( 17.01562500061451644, 3.027376345333613106, -5.243569643749998122 ) ) ;
#66826 = CARTESIAN_POINT ( 'NONE',  ( -1.626862140677534273E-15, 19.98124999877096641, 34.00000000000000000 ) ) ;
#66827 = ADVANCED_FACE ( 'NONE', ( #36012 ), #31202, .F. ) ;
#66828 = CARTESIAN_POINT ( 'NONE',  ( 26.55937500061451573, 4.541064518000418104, -2.621784821874998173 ) ) ;
#66829 = CARTESIAN_POINT ( 'NONE',  ( 9.001249775931846008E-16, 13.16562500061451857, 34.90005215228797653 ) ) ;
#66830 = CARTESIAN_POINT ( 'NONE',  ( 14.85937500061451644, 4.541064518000418104, -2.621784821874998173 ) ) ;
#66831 = CARTESIAN_POINT ( 'NONE',  ( 15.07500000122903394, 2.886751345948129099, -4.999999999999998224 ) ) ;
#66832 = CARTESIAN_POINT ( 'NONE',  ( 9.496875000614517504, 5.492252693125287522, 3.363034840372157021E-16 ) ) ;
#66833 = EDGE_CURVE ( 'NONE', #72537, #27078, #14051, .T. ) ;
#66834 = CARTESIAN_POINT ( 'NONE',  ( -2.121784821874999949, 18.43437500061451928, -33.67503911421598417 ) ) ;
#66835 = CARTESIAN_POINT ( 'NONE',  ( 21.49687500061451573, -3.027376345333610441, -5.243569643749999898 ) ) ;
#66836 = CARTESIAN_POINT ( 'NONE',  ( 22.42500000122903359, 2.886751345948126879, 4.999999999999999112 ) ) ;
#66837 = CARTESIAN_POINT ( 'NONE',  ( 16.47187500061452070, -6.054752690667223547, -1.112240025338166033E-15 ) ) ;
#66838 = CARTESIAN_POINT ( 'NONE',  ( -4.243569643749999898, 11.72187500061451892, 27.54997392385601529 ) ) ;
#66839 = AXIS2_PLACEMENT_3D ( 'NONE', #49964, #9702, #72488 ) ;
#66840 = CARTESIAN_POINT ( 'NONE',  ( 17.20312500061451644, 0.000000000000000000, 5.243569643749999010 ) ) ;
#66841 = VERTEX_POINT ( 'NONE', #64451 ) ;
#66842 = ORIENTED_EDGE ( 'NONE', *, *, #51591, .F. ) ;
#66843 = CARTESIAN_POINT ( 'NONE',  ( 21.18749999999999645, -2.886751345948125991, -5.000000000000000000 ) ) ;
#66844 = LINE ( 'NONE', #38391, #12588 ) ;
#66845 = CARTESIAN_POINT ( 'NONE',  ( 24.89062500061451644, -3.027376345333614438, 5.243569643749998122 ) ) ;
#66846 = CARTESIAN_POINT ( 'NONE',  ( 5.165625000614518569, -6.054752690667223547, -1.112240025338166033E-15 ) ) ;
#66847 = CARTESIAN_POINT ( 'NONE',  ( 16.72500000122903430, -5.773502691896255534, -1.060575238724906372E-15 ) ) ;
#66848 = CARTESIAN_POINT ( 'NONE',  ( 22.04062500061451502, 6.054752690667223547, 3.707466751127219781E-16 ) ) ;
#66849 = CARTESIAN_POINT ( 'NONE',  ( 21.15000000000000213, -4.330127018922190985, -2.500000000000001332 ) ) ;
#66850 = CARTESIAN_POINT ( 'NONE',  ( 25.94062500061451715, -3.027376345333610441, -5.243569643749999898 ) ) ;
#66851 = CARTESIAN_POINT ( 'NONE',  ( 6.703125000614516438, 4.541064518000418104, -2.621784821874998173 ) ) ;
#66852 = EDGE_LOOP ( 'NONE', ( #18539, #4600, #17863, #65463 ) ) ;
#66853 = CARTESIAN_POINT ( 'NONE',  ( 3.390184931900214860, 3.675138926287994767, 3.390184931900133147 ) ) ;
#66854 = CARTESIAN_POINT ( 'NONE',  ( 17.28750000000000142, 5.773502691896255534, 3.535250795749688401E-16 ) ) ;
#66855 = CARTESIAN_POINT ( 'NONE',  ( 10.47187500061451715, 2.746126346562643317, 4.756430356249998326 ) ) ;
#66856 = CARTESIAN_POINT ( 'NONE',  ( 1.071796769724491893, 18.78259618943233278, 33.99999999999999289 ) ) ;
#66857 = CARTESIAN_POINT ( 'NONE',  ( 4.000000000000000000, 12.20000000122903394, -27.69059892324149530 ) ) ;
#66858 = CARTESIAN_POINT ( 'NONE',  ( -2.121784821874996840, 18.13437500061451502, -26.32496088578401583 ) ) ;
#66859 = EDGE_CURVE ( 'NONE', #34596, #10453, #21616, .T. ) ;
#66860 = CARTESIAN_POINT ( 'NONE',  ( 8.437500000000000000, -2.886751345948129988, 4.999999999999997335 ) ) ;
#66861 = CARTESIAN_POINT ( 'NONE',  ( 8.296875000614516438, -3.027376345333614438, 5.243569643749998122 ) ) ;
#66862 = CARTESIAN_POINT ( 'NONE',  ( 6.600000001229032520, 5.773502691896255534, 3.535250795749688894E-16 ) ) ;
#66863 = CARTESIAN_POINT ( 'NONE',  ( 12.00937500061451857, -4.541064518000417216, -2.621784821875001281 ) ) ;
#66864 = CARTESIAN_POINT ( 'NONE',  ( 3.421875000614516882, -6.054752690667223547, -1.112240025338166033E-15 ) ) ;
#66865 = CARTESIAN_POINT ( 'NONE',  ( 30.00000000000000000, 0.000000000000000000, 4.999999999999998224 ) ) ;
#66866 = AXIS2_PLACEMENT_3D ( 'NONE', #69435, #50363, #122 ) ;
#66867 = CARTESIAN_POINT ( 'NONE',  ( -0.6945831915928805111, 10.00052343484236950, 26.06076730949330411 ) ) ;
#66868 = CARTESIAN_POINT ( 'NONE',  ( 10.24687500061451750, -3.027376345333610441, -5.243569643749999898 ) ) ;
#66869 = DIRECTION ( 'NONE',  ( -0.000000000000000000, -1.000000000000000000, -0.000000000000000000 ) ) ;
#66870 = CARTESIAN_POINT ( 'NONE',  ( 19.86562500061451786, 3.027376345333611329, 5.243569643749999010 ) ) ;
#66871 = CARTESIAN_POINT ( 'NONE',  ( -3.137519842735245283E-14, 12.57500000122903572, -26.00000000000000711 ) ) ;
#66872 = CARTESIAN_POINT ( 'NONE',  ( -4.243569643749999898, 19.80312500061451786, 30.00000000000000000 ) ) ;
#66873 = CARTESIAN_POINT ( 'NONE',  ( 24.38437500061451502, 4.541064518000418104, 2.621784821874999949 ) ) ;
#66874 = CARTESIAN_POINT ( 'NONE',  ( 45.00000000000000000, 0.000000000000000000, 0.000000000000000000 ) ) ;
#66875 = CARTESIAN_POINT ( 'NONE',  ( 28.57500000122903572, 2.886751345948129099, -4.999999999999998224 ) ) ;
#66876 = CARTESIAN_POINT ( 'NONE',  ( 20.97187500061451715, 5.824947211148865298E-16, -4.756430356249998326 ) ) ;
#66877 = CARTESIAN_POINT ( 'NONE',  ( 25.75312500061451715, 0.000000000000000000, 5.243569643749999010 ) ) ;
#66878 = CARTESIAN_POINT ( 'NONE',  ( 14.99062500061451786, -3.027376345333614438, 5.243569643749998122 ) ) ;
#66879 = CARTESIAN_POINT ( 'NONE',  ( 14.75625000122903252, 0.000000000000000000, 4.999999999999998224 ) ) ;
#66880 = CARTESIAN_POINT ( 'NONE',  ( 13.54687500061451999, 6.054752690667223547, 3.707466751127219781E-16 ) ) ;
#66881 = DIRECTION ( 'NONE',  ( 1.000000000000000000, -0.000000000000000000, -0.000000000000000000 ) ) ;
#66882 = VECTOR ( 'NONE', #60848, 1000.000000000000000 ) ;
#66883 = CARTESIAN_POINT ( 'NONE',  ( 24.26250000122903216, 0.000000000000000000, 4.999999999999998224 ) ) ;
#66884 = CARTESIAN_POINT ( 'NONE',  ( 4.471875000614518925, 3.027376345333613106, -5.243569643749998122 ) ) ;
#66885 = CARTESIAN_POINT ( 'NONE',  ( 13.77187500061451786, -6.054752690667223547, -1.112240025338166033E-15 ) ) ;
#66886 = CARTESIAN_POINT ( 'NONE',  ( 4.859524668404109349, -1.177064389673172728, -5.109794524303713281 ) ) ;
#66887 = CARTESIAN_POINT ( 'NONE',  ( 0.000000000000000000, 12.50000000000000000, 30.00000000000000000 ) ) ;
#66888 = CARTESIAN_POINT ( 'NONE',  ( 16.68750000122903288, -4.330127018922194537, 2.499999999999995559 ) ) ;
#66889 = CARTESIAN_POINT ( 'NONE',  ( 23.97187500061451360, 3.027376345333611329, 5.243569643749999010 ) ) ;
#66890 = CARTESIAN_POINT ( 'NONE',  ( 15.94687500061451502, -3.027376345333614438, 5.243569643749998122 ) ) ;
#66891 = CARTESIAN_POINT ( 'NONE',  ( -3.756430356250001434, 15.71562499938548108, 32.16877607737301048 ) ) ;
#66892 = CARTESIAN_POINT ( 'NONE',  ( 28.68749999999999645, -2.886751345948129988, 4.999999999999997335 ) ) ;
#66893 = CARTESIAN_POINT ( 'NONE',  ( 2.662500001229036073, 0.000000000000000000, 4.999999999999998224 ) ) ;
#66894 = CARTESIAN_POINT ( 'NONE',  ( 4.575000000000002842, 6.123233995736764310E-16, -4.999999999999998224 ) ) ;
#66895 = CARTESIAN_POINT ( 'NONE',  ( 29.59687500061451715, -2.746126346562642428, -4.756430356249999214 ) ) ;
#66896 = CARTESIAN_POINT ( 'NONE',  ( 19.67812500061451786, 6.421520780324663323E-16, -5.243569643749999010 ) ) ;
#66897 = CARTESIAN_POINT ( 'NONE',  ( 9.899999999999998579, -4.330127018922190985, -2.500000000000001332 ) ) ;
#66898 = CARTESIAN_POINT ( 'NONE',  ( 4.340625000614515727, -3.027376345333610441, -5.243569643749999898 ) ) ;
#66899 = CARTESIAN_POINT ( 'NONE',  ( 17.13749999999999929, -2.886751345948125991, -5.000000000000000000 ) ) ;
#66900 = CARTESIAN_POINT ( 'NONE',  ( 2.417052323292336544E-14, 20.48749999999999716, 34.00000000000000000 ) ) ;
#66901 = CARTESIAN_POINT ( 'NONE',  ( 20.96250000122903145, 4.330127018922192761, -2.499999999999997780 ) ) ;
#66902 = CARTESIAN_POINT ( 'NONE',  ( 28.31250000122903288, 0.000000000000000000, 4.999999999999998224 ) ) ;
#66903 = CARTESIAN_POINT ( 'NONE',  ( 27.87187500061451573, 3.027376345333613106, -5.243569643749998122 ) ) ;
#66904 = VERTEX_POINT ( 'NONE', #3874 ) ;
#66905 = CARTESIAN_POINT ( 'NONE',  ( 16.15312500061451573, 4.541064518000418104, -2.621784821874998173 ) ) ;
#66906 = CARTESIAN_POINT ( 'NONE',  ( 25.11562500061451431, 3.027376345333613106, -5.243569643749998122 ) ) ;
#66907 = CARTESIAN_POINT ( 'NONE',  ( 22.47187500061451715, 3.027376345333613106, -5.243569643749998122 ) ) ;
#66908 = CARTESIAN_POINT ( 'NONE',  ( 6.975000000000002309, 4.330127018922191873, 2.499999999999999556 ) ) ;
#66909 = CARTESIAN_POINT ( 'NONE',  ( 9.328125000614518214, 6.421520780324663323E-16, -5.243569643749999010 ) ) ;
#66910 = CARTESIAN_POINT ( 'NONE',  ( 23.09062500061451573, -3.027376345333614438, 5.243569643749998122 ) ) ;
#66911 = CARTESIAN_POINT ( 'NONE',  ( 15.79687500061451821, 6.054752690667223547, 3.707466751127219781E-16 ) ) ;
#66912 = CARTESIAN_POINT ( 'NONE',  ( 18.72187500061451360, -6.054752690667223547, -1.112240025338166033E-15 ) ) ;
#66913 = CARTESIAN_POINT ( 'NONE',  ( 4.432080220173729046, 2.314473833018743321, -4.705141300289269246 ) ) ;
#66914 = CARTESIAN_POINT ( 'NONE',  ( -2.121784821874996840, 10.93437500061451928, 33.67503911421598417 ) ) ;
#66915 = CARTESIAN_POINT ( 'NONE',  ( 21.33750000122903145, 6.123233995736764310E-16, -4.999999999999998224 ) ) ;
#66916 = CARTESIAN_POINT ( 'NONE',  ( 17.40937500061451715, -4.119189519843965641, -2.378215178125001383 ) ) ;
#66917 = CARTESIAN_POINT ( 'NONE',  ( 12.29062500061451857, -3.027376345333614438, 5.243569643749998122 ) ) ;
#66918 = CARTESIAN_POINT ( 'NONE',  ( 8.109375000614518214, 4.541064518000418104, -2.621784821874998173 ) ) ;
#66919 = CARTESIAN_POINT ( 'NONE',  ( 6.684375000614518392, 6.421520780324663323E-16, -5.243569643749999010 ) ) ;
#66920 = EDGE_LOOP ( 'NONE', ( #62431, #51485, #32649, #48387 ) ) ;
#66921 = EDGE_CURVE ( 'NONE', #62090, #16892, #26373, .T. ) ;
#66922 = CARTESIAN_POINT ( 'NONE',  ( 28.24687500061451573, -3.027376345333610441, -5.243569643749999898 ) ) ;
#66923 = CARTESIAN_POINT ( 'NONE',  ( 19.04062500061451146, -3.027376345333614438, 5.243569643749998122 ) ) ;
#66924 = CARTESIAN_POINT ( 'NONE',  ( 3.140625000614516882, 6.054752690667223547, 3.707466751127219781E-16 ) ) ;
#66925 = CARTESIAN_POINT ( 'NONE',  ( 28.37812500061451715, 4.541064518000418104, 2.621784821874999949 ) ) ;
#66926 = CARTESIAN_POINT ( 'NONE',  ( 23.89687500061451786, 6.054752690667223547, 3.707466751127219781E-16 ) ) ;
#66927 = CARTESIAN_POINT ( 'NONE',  ( 19.86562500061451786, 3.027376345333611329, 5.243569643749999010 ) ) ;
#66928 = CARTESIAN_POINT ( 'NONE',  ( -4.243569643749999898, 18.95937500061451431, 30.00000000000000000 ) ) ;
#66929 = CARTESIAN_POINT ( 'NONE',  ( 24.85312500061451502, 0.000000000000000000, 5.243569643749999010 ) ) ;
#66930 = CARTESIAN_POINT ( 'NONE',  ( 4.462500001229035007, 0.000000000000000000, 4.999999999999998224 ) ) ;
#66931 = VERTEX_POINT ( 'NONE', #4245 ) ;
#66932 = CARTESIAN_POINT ( 'NONE',  ( 27.59999999999999787, 4.330127018922192761, -2.499999999999997780 ) ) ;
#66933 = CARTESIAN_POINT ( 'NONE',  ( -2.828200636599751609E-16, 15.38750000000000284, -34.61880215351700230 ) ) ;
#66934 = CARTESIAN_POINT ( 'NONE',  ( 3.756430356250000546, 18.64062499938548001, 27.83122392262697886 ) ) ;
#66935 = CARTESIAN_POINT ( 'NONE',  ( 5.371875000614516615, 3.027376345333613106, -5.243569643749998122 ) ) ;
#66936 = CARTESIAN_POINT ( 'NONE',  ( 13.52812500061451750, 4.541064518000418104, 2.621784821874999949 ) ) ;
#66937 = CARTESIAN_POINT ( 'NONE',  ( 6.796875000614516438, 6.054752690667223547, 3.707466751127219781E-16 ) ) ;
#66938 = CARTESIAN_POINT ( 'NONE',  ( 25.27500000122903145, -5.773502691896255534, -1.060575238724906372E-15 ) ) ;
#66939 = VECTOR ( 'NONE', #13190, 1000.000000000000000 ) ;
#66940 = CARTESIAN_POINT ( 'NONE',  ( 15.38437500061451679, 4.541064518000418104, 2.621784821874999949 ) ) ;
#66941 = CARTESIAN_POINT ( 'NONE',  ( 29.20312500061451644, 4.541064518000418104, -2.621784821874998173 ) ) ;
#66942 = CARTESIAN_POINT ( 'NONE',  ( 29.92500000000000071, 4.330127018922191873, 2.499999999999999556 ) ) ;
#66943 = CARTESIAN_POINT ( 'NONE',  ( 27.04687500061451644, 6.054752690667223547, 3.707466751127219781E-16 ) ) ;
#66944 = CARTESIAN_POINT ( 'NONE',  ( 3.965625000614515727, 3.027376345333613106, -5.243569643749998122 ) ) ;
#66945 = CARTESIAN_POINT ( 'NONE',  ( 13.00312500061451537, 4.541064518000418104, -2.621784821874998173 ) ) ;
#66946 = ORIENTED_EDGE ( 'NONE', *, *, #45929, .F. ) ;
#66947 = CARTESIAN_POINT ( 'NONE',  ( 10.04062500061451502, -3.027376345333614438, 5.243569643749998122 ) ) ;
#66948 = CARTESIAN_POINT ( 'NONE',  ( 7.378125000614518036, -4.541064518000419881, 2.621784821874995952 ) ) ;
#66949 = CARTESIAN_POINT ( 'NONE',  ( 18.30937500061451928, -4.119189519843965641, -2.378215178125001383 ) ) ;
#66950 = CARTESIAN_POINT ( 'NONE',  ( 8.474999999999999645, -4.330127018922194537, 2.499999999999995559 ) ) ;
#66951 = CARTESIAN_POINT ( 'NONE',  ( 2.887500001229035274, 6.123233995736764310E-16, -4.999999999999998224 ) ) ;
#66952 = CARTESIAN_POINT ( 'NONE',  ( 18.78749999999999432, -2.886751345948129988, 4.999999999999997335 ) ) ;
#66953 =( BOUNDED_CURVE ( )  B_SPLINE_CURVE ( 2, ( #69284, #68205, #29748, #52286, #12037, #46750, #40128 ),
 .UNSPECIFIED., .F., .F. ) 
 B_SPLINE_CURVE_WITH_KNOTS ( ( 3, 2, 2, 3 ),
 ( 0.04000000000000007022, 0.04333333333333339726, 0.04666666666666672431, 0.05000000000000005135 ),
 .UNSPECIFIED. ) 
 CURVE ( )  GEOMETRIC_REPRESENTATION_ITEM ( )  RATIONAL_B_SPLINE_CURVE ( ( 0.9999999999999972244, 0.8660254037844414832, 1.000000000000000000, 0.8660254037844387076, 1.000000000000000000, 0.8660254037844367092, 1.000000000000001998 ) ) 
 REPRESENTATION_ITEM ( '' )  );
#66954 = EDGE_CURVE ( 'NONE', #38121, #54432, #54838, .T. ) ;
#66955 = CARTESIAN_POINT ( 'NONE',  ( 18.04687500061451999, 6.054752690667223547, 3.707466751127219781E-16 ) ) ;
#66956 = CARTESIAN_POINT ( 'NONE',  ( 13.98750000122903359, -4.330127018922194537, 2.499999999999995559 ) ) ;
#66957 = CARTESIAN_POINT ( 'NONE',  ( 19.68750000000000355, -2.886751345948129988, 4.999999999999997335 ) ) ;
#66958 = CARTESIAN_POINT ( 'NONE',  ( 9.001249775931846008E-16, 17.21562500061451928, -25.09994784771203058 ) ) ;
#66959 = CARTESIAN_POINT ( 'NONE',  ( -2.000000000000001776, 13.64374999877096784, 33.46410161513775705 ) ) ;
#66960 = CARTESIAN_POINT ( 'NONE',  ( 26.18437500061451573, -2.746126346562646425, 4.756430356249996549 ) ) ;
#66961 = CARTESIAN_POINT ( 'NONE',  ( 18.88125000122903430, -4.330127018922194537, 2.499999999999995559 ) ) ;
#66962 = CARTESIAN_POINT ( 'NONE',  ( 27.44062500061451715, 6.054752690667223547, 3.707466751127219781E-16 ) ) ;
#66963 = LINE ( 'NONE', #27798, #10425 ) ;
#66964 = CARTESIAN_POINT ( 'NONE',  ( 24.33749999999999858, -2.886751345948092684, -5.000000000000057732 ) ) ;
#66965 = CARTESIAN_POINT ( 'NONE',  ( 25.68750000000000000, -2.886751345948125991, -5.000000000000000000 ) ) ;
#66966 = CARTESIAN_POINT ( 'NONE',  ( 8.690625000614515372, -3.027376345333614438, 5.243569643749998122 ) ) ;
#66967 = CARTESIAN_POINT ( 'NONE',  ( 26.37187500061451573, 5.824947211148865298E-16, -4.756430356249998326 ) ) ;
#66968 = CARTESIAN_POINT ( 'NONE',  ( 20.78437500061451715, 4.541064518000418104, 2.621784821874999949 ) ) ;
#66969 = CARTESIAN_POINT ( 'NONE',  ( 13.77187500061451431, 5.824947211148865298E-16, -4.756430356249998326 ) ) ;
#66970 = CARTESIAN_POINT ( 'NONE',  ( 7.415625000614516793, -6.054752690667223547, -1.112240025338166033E-15 ) ) ;
#66971 = CARTESIAN_POINT ( 'NONE',  ( 10.62187500061451928, -6.054752690667223547, -1.112240025338166033E-15 ) ) ;
#66972 = EDGE_LOOP ( 'NONE', ( #68556, #58892, #5366, #64778 ) ) ;
#66973 = CARTESIAN_POINT ( 'NONE',  ( 20.82187500061451857, 3.027376345333611329, 5.243569643749999010 ) ) ;
#66974 = CARTESIAN_POINT ( 'NONE',  ( 28.94999999999999929, 4.330127018922192761, -2.499999999999997780 ) ) ;
#66975 = DIRECTION ( 'NONE',  ( 0.000000000000000000, -1.000000000000000000, 8.673617379884035472E-17 ) ) ;
#66976 = CARTESIAN_POINT ( 'NONE',  ( 4.012500000000001954, -5.773502691896255534, -1.060575238724906372E-15 ) ) ;
#66977 = AXIS2_PLACEMENT_3D ( 'NONE', #56081, #22449, #44998 ) ;
#66978 = CARTESIAN_POINT ( 'NONE',  ( 14.47500000122903430, -5.773502691896255534, -1.060575238724906372E-15 ) ) ;
#66979 = DIRECTION ( 'NONE',  ( -1.000000000000000000, -0.000000000000000000, -0.000000000000000000 ) ) ;
#66980 = CARTESIAN_POINT ( 'NONE',  ( 3.781380313051493580, -3.271273037562549835, 4.098030693279675951 ) ) ;
#66981 = VERTEX_POINT ( 'NONE', #16035 ) ;
#66982 = CARTESIAN_POINT ( 'NONE',  ( 13.68750000000000178, 5.773502691896255534, 3.535250795749688894E-16 ) ) ;
#66983 = CARTESIAN_POINT ( 'NONE',  ( 15.63749999999999751, -2.886751345948129988, 4.999999999999997335 ) ) ;
#66984 = CARTESIAN_POINT ( 'NONE',  ( 13.91250000122903252, 0.000000000000000000, 4.999999999999998224 ) ) ;
#66985 = CARTESIAN_POINT ( 'NONE',  ( 10.67812500061451608, 6.421520780324663323E-16, -5.243569643749999010 ) ) ;
#66986 = CIRCLE ( 'NONE', #12688, 10.00000000000000000 ) ;
#66987 = ORIENTED_EDGE ( 'NONE', *, *, #42756, .F. ) ;
#66988 = CARTESIAN_POINT ( 'NONE',  ( 9.787499999999999645, -2.886751345948129988, 4.999999999999997335 ) ) ;
#66989 = CARTESIAN_POINT ( 'NONE',  ( -3.999999999999997335, 15.65000000122903501, 32.30940107675850470 ) ) ;
#66990 = CARTESIAN_POINT ( 'NONE',  ( -4.243569643749997233, 14.94687500061451679, -27.54997392385601174 ) ) ;
#66991 = CARTESIAN_POINT ( 'NONE',  ( 28.42500000122904069, -5.773502691896255534, -1.060575238724906372E-15 ) ) ;
#66992 = CARTESIAN_POINT ( 'NONE',  ( -3.756430356250000990, 15.15312499938548463, 32.16877607737301048 ) ) ;
#66993 = CARTESIAN_POINT ( 'NONE',  ( 10.72500000000000142, -4.330127018922194537, 2.499999999999995559 ) ) ;
#66994 = DIRECTION ( 'NONE',  ( 0.000000000000000000, 0.000000000000000000, 1.000000000000000000 ) ) ;
#66995 = ORIENTED_EDGE ( 'NONE', *, *, #24066, .F. ) ;
#66996 = CARTESIAN_POINT ( 'NONE',  ( 25.30312500061451431, 0.000000000000000000, 5.243569643749999010 ) ) ;
#66997 = CARTESIAN_POINT ( 'NONE',  ( 4.238135780288177834, -2.653016584470423656, 4.522920254035737386 ) ) ;
#66998 = CARTESIAN_POINT ( 'NONE',  ( 30.00000000000000000, 0.000000000000000000, 0.000000000000000000 ) ) ;
#66999 = CARTESIAN_POINT ( 'NONE',  ( 22.20937500061451431, 0.000000000000000000, 5.243569643749999010 ) ) ;
#67000 = CARTESIAN_POINT ( 'NONE',  ( 17.80312500061451786, -4.541064518000417216, -2.621784821875001281 ) ) ;
#67001 = CARTESIAN_POINT ( 'NONE',  ( -2.121784821874996840, 10.87812500061459353, -26.32496088578401583 ) ) ;
#67002 = CARTESIAN_POINT ( 'NONE',  ( 5.428125000614517859, 4.541064518000418104, 2.621784821874999949 ) ) ;
#67003 =( BOUNDED_CURVE ( )  B_SPLINE_CURVE ( 2, ( #4996, #26801, #48970, #43055, #72228, #15695, #9440 ),
 .UNSPECIFIED., .F., .F. ) 
 B_SPLINE_CURVE_WITH_KNOTS ( ( 3, 2, 2, 3 ),
 ( 0.2666666666666666075, 0.2694444444444444309, 0.2722222222222221988, 0.2750000000000000777 ),
 .UNSPECIFIED. ) 
 CURVE ( )  GEOMETRIC_REPRESENTATION_ITEM ( )  RATIONAL_B_SPLINE_CURVE ( ( 1.000000000000002665, 0.8660254037844360431, 1.000000000000000000, 0.8660254037844387076, 1.000000000000000000, 0.8660254037844360431, 1.000000000000002665 ) ) 
 REPRESENTATION_ITEM ( '' )  );
#67004 = CARTESIAN_POINT ( 'NONE',  ( 29.55000000122903003, 5.773502691896255534, 3.535250795749688894E-16 ) ) ;
#67005 = CARTESIAN_POINT ( 'NONE',  ( 23.89687500061451786, 5.492252693125287522, 3.363034840372157021E-16 ) ) ;
#67006 = CARTESIAN_POINT ( 'NONE',  ( 19.56562500061451715, -6.054752690667223547, -1.112240025338166033E-15 ) ) ;
#67007 = CARTESIAN_POINT ( 'NONE',  ( 9.159375000614515372, 0.000000000000000000, 4.756430356249998326 ) ) ;
#67008 = CARTESIAN_POINT ( 'NONE',  ( -7.967954043666661671E-16, 17.92812499938548498, 34.33755215474603517 ) ) ;
#67009 = CARTESIAN_POINT ( 'NONE',  ( 15.45937500061451608, 0.000000000000000000, 5.243569643749999010 ) ) ;
#67010 = CARTESIAN_POINT ( 'NONE',  ( 15.34687500061451537, 6.054752690667223547, 3.707466751127219781E-16 ) ) ;
#67011 = CARTESIAN_POINT ( 'NONE',  ( 22.88437500061451857, 6.421520780324663323E-16, -5.243569643749999010 ) ) ;
#67012 = ORIENTED_EDGE ( 'NONE', *, *, #20226, .F. ) ;
#67013 = CARTESIAN_POINT ( 'NONE',  ( -2.121784821874996840, 11.83437500061451786, 33.67503911421598417 ) ) ;
#67014 = CARTESIAN_POINT ( 'NONE',  ( 3.740625000614516527, -3.027376345333614438, 5.243569643749998122 ) ) ;
#67016 =( BOUNDED_SURFACE ( )  B_SPLINE_SURFACE ( 1, 2, ( 
 ( #35658, #52652, #30118, #2058, #47115, #41932, #64458, #6507, #26038, #42299, #49311, #47844, #54483, #21216, #43769, #3147, #20852, #71845, #48577, #48210, #43030, #64825, #20477, #4254, #60368, #65559, #14948, #60007, #37486, #9417, #54845, #25297, #15673, #31947, #59639, #42664, #66293, #53378, #58904, #14214, #71104, #26779, #36750, #3884, #37847, #26404, #48947, #15309, #71476, #9777, #65189, #43404, #8315, #59270, #65929, #30844, #2774, #31210, #14579, #32311, #70372, #8678, #19750, #53750, #25673, #9051, #70732, #20110, #37112, #31582, #54121, #3517, #50409, #72207, #60738, #38590, #32680, #50763, #5697, #10148, #67756, #67404, #39689, #45223, #28233, #168, #6054, #10513, #11603, #50040, #22672, #44138, #17128, #33040, #21952, #27876, #67043, #62207, #61475, #11241, #61116, #27507, #34120, #61836, #44509, #55580, #56660, #4614, #28589, #66665, #33764, #55219, #27144, #21584, #4973, #49678, #72566, #16403, #10870, #56308, #51126, #523, #16042, #39323, #38957, #23034, #45589, #33403, #55940, #68123, #5336, #38210, #72933, #22315, #44868, #16765, #34483, #62562, #52928, #51489, #889, #6418, #11958, #23753, #18566, #63283, #41484, #7497, #1607, #68476, #40050, #57013, #62918, #12313, #23396, #46302, #34848, #7140, #30025, #28950, #29670, #13384, #45945, #52206, #69563, #24118, #58089, #47028, #52568, #18924, #1248, #35570, #35929, #17838, #63642, #58451, #40399, #57375, #68841, #1975, #6782, #29314, #24484, #64004, #46667, #40769, #7863, #51845, #30399, #18198, #12675, #13031, #69208, #35212, #57734, #41132, #2325, #24841, #47388, #17488, #26317, #25951, #71387, #3795, #59922, #9328, #37760, #42213, #43318, #8591, #54396, #2687, #31861, #64737, #53661, #59551, #25584, #48856, #20021, #42942, #70286, #59182, #20760, #20393, #3053, #19658, #65838, #36304, #15221, #25203, #65468, #19288, #58818, #30757, #14125, #64371, #36663, #31121, #42575, #14859, #60278, #9691, #8229, #71015, #53288, #32224, #54758, #47751, #48123, #4162, #70646, #26692, #41842, #69918, #65103, #14492, #13762, #37026, #8962, #31496, #54036, #3431, #48491, #37398, #50323, #21861, #80, #39233, #33316, #27057, #71759, #43681, #21495, #44048, #55130, #4884, #66572, #38870, #61745, #21128, #5964, #27786, #49950, #32953, #56568, #66204, #11509, #32592, #39593, #16317, #38499, #55854, #4528, #10783, #67669, #50676, #5244, #72847, #22228, #44784, #67317, #45134, #15582, #38124, #16675, #49587, #15951, #72475, #66949, #10060, #72111, #61025, #11147, #55490, #61387, #33677, #44422, #56219, #10422, #28148, #62117, #34031, #5612, #22585, #27419, #17036, #49225, #60645, #1889, #68389, #1159, #22939, #35481, #430, #34390, #797, #18479, #58003, #34753, #63194, #58362, #35838, #23305, #62831, #46214, #12225, #51395, #45854, #17750, #40309, #17401, #29939, #57288, #28498, #51034, #62472, #6694, #13301, #7411, #51759, #68753, #52479, #45499, #57646, #29223, #24394, #23668, #29582, #68030, #39958, #6326, #46943, #18111, #69479, #40674, #12589, #35123, #7053, #52120, #1522, #11869, #18837, #24027, #41400, #63915, #56922, #28855, #46576, #69121, #41044, #63558, #12945, #59831, #58729, #24755, #53200, #37669, #42492, #54311, #36575, #53944, #53567, #70191, #30309, #48767, #20669, #30667, #48037, #64281, #71290, #69835, #3341, #43227, #65747, #25116, #42854, #13669, #19198, #52841, #14034, #8868, #2962, #31774, #70929, #65015, #8141, #2240, #47298, #2596, #47658, #36212, #59095, #19569, #70563, #20300, #41753, #7776, #59460, #8501, #64650, #15131, #42124, #31031, #25492, #19938, #3702, #14403, #36940, #9238, #31404, #48403, #37309, #65376, #26229, #25864, #14765, #56126, #66112, #33222, #5519, #54666, #32501, #43958, #44692, #26596, #15491, #5154, #72752, #49860, #10329, #28057, #32133, #61653, #71664, #32863, #55760, #72384, #21039, #9601, #60556, #4070, #22137, #27689, #49136, #16584, #16227, #11052, #67223, #50227, #39135, #50585, #55035, #33580, #72024, #73113, #38034, #22495, #4438, #66479, #21764, #15857, #45045, #55398, #67580, #9963, #49495, #16946, #10691, #38403, #26966, #60191, #43590, #21401, #60926, #4794, #27326, #44326, #66855, #38779, #61297, #39871, #62383, #12139, #57561, #40957, #52391, #5874, #40585, #50943, #23940, #57917, #342, #17663, #46489, #707, #24309, #62023, #46855, #17311, #28407, #56482, #11422, #1798, #22848, #34664, #28765, #33939, #7324, #69396, #11782, #6608, #45402, #29855, #67938, #35033, #39499, #34298, #56830, #1434, #6237, #29136, #51304, #23582, #23215, #1074, #45768, #63472, #46127, #68665, #63105, #18029, #12505, #35392, #68304, #40224, #6964, #62746, #57193, #51669, #29495, #52031, #69028, #18389, #12860, #2508, #30940, #59006, #64561, #3247, #53111, #70836, #9148, #31684, #70475, #8410, #41668, #42038, #36124, #25775, #65286, #58643 ),
 ( #64191, #8051, #13578, #7684, #20212, #25031, #48677, #18750, #52753, #30585, #3615, #42766, #13950, #53481, #48313, #13217, #47947, #47574, #14674, #70104, #19852, #63824, #58276, #69745, #37218, #19480, #59740, #36487, #2873, #25404, #42403, #64925, #14315, #35755, #54217, #36851, #26136, #41314, #30220, #24667, #19113, #2156, #59367, #8778, #47213, #31313, #53856, #15045, #44515, #28955, #33771, #45597, #27881, #45228, #38964, #39328, #61481, #55946, #21959, #65656, #40055, #16771, #28595, #6061, #68128, #3983, #49048, #23039, #56313, #50770, #57018, #51131, #72572, #37583, #67050, #71201, #5703, #17494, #50415, #67761, #44874, #10875, #20577, #62568, #11964, #16409, #61842, #54579, #34489, #60105, #17134, #6423, #43132, #33408, #34126, #9514, #11246, #5342, #28238, #26508, #173, #32047, #528, #22678, #39694, #62213, #11608, #56665, #72939, #22321, #67409, #1981, #34853, #68846, #52212, #69214, #12318, #29321, #57380, #30033, #35218, #63647, #18572, #24124, #35934, #12681, #30405, #41849, #64376, #52573, #41138, #1254, #1614, #18205, #58457, #24848, #40774, #46674, #45951, #7869, #23402, #6787, #23758, #41490, #52933, #57739, #13038, #8234, #58824, #46309, #7145, #35575, #29676, #63288, #58096, #7502, #24490, #40406, #2330, #47034, #51494, #895, #51850, #69569, #36309, #47394, #18930, #64010, #69925, #68481, #13390, #19294, #13768, #17844, #62924, #2695, #70293, #8598, #32230, #42583, #4169, #37033, #20767, #60285, #14499, #48862, #26698, #36669, #3802, #49232, #25210, #3059, #59557, #15227, #19665, #59188, #71394, #43324, #20399, #54042, #71765, #47757, #54765, #42219, #3438, #26325, #42948, #64743, #53295, #31127, #14133, #65845, #37766, #53668, #9697, #59928, #21135, #43687, #66210, #15588, #38130, #25590, #60652, #65109, #30763, #48129, #70653, #20027, #8970, #65476, #31502, #25957, #48497, #71022, #14865, #37405, #9335, #54402, #31867, #10429, #62123, #49594, #11515, #15957, #5618, #32598, #72119, #44054, #4891, #4535, #32960, #55496, #55860, #28154, #34037, #22946, #21501, #11154, #66580, #67674, #28503, #38506, #61395, #17044, #44428, #68037, #55137, #17407, #61031, #27426, #27063, #49957, #45507, #72481, #21867, #66957, #16323, #38876, #33681, #5249, #56576, #85, #67322, #10788, #33322, #27791, #50328, #72852, #22234, #44790, #16682, #39238, #22590, #61752, #39964, #56225, #50682, #45141, #10067, #39602, #5972, #51041, #437, #58370, #17756, #24035, #41406, #46584, #29945, #18845, #45861, #41051, #46221, #1528, #29588, #35129, #46949, #23674, #63922, #52848, #2246, #63564, #52126, #12231, #12596, #6700, #69486, #35845, #29233, #57654, #56928, #13307, #34400, #68395, #34760, #52485, #7781, #68760, #69127, #19205, #69840, #57295, #18118, #7060, #40682, #51766, #1165, #63200, #18485, #51402, #30318, #12952, #62478, #11876, #23312, #35489, #47305, #24762, #58009, #7417, #6332, #28863, #1896, #24400, #805, #40316, #62839, #64288, #58736, #47665, #9246, #59102, #54320, #31038, #14042, #42499, #36582, #8509, #19575, #13676, #26238, #19946, #37317, #14775, #31781, #2602, #70199, #3711, #36948, #31413, #20678, #59841, #42131, #36220, #64657, #65755, #59468, #48775, #53574, #25872, #48045, #2972, #41759, #8147, #30674, #25500, #53953, #70570, #53206, #65022, #71299, #25123, #14411, #43235, #8878, #3350, #48412, #70938, #20309, #42862, #65384, #48346, #54250, #65690, #20983, #49081, #3280, #65319, #54980, #26540, #9180, #25808, #4385, #42436, #26915, #8811, #71609, #37979, #66427, #43171, #14709, #60136, #59402, #37614, #32809, #70871, #20245, #32079, #4016, #54610, #9545, #71974, #64958, #25436, #43536, #31348, #42797, #3647, #20612, #36884, #53889, #37252, #66057, #59774, #15077, #15435, #48711, #60501, #31715, #49440, #15805, #38346, #9907, #32444, #26170, #71233, #21347, #43903, #60874, #10277, #2905, #70506, #47979, #19883, #14349, #27637, #46349, #12717, #61603, #17884, #13075, #63685, #50172, #16533, #73063, #39086, #5102, #72701, #22083, #44642, #44271, #57774, #11004, #55347, #4741, #16174, #67172, #41176, #35253, #5466, #22444, #63329, #49808, #12355, #33524, #7184, #56074, #57419, #27275, #21713, #33170, #29712, #28006, #52250, #50535, #44993, #68523, #40444, #62960, #34890, #72333, #24161, #6823, #1653, #46714, #69249, #61246, #55708, #18611, #29357, #51890, #66803, #38725, #1288, #10640, #23798, #68883, #18240, #40813, #64416, #8636, #8273, #24887, #58134, #3476, #48535, #58497, #2734, #18969, #25996, #24529, #31165, #71062, #20437, #52973, #7540, #42986, #13428, #47073, #52612, #30073, #65517, #69608, #41529, #64048, #2018, #41888, #36706, #30803, #59595, #25629, #19705, #35977, #7906, #30444, #2369, #47432, #69963, #13809, #19334, #25251, #48166, #36349, #35614, #14172, #58863, #53336, #47799, #70329, #42258, #64781 ) ),
 .UNSPECIFIED., .F., .F., .F. ) 
 B_SPLINE_SURFACE_WITH_KNOTS ( ( 2, 2 ),
 ( 3, 2, 2, 2, 2, 2, 2, 2, 2, 2, 2, 2, 2, 2, 2, 2, 2, 2, 2, 2, 2, 2, 2, 2, 2, 2, 2, 2, 2, 2, 2, 2, 2, 2, 2, 2, 2, 2, 2, 2, 2, 2, 2, 2, 2, 2, 2, 2, 2, 2, 2, 2, 2, 2, 2, 2, 2, 2, 2, 2, 2, 2, 2, 2, 2, 2, 2, 2, 2, 2, 2, 2, 2, 2, 2, 2, 2, 2, 2, 2, 2, 2, 2, 2, 2, 2, 2, 2, 2, 2, 2, 2, 2, 2, 2, 2, 2, 2, 2, 2, 2, 2, 2, 2, 2, 2, 2, 2, 2, 2, 2, 2, 2, 2, 2, 2, 2, 2, 2, 2, 2, 2, 2, 2, 2, 2, 2, 2, 2, 2, 2, 2, 2, 2, 2, 2, 2, 2, 2, 2, 2, 2, 2, 2, 2, 2, 2, 2, 2, 2, 2, 2, 2, 2, 2, 2, 2, 2, 2, 2, 2, 2, 2, 2, 2, 2, 2, 2, 2, 2, 2, 2, 2, 2, 2, 2, 2, 2, 2, 2, 2, 2, 2, 2, 2, 2, 2, 2, 2, 2, 2, 2, 2, 2, 2, 2, 2, 2, 2, 2, 2, 2, 2, 2, 2, 2, 2, 2, 2, 2, 2, 2, 2, 2, 2, 2, 2, 2, 2, 2, 2, 2, 2, 2, 2, 2, 2, 2, 2, 2, 2, 2, 2, 2, 2, 2, 2, 2, 2, 2, 2, 2, 2, 2, 2, 2, 2, 2, 2, 2, 2, 2, 2, 2, 2, 2, 2, 2, 2, 2, 2, 2, 2, 2, 2, 2, 2, 2, 2, 2, 2, 2, 2, 2, 2, 2, 2, 2, 2, 2, 2, 2, 2, 2, 2, 2, 2, 2, 2, 2, 2, 2, 2, 2, 2, 2, 2, 2, 2, 2, 3 ),
 ( 0.000000000000000000, 1.000000000000000000 ),
 ( 0.000000000000000000, 0.003333333333333333547, 0.006666666666666667095, 0.01000000000000000021, 0.01333333333333333419, 0.01666666666666666644, 0.02000000000000000042, 0.02333333333333333440, 0.02666666666666666838, 0.02999999999999999889, 0.03333333333333333287, 0.03666666666666666685, 0.04000000000000000083, 0.04333333333333333481, 0.04666666666666666879, 0.05000000000000000278, 0.05333333333333333676, 0.05666666666666666380, 0.05999999999999999778, 0.06333333333333333870, 0.06666666666666666574, 0.07000000000000000666, 0.07333333333333333370, 0.07666666666666666075, 0.08000000000000000167, 0.08333333333333332871, 0.08666666666666666963, 0.08999999999999999667, 0.09333333333333333759, 0.09666666666666666463, 0.1000000000000000056, 0.1033333333333333326, 0.1066666666666666735, 0.1100000000000000006, 0.1133333333333333276, 0.1166666666666666685, 0.1199999999999999956, 0.1233333333333333365, 0.1266666666666666774, 0.1300000000000000044, 0.1333333333333333315, 0.1366666666666666585, 0.1400000000000000133, 0.1433333333333333404, 0.1466666666666666674, 0.1499999999999999944, 0.1533333333333333215, 0.1566666666666666763, 0.1600000000000000033, 0.1633333333333333304, 0.1666666666666666574, 0.1700000000000000122, 0.1733333333333333393, 0.1766666666666666663, 0.1799999999999999933, 0.1833333333333333204, 0.1866666666666666752, 0.1900000000000000022, 0.1933333333333333293, 0.1966666666666666563, 0.2000000000000000111, 0.2033333333333333381, 0.2066666666666666652, 0.2099999999999999922, 0.2133333333333333470, 0.2166666666666666741, 0.2200000000000000011, 0.2233333333333333282, 0.2266666666666666552, 0.2300000000000000100, 0.2333333333333333370, 0.2366666666666666641, 0.2399999999999999911, 0.2433333333333333459, 0.2466666666666666730, 0.2500000000000000000, 0.2533333333333333548, 0.2566666666666666541, 0.2600000000000000089, 0.2633333333333333082, 0.2666666666666666630, 0.2700000000000000178, 0.2733333333333333171, 0.2766666666666666718, 0.2800000000000000266, 0.2833333333333333259, 0.2866666666666666807, 0.2899999999999999800, 0.2933333333333333348, 0.2966666666666666896, 0.2999999999999999889, 0.3033333333333333437, 0.3066666666666666430, 0.3099999999999999978, 0.3133333333333333526, 0.3166666666666666519, 0.3200000000000000067, 0.3233333333333333059, 0.3266666666666666607, 0.3300000000000000155, 0.3333333333333333148, 0.3366666666666666696, 0.3400000000000000244, 0.3433333333333333237, 0.3466666666666666785, 0.3499999999999999778, 0.3533333333333333326, 0.3566666666666666874, 0.3599999999999999867, 0.3633333333333333415, 0.3666666666666666408, 0.3699999999999999956, 0.3733333333333333504, 0.3766666666666666496, 0.3800000000000000044, 0.3833333333333333592, 0.3866666666666666585, 0.3900000000000000133, 0.3933333333333333126, 0.3966666666666666674, 0.4000000000000000222, 0.4033333333333333215, 0.4066666666666666763, 0.4099999999999999756, 0.4133333333333333304, 0.4166666666666666852, 0.4199999999999999845, 0.4233333333333333393, 0.4266666666666666941, 0.4299999999999999933, 0.4333333333333333481, 0.4366666666666666474, 0.4400000000000000022, 0.4433333333333333570, 0.4466666666666666563, 0.4500000000000000111, 0.4533333333333333104, 0.4566666666666666652, 0.4600000000000000200, 0.4633333333333333193, 0.4666666666666666741, 0.4699999999999999734, 0.4733333333333333282, 0.4766666666666666829, 0.4799999999999999822, 0.4833333333333333370, 0.4866666666666666918, 0.4899999999999999911, 0.4933333333333333459, 0.4966666666666666452, 0.5000000000000000000, 0.5033333333333332993, 0.5066666666666667096, 0.5100000000000000089, 0.5133333333333333082, 0.5166666666666667185, 0.5200000000000000178, 0.5233333333333333171, 0.5266666666666666163, 0.5300000000000000266, 0.5333333333333333259, 0.5366666666666666252, 0.5400000000000000355, 0.5433333333333333348, 0.5466666666666666341, 0.5500000000000000444, 0.5533333333333333437, 0.5566666666666666430, 0.5600000000000000533, 0.5633333333333333526, 0.5666666666666666519, 0.5699999999999999512, 0.5733333333333333615, 0.5766666666666666607, 0.5799999999999999600, 0.5833333333333333703, 0.5866666666666666696, 0.5899999999999999689, 0.5933333333333333792, 0.5966666666666666785, 0.5999999999999999778, 0.6033333333333333881, 0.6066666666666666874, 0.6099999999999999867, 0.6133333333333332860, 0.6166666666666666963, 0.6199999999999999956, 0.6233333333333332948, 0.6266666666666667052, 0.6300000000000000044, 0.6333333333333333037, 0.6366666666666667140, 0.6400000000000000133, 0.6433333333333333126, 0.6466666666666666119, 0.6500000000000000222, 0.6533333333333333215, 0.6566666666666666208, 0.6600000000000000311, 0.6633333333333333304, 0.6666666666666666297, 0.6700000000000000400, 0.6733333333333333393, 0.6766666666666666385, 0.6800000000000000488, 0.6833333333333333481, 0.6866666666666666474, 0.6899999999999999467, 0.6933333333333333570, 0.6966666666666666563, 0.6999999999999999556, 0.7033333333333333659, 0.7066666666666666652, 0.7099999999999999645, 0.7133333333333333748, 0.7166666666666666741, 0.7199999999999999734, 0.7233333333333333837, 0.7266666666666666829, 0.7299999999999999822, 0.7333333333333332815, 0.7366666666666666918, 0.7399999999999999911, 0.7433333333333332904, 0.7466666666666667007, 0.7500000000000000000, 0.7533333333333332993, 0.7566666666666667096, 0.7600000000000000089, 0.7633333333333333082, 0.7666666666666667185, 0.7700000000000000178, 0.7733333333333333171, 0.7766666666666666163, 0.7800000000000000266, 0.7833333333333333259, 0.7866666666666666252, 0.7900000000000000355, 0.7933333333333333348, 0.7966666666666666341, 0.8000000000000000444, 0.8033333333333333437, 0.8066666666666666430, 0.8100000000000000533, 0.8133333333333333526, 0.8166666666666666519, 0.8199999999999999512, 0.8233333333333333615, 0.8266666666666666607, 0.8299999999999999600, 0.8333333333333333703, 0.8366666666666666696, 0.8399999999999999689, 0.8433333333333333792, 0.8466666666666666785, 0.8499999999999999778, 0.8533333333333333881, 0.8566666666666666874, 0.8599999999999999867, 0.8633333333333332860, 0.8666666666666666963, 0.8699999999999999956, 0.8733333333333332948, 0.8766666666666667052, 0.8800000000000000044, 0.8833333333333333037, 0.8866666666666667140, 0.8900000000000000133, 0.8933333333333333126, 0.8966666666666666119, 0.9000000000000000222, 0.9033333333333333215, 0.9066666666666666208, 0.9100000000000000311, 0.9133333333333333304, 0.9166666666666666297, 0.9200000000000000400, 0.9233333333333333393, 0.9266666666666666385, 0.9300000000000000488, 0.9333333333333333481, 0.9366666666666666474, 0.9399999999999999467, 0.9433333333333333570, 0.9466666666666666563, 0.9499999999999999556, 0.9533333333333333659, 0.9566666666666666652, 0.9599999999999999645, 0.9633333333333333748, 0.9666666666666666741, 0.9699999999999999734, 0.9733333333333333837, 0.9766666666666666829, 0.9799999999999999822, 0.9833333333333332815, 0.9866666666666666918, 0.9899999999999999911, 0.9933333333333332904, 0.9966666666666667007, 1.000000000000000000 ),
 .UNSPECIFIED. ) 
 GEOMETRIC_REPRESENTATION_ITEM ( )  RATIONAL_B_SPLINE_SURFACE ( (
 ( 1.000000000000000000, 0.8660254037844387076, 1.000000000000000000, 0.8660254037844387076, 1.000000000000000000, 0.8660254037844387076, 1.000000000000000000, 0.8660254037844387076, 1.000000000000000000, 0.8660254037844387076, 1.000000000000000000, 0.8660254037844387076, 1.000000000000000000, 0.8660254037844387076, 1.000000000000000000, 0.8660254037844387076, 1.000000000000000000, 0.8660254037844387076, 1.000000000000000000, 0.8660254037844387076, 1.000000000000000000, 0.8660254037844387076, 1.000000000000000000, 0.8660254037844387076, 1.000000000000000000, 0.8660254037844387076, 1.000000000000000000, 0.8660254037844387076, 1.000000000000000000, 0.8660254037844387076, 1.000000000000000000, 0.8660254037844387076, 1.000000000000000000, 0.8660254037844387076, 1.000000000000000000, 0.8660254037844387076, 1.000000000000000000, 0.8660254037844387076, 1.000000000000000000, 0.8660254037844387076, 1.000000000000000000, 0.8660254037844387076, 1.000000000000000000, 0.8660254037844387076, 1.000000000000000000, 0.8660254037844387076, 1.000000000000000000, 0.8660254037844387076, 1.000000000000000000, 0.8660254037844387076, 1.000000000000000000, 0.8660254037844387076, 1.000000000000000000, 0.8660254037844387076, 1.000000000000000000, 0.8660254037844387076, 1.000000000000000000, 0.8660254037844387076, 1.000000000000000000, 0.8660254037844387076, 1.000000000000000000, 0.8660254037844387076, 1.000000000000000000, 0.8660254037844387076, 1.000000000000000000, 0.8660254037844387076, 1.000000000000000000, 0.8660254037844387076, 1.000000000000000000, 0.8660254037844387076, 1.000000000000000000, 0.8660254037844387076, 1.000000000000000000, 0.8660254037844387076, 1.000000000000000000, 0.8660254037844387076, 1.000000000000000000, 0.8660254037844387076, 1.000000000000000000, 0.8660254037844387076, 1.000000000000000000, 0.8660254037844387076, 1.000000000000000000, 0.8660254037844387076, 1.000000000000000000, 0.8660254037844387076, 1.000000000000000000, 0.8660254037844387076, 1.000000000000000000, 0.8660254037844387076, 1.000000000000000000, 0.8660254037844387076, 1.000000000000000000, 0.8660254037844387076, 1.000000000000000000, 0.8660254037844387076, 1.000000000000000000, 0.8660254037844387076, 1.000000000000000000, 0.8660254037844387076, 1.000000000000000000, 0.8660254037844387076, 1.000000000000000000, 0.8660254037844387076, 1.000000000000000000, 0.8660254037844387076, 1.000000000000000000, 0.8660254037844387076, 1.000000000000000000, 0.8660254037844387076, 1.000000000000000000, 0.8660254037844387076, 1.000000000000000000, 0.8660254037844387076, 1.000000000000000000, 0.8660254037844387076, 1.000000000000000000, 0.8660254037844387076, 1.000000000000000000, 0.8660254037844387076, 1.000000000000000000, 0.8660254037844387076, 1.000000000000000000, 0.8660254037844387076, 1.000000000000000000, 0.8660254037844387076, 1.000000000000000000, 0.8660254037844387076, 1.000000000000000000, 0.8660254037844387076, 1.000000000000000000, 0.8660254037844387076, 1.000000000000000000, 0.8660254037844387076, 1.000000000000000000, 0.8660254037844387076, 1.000000000000000000, 0.8660254037844387076, 1.000000000000000000, 0.8660254037844387076, 1.000000000000000000, 0.8660254037844387076, 1.000000000000000000, 0.8660254037844387076, 1.000000000000000000, 0.8660254037844387076, 1.000000000000000000, 0.8660254037844387076, 1.000000000000000000, 0.8660254037844387076, 1.000000000000000000, 0.8660254037844387076, 1.000000000000000000, 0.8660254037844387076, 1.000000000000000000, 0.8660254037844387076, 1.000000000000000000, 0.8660254037844387076, 1.000000000000000000, 0.8660254037844387076, 1.000000000000000000, 0.8660254037844387076, 1.000000000000000000, 0.8660254037844387076, 1.000000000000000000, 0.8660254037844387076, 1.000000000000000000, 0.8660254037844387076, 1.000000000000000000, 0.8660254037844387076, 1.000000000000000000, 0.8660254037844387076, 1.000000000000000000, 0.8660254037844387076, 1.000000000000000000, 0.8660254037844387076, 1.000000000000000000, 0.8660254037844387076, 1.000000000000000000, 0.8660254037844387076, 1.000000000000000000, 0.8660254037844387076, 1.000000000000000000, 0.8660254037844387076, 1.000000000000000000, 0.8660254037844387076, 1.000000000000000000, 0.8660254037844387076, 1.000000000000000000, 0.8660254037844387076, 1.000000000000000000, 0.8660254037844387076, 1.000000000000000000, 0.8660254037844387076, 1.000000000000000000, 0.8660254037844387076, 1.000000000000000000, 0.8660254037844387076, 1.000000000000000000, 0.8660254037844387076, 1.000000000000000000, 0.8660254037844387076, 1.000000000000000000, 0.8660254037844387076, 1.000000000000000000, 0.8660254037844387076, 1.000000000000000000, 0.8660254037844387076, 1.000000000000000000, 0.8660254037844387076, 1.000000000000000000, 0.8660254037844387076, 1.000000000000000000, 0.8660254037844387076, 1.000000000000000000, 0.8660254037844387076, 1.000000000000000000, 0.8660254037844387076, 1.000000000000000000, 0.8660254037844387076, 1.000000000000000000, 0.8660254037844387076, 1.000000000000000000, 0.8660254037844387076, 1.000000000000000000, 0.8660254037844387076, 1.000000000000000000, 0.8660254037844387076, 1.000000000000000000, 0.8660254037844387076, 1.000000000000000000, 0.8660254037844387076, 1.000000000000000000, 0.8660254037844387076, 1.000000000000000000, 0.8660254037844387076, 1.000000000000000000, 0.8660254037844387076, 1.000000000000000000, 0.8660254037844387076, 1.000000000000000000, 0.8660254037844387076, 1.000000000000000000, 0.8660254037844387076, 1.000000000000000000, 0.8660254037844387076, 1.000000000000000000, 0.8660254037844387076, 1.000000000000000000, 0.8660254037844387076, 1.000000000000000000, 0.8660254037844387076, 1.000000000000000000, 0.8660254037844387076, 1.000000000000000000, 0.8660254037844387076, 1.000000000000000000, 0.8660254037844387076, 1.000000000000000000, 0.8660254037844387076, 1.000000000000000000, 0.8660254037844387076, 1.000000000000000000, 0.8660254037844387076, 1.000000000000000000, 0.8660254037844387076, 1.000000000000000000, 0.8660254037844387076, 1.000000000000000000, 0.8660254037844387076, 1.000000000000000000, 0.8660254037844387076, 1.000000000000000000, 0.8660254037844387076, 1.000000000000000000, 0.8660254037844387076, 1.000000000000000000, 0.8660254037844387076, 1.000000000000000000, 0.8660254037844387076, 1.000000000000000000, 0.8660254037844387076, 1.000000000000000000, 0.8660254037844387076, 1.000000000000000000, 0.8660254037844387076, 1.000000000000000000, 0.8660254037844387076, 1.000000000000000000, 0.8660254037844387076, 1.000000000000000000, 0.8660254037844387076, 1.000000000000000000, 0.8660254037844387076, 1.000000000000000000, 0.8660254037844387076, 1.000000000000000000, 0.8660254037844387076, 1.000000000000000000, 0.8660254037844387076, 1.000000000000000000, 0.8660254037844387076, 1.000000000000000000, 0.8660254037844387076, 1.000000000000000000, 0.8660254037844387076, 1.000000000000000000, 0.8660254037844387076, 1.000000000000000000, 0.8660254037844387076, 1.000000000000000000, 0.8660254037844387076, 1.000000000000000000, 0.8660254037844387076, 1.000000000000000000, 0.8660254037844387076, 1.000000000000000000, 0.8660254037844387076, 1.000000000000000000, 0.8660254037844387076, 1.000000000000000000, 0.8660254037844387076, 1.000000000000000000, 0.8660254037844387076, 1.000000000000000000, 0.8660254037844387076, 1.000000000000000000, 0.8660254037844387076, 1.000000000000000000, 0.8660254037844387076, 1.000000000000000000, 0.8660254037844387076, 1.000000000000000000, 0.8660254037844387076, 1.000000000000000000, 0.8660254037844387076, 1.000000000000000000, 0.8660254037844387076, 1.000000000000000000, 0.8660254037844387076, 1.000000000000000000, 0.8660254037844387076, 1.000000000000000000, 0.8660254037844387076, 1.000000000000000000, 0.8660254037844387076, 1.000000000000000000, 0.8660254037844387076, 1.000000000000000000, 0.8660254037844387076, 1.000000000000000000, 0.8660254037844387076, 1.000000000000000000, 0.8660254037844387076, 1.000000000000000000, 0.8660254037844387076, 1.000000000000000000, 0.8660254037844387076, 1.000000000000000000, 0.8660254037844387076, 1.000000000000000000, 0.8660254037844387076, 1.000000000000000000, 0.8660254037844387076, 1.000000000000000000, 0.8660254037844387076, 1.000000000000000000, 0.8660254037844387076, 1.000000000000000000, 0.8660254037844387076, 1.000000000000000000, 0.8660254037844387076, 1.000000000000000000, 0.8660254037844387076, 1.000000000000000000, 0.8660254037844387076, 1.000000000000000000, 0.8660254037844387076, 1.000000000000000000, 0.8660254037844387076, 1.000000000000000000, 0.8660254037844387076, 1.000000000000000000, 0.8660254037844387076, 1.000000000000000000, 0.8660254037844387076, 1.000000000000000000, 0.8660254037844387076, 1.000000000000000000, 0.8660254037844387076, 1.000000000000000000, 0.8660254037844387076, 1.000000000000000000, 0.8660254037844387076, 1.000000000000000000, 0.8660254037844387076, 1.000000000000000000, 0.8660254037844387076, 1.000000000000000000, 0.8660254037844387076, 1.000000000000000000, 0.8660254037844387076, 1.000000000000000000, 0.8660254037844387076, 1.000000000000000000, 0.8660254037844387076, 1.000000000000000000, 0.8660254037844387076, 1.000000000000000000, 0.8660254037844387076, 1.000000000000000000, 0.8660254037844387076, 1.000000000000000000, 0.8660254037844387076, 1.000000000000000000, 0.8660254037844387076, 1.000000000000000000, 0.8660254037844387076, 1.000000000000000000, 0.8660254037844387076, 1.000000000000000000, 0.8660254037844387076, 1.000000000000000000, 0.8660254037844387076, 1.000000000000000000, 0.8660254037844387076, 1.000000000000000000, 0.8660254037844387076, 1.000000000000000000, 0.8660254037844387076, 1.000000000000000000, 0.8660254037844387076, 1.000000000000000000, 0.8660254037844387076, 1.000000000000000000, 0.8660254037844387076, 1.000000000000000000, 0.8660254037844387076, 1.000000000000000000, 0.8660254037844387076, 1.000000000000000000, 0.8660254037844387076, 1.000000000000000000, 0.8660254037844387076, 1.000000000000000000, 0.8660254037844387076, 1.000000000000000000, 0.8660254037844387076, 1.000000000000000000, 0.8660254037844387076, 1.000000000000000000, 0.8660254037844387076, 1.000000000000000000, 0.8660254037844387076, 1.000000000000000000, 0.8660254037844387076, 1.000000000000000000, 0.8660254037844387076, 1.000000000000000000, 0.8660254037844387076, 1.000000000000000000, 0.8660254037844387076, 1.000000000000000000, 0.8660254037844387076, 1.000000000000000000, 0.8660254037844387076, 1.000000000000000000, 0.8660254037844387076, 1.000000000000000000, 0.8660254037844387076, 1.000000000000000000, 0.8660254037844387076, 1.000000000000000000, 0.8660254037844387076, 1.000000000000000000, 0.8660254037844387076, 1.000000000000000000, 0.8660254037844387076, 1.000000000000000000, 0.8660254037844387076, 1.000000000000000000, 0.8660254037844387076, 1.000000000000000000, 0.8660254037844387076, 1.000000000000000000, 0.8660254037844387076, 1.000000000000000000, 0.8660254037844387076, 1.000000000000000000, 0.8660254037844387076, 1.000000000000000000, 0.8660254037844387076, 1.000000000000000000, 0.8660254037844387076, 1.000000000000000000, 0.8660254037844387076, 1.000000000000000000, 0.8660254037844387076, 1.000000000000000000, 0.8660254037844387076, 1.000000000000000000, 0.8660254037844387076, 1.000000000000000000, 0.8660254037844387076, 1.000000000000000000, 0.8660254037844387076, 1.000000000000000000, 0.8660254037844387076, 1.000000000000000000, 0.8660254037844387076, 1.000000000000000000, 0.8660254037844387076, 1.000000000000000000, 0.8660254037844387076, 1.000000000000000000, 0.8660254037844387076, 1.000000000000000000, 0.8660254037844387076, 1.000000000000000000, 0.8660254037844387076, 1.000000000000000000, 0.8660254037844387076, 1.000000000000000000, 0.8660254037844387076, 1.000000000000000000, 0.8660254037844387076, 1.000000000000000000, 0.8660254037844387076, 1.000000000000000000, 0.8660254037844387076, 1.000000000000000000, 0.8660254037844387076, 1.000000000000000000, 0.8660254037844387076, 1.000000000000000000, 0.8660254037844387076, 1.000000000000000000, 0.8660254037844387076, 1.000000000000000000, 0.8660254037844387076, 1.000000000000000000, 0.8660254037844387076, 1.000000000000000000, 0.8660254037844387076, 1.000000000000000000, 0.8660254037844387076, 1.000000000000000000, 0.8660254037844387076, 1.000000000000000000, 0.8660254037844387076, 1.000000000000000000, 0.8660254037844387076, 1.000000000000000000, 0.8660254037844387076, 1.000000000000000000, 0.8660254037844387076, 1.000000000000000000, 0.8660254037844387076, 1.000000000000000000, 0.8660254037844387076, 1.000000000000000000, 0.8660254037844387076, 1.000000000000000000, 0.8660254037844387076, 1.000000000000000000, 0.8660254037844387076, 1.000000000000000000, 0.8660254037844387076, 1.000000000000000000, 0.8660254037844387076, 1.000000000000000000, 0.8660254037844387076, 1.000000000000000000, 0.8660254037844387076, 1.000000000000000000, 0.8660254037844387076, 1.000000000000000000, 0.8660254037844387076, 1.000000000000000000, 0.8660254037844387076, 1.000000000000000000, 0.8660254037844387076, 1.000000000000000000, 0.8660254037844387076, 1.000000000000000000, 0.8660254037844387076, 1.000000000000000000, 0.8660254037844387076, 1.000000000000000000, 0.8660254037844387076, 1.000000000000000000, 0.8660254037844387076, 1.000000000000000000, 0.8660254037844387076, 1.000000000000000000, 0.8660254037844387076, 1.000000000000000000, 0.8660254037844387076, 1.000000000000000000, 0.8660254037844387076, 1.000000000000000000),
 ( 1.000000000000000000, 0.8660254037844387076, 1.000000000000000000, 0.8660254037844387076, 1.000000000000000000, 0.8660254037844387076, 1.000000000000000000, 0.8660254037844387076, 1.000000000000000000, 0.8660254037844387076, 1.000000000000000000, 0.8660254037844387076, 1.000000000000000000, 0.8660254037844387076, 1.000000000000000000, 0.8660254037844387076, 1.000000000000000000, 0.8660254037844387076, 1.000000000000000000, 0.8660254037844387076, 1.000000000000000000, 0.8660254037844387076, 1.000000000000000000, 0.8660254037844387076, 1.000000000000000000, 0.8660254037844387076, 1.000000000000000000, 0.8660254037844387076, 1.000000000000000000, 0.8660254037844387076, 1.000000000000000000, 0.8660254037844387076, 1.000000000000000000, 0.8660254037844387076, 1.000000000000000000, 0.8660254037844387076, 1.000000000000000000, 0.8660254037844387076, 1.000000000000000000, 0.8660254037844387076, 1.000000000000000000, 0.8660254037844387076, 1.000000000000000000, 0.8660254037844387076, 1.000000000000000000, 0.8660254037844387076, 1.000000000000000000, 0.8660254037844387076, 1.000000000000000000, 0.8660254037844387076, 1.000000000000000000, 0.8660254037844387076, 1.000000000000000000, 0.8660254037844387076, 1.000000000000000000, 0.8660254037844387076, 1.000000000000000000, 0.8660254037844387076, 1.000000000000000000, 0.8660254037844387076, 1.000000000000000000, 0.8660254037844387076, 1.000000000000000000, 0.8660254037844387076, 1.000000000000000000, 0.8660254037844387076, 1.000000000000000000, 0.8660254037844387076, 1.000000000000000000, 0.8660254037844387076, 1.000000000000000000, 0.8660254037844387076, 1.000000000000000000, 0.8660254037844387076, 1.000000000000000000, 0.8660254037844387076, 1.000000000000000000, 0.8660254037844387076, 1.000000000000000000, 0.8660254037844387076, 1.000000000000000000, 0.8660254037844387076, 1.000000000000000000, 0.8660254037844387076, 1.000000000000000000, 0.8660254037844387076, 1.000000000000000000, 0.8660254037844387076, 1.000000000000000000, 0.8660254037844387076, 1.000000000000000000, 0.8660254037844387076, 1.000000000000000000, 0.8660254037844387076, 1.000000000000000000, 0.8660254037844387076, 1.000000000000000000, 0.8660254037844387076, 1.000000000000000000, 0.8660254037844387076, 1.000000000000000000, 0.8660254037844387076, 1.000000000000000000, 0.8660254037844387076, 1.000000000000000000, 0.8660254037844387076, 1.000000000000000000, 0.8660254037844387076, 1.000000000000000000, 0.8660254037844387076, 1.000000000000000000, 0.8660254037844387076, 1.000000000000000000, 0.8660254037844387076, 1.000000000000000000, 0.8660254037844387076, 1.000000000000000000, 0.8660254037844387076, 1.000000000000000000, 0.8660254037844387076, 1.000000000000000000, 0.8660254037844387076, 1.000000000000000000, 0.8660254037844387076, 1.000000000000000000, 0.8660254037844387076, 1.000000000000000000, 0.8660254037844387076, 1.000000000000000000, 0.8660254037844387076, 1.000000000000000000, 0.8660254037844387076, 1.000000000000000000, 0.8660254037844387076, 1.000000000000000000, 0.8660254037844387076, 1.000000000000000000, 0.8660254037844387076, 1.000000000000000000, 0.8660254037844387076, 1.000000000000000000, 0.8660254037844387076, 1.000000000000000000, 0.8660254037844387076, 1.000000000000000000, 0.8660254037844387076, 1.000000000000000000, 0.8660254037844387076, 1.000000000000000000, 0.8660254037844387076, 1.000000000000000000, 0.8660254037844387076, 1.000000000000000000, 0.8660254037844387076, 1.000000000000000000, 0.8660254037844387076, 1.000000000000000000, 0.8660254037844387076, 1.000000000000000000, 0.8660254037844387076, 1.000000000000000000, 0.8660254037844387076, 1.000000000000000000, 0.8660254037844387076, 1.000000000000000000, 0.8660254037844387076, 1.000000000000000000, 0.8660254037844387076, 1.000000000000000000, 0.8660254037844387076, 1.000000000000000000, 0.8660254037844387076, 1.000000000000000000, 0.8660254037844387076, 1.000000000000000000, 0.8660254037844387076, 1.000000000000000000, 0.8660254037844387076, 1.000000000000000000, 0.8660254037844387076, 1.000000000000000000, 0.8660254037844387076, 1.000000000000000000, 0.8660254037844387076, 1.000000000000000000, 0.8660254037844387076, 1.000000000000000000, 0.8660254037844387076, 1.000000000000000000, 0.8660254037844387076, 1.000000000000000000, 0.8660254037844387076, 1.000000000000000000, 0.8660254037844387076, 1.000000000000000000, 0.8660254037844387076, 1.000000000000000000, 0.8660254037844387076, 1.000000000000000000, 0.8660254037844387076, 1.000000000000000000, 0.8660254037844387076, 1.000000000000000000, 0.8660254037844387076, 1.000000000000000000, 0.8660254037844387076, 1.000000000000000000, 0.8660254037844387076, 1.000000000000000000, 0.8660254037844387076, 1.000000000000000000, 0.8660254037844387076, 1.000000000000000000, 0.8660254037844387076, 1.000000000000000000, 0.8660254037844387076, 1.000000000000000000, 0.8660254037844387076, 1.000000000000000000, 0.8660254037844387076, 1.000000000000000000, 0.8660254037844387076, 1.000000000000000000, 0.8660254037844387076, 1.000000000000000000, 0.8660254037844387076, 1.000000000000000000, 0.8660254037844387076, 1.000000000000000000, 0.8660254037844387076, 1.000000000000000000, 0.8660254037844387076, 1.000000000000000000, 0.8660254037844387076, 1.000000000000000000, 0.8660254037844387076, 1.000000000000000000, 0.8660254037844387076, 1.000000000000000000, 0.8660254037844387076, 1.000000000000000000, 0.8660254037844387076, 1.000000000000000000, 0.8660254037844387076, 1.000000000000000000, 0.8660254037844387076, 1.000000000000000000, 0.8660254037844387076, 1.000000000000000000, 0.8660254037844387076, 1.000000000000000000, 0.8660254037844387076, 1.000000000000000000, 0.8660254037844387076, 1.000000000000000000, 0.8660254037844387076, 1.000000000000000000, 0.8660254037844387076, 1.000000000000000000, 0.8660254037844387076, 1.000000000000000000, 0.8660254037844387076, 1.000000000000000000, 0.8660254037844387076, 1.000000000000000000, 0.8660254037844387076, 1.000000000000000000, 0.8660254037844387076, 1.000000000000000000, 0.8660254037844387076, 1.000000000000000000, 0.8660254037844387076, 1.000000000000000000, 0.8660254037844387076, 1.000000000000000000, 0.8660254037844387076, 1.000000000000000000, 0.8660254037844387076, 1.000000000000000000, 0.8660254037844387076, 1.000000000000000000, 0.8660254037844387076, 1.000000000000000000, 0.8660254037844387076, 1.000000000000000000, 0.8660254037844387076, 1.000000000000000000, 0.8660254037844387076, 1.000000000000000000, 0.8660254037844387076, 1.000000000000000000, 0.8660254037844387076, 1.000000000000000000, 0.8660254037844387076, 1.000000000000000000, 0.8660254037844387076, 1.000000000000000000, 0.8660254037844387076, 1.000000000000000000, 0.8660254037844387076, 1.000000000000000000, 0.8660254037844387076, 1.000000000000000000, 0.8660254037844387076, 1.000000000000000000, 0.8660254037844387076, 1.000000000000000000, 0.8660254037844387076, 1.000000000000000000, 0.8660254037844387076, 1.000000000000000000, 0.8660254037844387076, 1.000000000000000000, 0.8660254037844387076, 1.000000000000000000, 0.8660254037844387076, 1.000000000000000000, 0.8660254037844387076, 1.000000000000000000, 0.8660254037844387076, 1.000000000000000000, 0.8660254037844387076, 1.000000000000000000, 0.8660254037844387076, 1.000000000000000000, 0.8660254037844387076, 1.000000000000000000, 0.8660254037844387076, 1.000000000000000000, 0.8660254037844387076, 1.000000000000000000, 0.8660254037844387076, 1.000000000000000000, 0.8660254037844387076, 1.000000000000000000, 0.8660254037844387076, 1.000000000000000000, 0.8660254037844387076, 1.000000000000000000, 0.8660254037844387076, 1.000000000000000000, 0.8660254037844387076, 1.000000000000000000, 0.8660254037844387076, 1.000000000000000000, 0.8660254037844387076, 1.000000000000000000, 0.8660254037844387076, 1.000000000000000000, 0.8660254037844387076, 1.000000000000000000, 0.8660254037844387076, 1.000000000000000000, 0.8660254037844387076, 1.000000000000000000, 0.8660254037844387076, 1.000000000000000000, 0.8660254037844387076, 1.000000000000000000, 0.8660254037844387076, 1.000000000000000000, 0.8660254037844387076, 1.000000000000000000, 0.8660254037844387076, 1.000000000000000000, 0.8660254037844387076, 1.000000000000000000, 0.8660254037844387076, 1.000000000000000000, 0.8660254037844387076, 1.000000000000000000, 0.8660254037844387076, 1.000000000000000000, 0.8660254037844387076, 1.000000000000000000, 0.8660254037844387076, 1.000000000000000000, 0.8660254037844387076, 1.000000000000000000, 0.8660254037844387076, 1.000000000000000000, 0.8660254037844387076, 1.000000000000000000, 0.8660254037844387076, 1.000000000000000000, 0.8660254037844387076, 1.000000000000000000, 0.8660254037844387076, 1.000000000000000000, 0.8660254037844387076, 1.000000000000000000, 0.8660254037844387076, 1.000000000000000000, 0.8660254037844387076, 1.000000000000000000, 0.8660254037844387076, 1.000000000000000000, 0.8660254037844387076, 1.000000000000000000, 0.8660254037844387076, 1.000000000000000000, 0.8660254037844387076, 1.000000000000000000, 0.8660254037844387076, 1.000000000000000000, 0.8660254037844387076, 1.000000000000000000, 0.8660254037844387076, 1.000000000000000000, 0.8660254037844387076, 1.000000000000000000, 0.8660254037844387076, 1.000000000000000000, 0.8660254037844387076, 1.000000000000000000, 0.8660254037844387076, 1.000000000000000000, 0.8660254037844387076, 1.000000000000000000, 0.8660254037844387076, 1.000000000000000000, 0.8660254037844387076, 1.000000000000000000, 0.8660254037844387076, 1.000000000000000000, 0.8660254037844387076, 1.000000000000000000, 0.8660254037844387076, 1.000000000000000000, 0.8660254037844387076, 1.000000000000000000, 0.8660254037844387076, 1.000000000000000000, 0.8660254037844387076, 1.000000000000000000, 0.8660254037844387076, 1.000000000000000000, 0.8660254037844387076, 1.000000000000000000, 0.8660254037844387076, 1.000000000000000000, 0.8660254037844387076, 1.000000000000000000, 0.8660254037844387076, 1.000000000000000000, 0.8660254037844387076, 1.000000000000000000, 0.8660254037844387076, 1.000000000000000000, 0.8660254037844387076, 1.000000000000000000, 0.8660254037844387076, 1.000000000000000000, 0.8660254037844387076, 1.000000000000000000, 0.8660254037844387076, 1.000000000000000000, 0.8660254037844387076, 1.000000000000000000, 0.8660254037844387076, 1.000000000000000000, 0.8660254037844387076, 1.000000000000000000, 0.8660254037844387076, 1.000000000000000000, 0.8660254037844387076, 1.000000000000000000, 0.8660254037844387076, 1.000000000000000000, 0.8660254037844387076, 1.000000000000000000, 0.8660254037844387076, 1.000000000000000000, 0.8660254037844387076, 1.000000000000000000, 0.8660254037844387076, 1.000000000000000000, 0.8660254037844387076, 1.000000000000000000, 0.8660254037844387076, 1.000000000000000000, 0.8660254037844387076, 1.000000000000000000, 0.8660254037844387076, 1.000000000000000000, 0.8660254037844387076, 1.000000000000000000, 0.8660254037844387076, 1.000000000000000000, 0.8660254037844387076, 1.000000000000000000, 0.8660254037844387076, 1.000000000000000000, 0.8660254037844387076, 1.000000000000000000, 0.8660254037844387076, 1.000000000000000000, 0.8660254037844387076, 1.000000000000000000, 0.8660254037844387076, 1.000000000000000000, 0.8660254037844387076, 1.000000000000000000, 0.8660254037844387076, 1.000000000000000000, 0.8660254037844387076, 1.000000000000000000, 0.8660254037844387076, 1.000000000000000000, 0.8660254037844387076, 1.000000000000000000, 0.8660254037844387076, 1.000000000000000000, 0.8660254037844387076, 1.000000000000000000, 0.8660254037844387076, 1.000000000000000000, 0.8660254037844387076, 1.000000000000000000, 0.8660254037844387076, 1.000000000000000000, 0.8660254037844387076, 1.000000000000000000, 0.8660254037844387076, 1.000000000000000000, 0.8660254037844387076, 1.000000000000000000, 0.8660254037844387076, 1.000000000000000000, 0.8660254037844387076, 1.000000000000000000, 0.8660254037844387076, 1.000000000000000000, 0.8660254037844387076, 1.000000000000000000, 0.8660254037844387076, 1.000000000000000000, 0.8660254037844387076, 1.000000000000000000, 0.8660254037844387076, 1.000000000000000000, 0.8660254037844387076, 1.000000000000000000, 0.8660254037844387076, 1.000000000000000000, 0.8660254037844387076, 1.000000000000000000, 0.8660254037844387076, 1.000000000000000000, 0.8660254037844387076, 1.000000000000000000, 0.8660254037844387076, 1.000000000000000000, 0.8660254037844387076, 1.000000000000000000, 0.8660254037844387076, 1.000000000000000000, 0.8660254037844387076, 1.000000000000000000, 0.8660254037844387076, 1.000000000000000000, 0.8660254037844387076, 1.000000000000000000, 0.8660254037844387076, 1.000000000000000000, 0.8660254037844387076, 1.000000000000000000, 0.8660254037844387076, 1.000000000000000000, 0.8660254037844387076, 1.000000000000000000, 0.8660254037844387076, 1.000000000000000000, 0.8660254037844387076, 1.000000000000000000, 0.8660254037844387076, 1.000000000000000000, 0.8660254037844387076, 1.000000000000000000, 0.8660254037844387076, 1.000000000000000000, 0.8660254037844387076, 1.000000000000000000, 0.8660254037844387076, 1.000000000000000000, 0.8660254037844387076, 1.000000000000000000, 0.8660254037844387076, 1.000000000000000000, 0.8660254037844387076, 1.000000000000000000, 0.8660254037844387076, 1.000000000000000000, 0.8660254037844387076, 1.000000000000000000, 0.8660254037844387076, 1.000000000000000000, 0.8660254037844387076, 1.000000000000000000, 0.8660254037844387076, 1.000000000000000000) ) ) 
 REPRESENTATION_ITEM ( '' )  SURFACE ( )  );
#67015 = CARTESIAN_POINT ( 'NONE',  ( 27.02812500061451573, 4.541064518000418104, 2.621784821874999949 ) ) ;
#67017 = CARTESIAN_POINT ( 'NONE',  ( 26.42812500061451431, 6.421520780324663323E-16, -5.243569643749999010 ) ) ;
#67018 = DIRECTION ( 'NONE',  ( 0.000000000000000000, 0.000000000000000000, 1.000000000000000000 ) ) ;
#67019 = CARTESIAN_POINT ( 'NONE',  ( 3.999999999999998668, 17.11250000000000071, 27.69059892324149175 ) ) ;
#67020 = CARTESIAN_POINT ( 'NONE',  ( 4.134375000614517681, 4.541064518000418104, 2.621784821874999949 ) ) ;
#67021 = CONTEXT_DEPENDENT_SHAPE_REPRESENTATION ( #66786, #20779 ) ;
#67022 = CARTESIAN_POINT ( 'NONE',  ( 11.96250000122903501, 4.330127018922192761, -2.499999999999997780 ) ) ;
#67023 = CARTESIAN_POINT ( 'NONE',  ( 7.875000001229034652, 2.886751345948129099, -4.999999999999998224 ) ) ;
#67024 = CARTESIAN_POINT ( 'NONE',  ( 29.55000000122903003, 5.773502691896255534, 3.535250795749688894E-16 ) ) ;
#67025 = CARTESIAN_POINT ( 'NONE',  ( 2.000000000000000444, 18.81874999877096499, 26.53589838486224650 ) ) ;
#67026 = CARTESIAN_POINT ( 'NONE',  ( 19.21875000122902932, 2.886751345948126879, 4.999999999999999112 ) ) ;
#67027 = CARTESIAN_POINT ( 'NONE',  ( 12.57187500061451857, 3.027376345333613106, -5.243569643749998122 ) ) ;
#67028 = CARTESIAN_POINT ( 'NONE',  ( 3.999999999999998668, 12.91249999999999964, 32.30940107675850470 ) ) ;
#67029 = ORIENTED_EDGE ( 'NONE', *, *, #6241, .T. ) ;
#67030 = CARTESIAN_POINT ( 'NONE',  ( 20.35312500061451502, 0.000000000000000000, 5.243569643749999010 ) ) ;
#67031 = CARTESIAN_POINT ( 'NONE',  ( 14.14687500061451786, -3.027376345333614438, 5.243569643749998122 ) ) ;
#67032 = CARTESIAN_POINT ( 'NONE',  ( 4.828125000614518214, 6.421520780324663323E-16, -5.243569643749999010 ) ) ;
#67033 = CARTESIAN_POINT ( 'NONE',  ( 21.75937500061451502, 0.000000000000000000, 5.243569643749999010 ) ) ;
#67034 = CARTESIAN_POINT ( 'NONE',  ( 9.721875000614517148, -6.054752690667223547, -1.112240025338166033E-15 ) ) ;
#67035 = CARTESIAN_POINT ( 'NONE',  ( 4.603125000614518569, 0.000000000000000000, 5.243569643749999010 ) ) ;
#67036 = CARTESIAN_POINT ( 'NONE',  ( 10.95000000122903216, -2.886751345948126435, -5.000000000000000000 ) ) ;
#67037 = CARTESIAN_POINT ( 'NONE',  ( 5.362500001229033586, 0.000000000000000000, 4.999999999999998224 ) ) ;
#67038 = CARTESIAN_POINT ( 'NONE',  ( 19.45312500061451644, 0.000000000000000000, 5.243569643749999010 ) ) ;
#67039 =( BOUNDED_CURVE ( )  B_SPLINE_CURVE ( 2, ( #43440, #49347, #67442, #38245, #27543, #5009, #10907 ),
 .UNSPECIFIED., .F., .F. ) 
 B_SPLINE_CURVE_WITH_KNOTS ( ( 3, 2, 2, 3 ),
 ( 0.3666666666666666408, 0.3694444444444444642, 0.3722222222222222321, 0.3750000000000000000 ),
 .UNSPECIFIED. ) 
 CURVE ( )  GEOMETRIC_REPRESENTATION_ITEM ( )  RATIONAL_B_SPLINE_CURVE ( ( 1.000000000000000000, 0.8660254037844387076, 1.000000000000000000, 0.8660254037844387076, 1.000000000000000000, 0.8660254037844387076, 1.000000000000000000 ) ) 
 REPRESENTATION_ITEM ( '' )  );
#67040 = CARTESIAN_POINT ( 'NONE',  ( 8.662500001229034297, -4.330127018922190985, -2.500000000000001332 ) ) ;
#67041 = CARTESIAN_POINT ( 'NONE',  ( 17.61562500061451786, 3.027376345333611329, 5.243569643749999010 ) ) ;
#67042 = CARTESIAN_POINT ( 'NONE',  ( 16.04062500061451857, -3.027376345333610441, -5.243569643749999898 ) ) ;
#67043 = CARTESIAN_POINT ( 'NONE',  ( 26.25937500061451857, 0.000000000000000000, 4.756430356249998326 ) ) ;
#67044 = CARTESIAN_POINT ( 'NONE',  ( 16.57499999999999929, -4.330127018922194537, 2.499999999999995559 ) ) ;
#67045 = CARTESIAN_POINT ( 'NONE',  ( 9.787500001229036073, 4.330127018922191873, 2.499999999999999556 ) ) ;
#67046 = CARTESIAN_POINT ( 'NONE',  ( 8.503125000614515372, 4.541064518000418104, -2.621784821874998173 ) ) ;
#67047 = CARTESIAN_POINT ( 'NONE',  ( 11.76562500061451644, 3.027376345333611329, 5.243569643749999010 ) ) ;
#67048 = EDGE_CURVE ( 'NONE', #45011, #71132, #43864, .T. ) ;
#67049 = CARTESIAN_POINT ( 'NONE',  ( 20.70000000122903216, -2.886751345948129988, 4.999999999999997335 ) ) ;
#67050 = CARTESIAN_POINT ( 'NONE',  ( 27.22499999999999787, 4.330127018922191873, 2.499999999999999556 ) ) ;
#67051 = CARTESIAN_POINT ( 'NONE',  ( -2.121784821874996840, 14.53437500061451715, -26.32496088578401583 ) ) ;
#67052 = FACE_OUTER_BOUND ( 'NONE', #67666, .T. ) ;
#67053 = CARTESIAN_POINT ( 'NONE',  ( 3.112500001229034918, 0.000000000000000000, 4.999999999999998224 ) ) ;
#67054 = CARTESIAN_POINT ( 'NONE',  ( 3.309375000614518836, 0.000000000000000000, 5.243569643749999010 ) ) ;
#67055 = CARTESIAN_POINT ( 'NONE',  ( 20.74687500061451573, 6.054752690667223547, 3.707466751127219781E-16 ) ) ;
#67056 = CARTESIAN_POINT ( 'NONE',  ( 8.662499999999997868, 2.886751345948073588, -5.000000000000094147 ) ) ;
#67057 = CARTESIAN_POINT ( 'NONE',  ( 16.41562500061451857, -6.054752690667223547, -1.112240025338166033E-15 ) ) ;
#67058 = CARTESIAN_POINT ( 'NONE',  ( 12.43125000122903145, 4.330127018922191873, 2.499999999999999556 ) ) ;
#67059 = CARTESIAN_POINT ( 'NONE',  ( 1.626862140677534273E-15, 15.61250000000000071, -26.00000000000000355 ) ) ;
#67060 = CARTESIAN_POINT ( 'NONE',  ( 4.385796401931335353, -2.400997692794667682, 4.385796401931427724 ) ) ;
#67061 = CARTESIAN_POINT ( 'NONE',  ( 29.40937500061451715, 0.000000000000000000, 5.243569643749999010 ) ) ;
#67062 = CARTESIAN_POINT ( 'NONE',  ( 21.45937500061451786, 2.746126346562645981, -4.756430356249997438 ) ) ;
#67063 = CARTESIAN_POINT ( 'NONE',  ( 13.82812500061451466, 6.421520780324663323E-16, -5.243569643749999010 ) ) ;
#67064 = CARTESIAN_POINT ( 'NONE',  ( 11.89687500061451608, -3.027376345333614438, 5.243569643749998122 ) ) ;
#67065 = EDGE_LOOP ( 'NONE', ( #37653, #41154, #21941, #51619 ) ) ;
#67066 = CARTESIAN_POINT ( 'NONE',  ( 29.05312500061451431, -4.541064518000417216, -2.621784821875001281 ) ) ;
#67067 = CARTESIAN_POINT ( 'NONE',  ( 22.49062500061451431, 6.054752690667223547, 3.707466751127219781E-16 ) ) ;
#67068 = CARTESIAN_POINT ( 'NONE',  ( 3.999999999999998668, 11.26250000000000107, -32.30940107675850470 ) ) ;
#67069 = CARTESIAN_POINT ( 'NONE',  ( 13.35000000000000142, 0.000000000000000000, 4.999999999999998224 ) ) ;
#67070 = CARTESIAN_POINT ( 'NONE',  ( 22.23750000122903003, 6.123233995736764310E-16, -4.999999999999998224 ) ) ;
#67071 = CARTESIAN_POINT ( 'NONE',  ( 16.34062500061451573, -3.027376345333614438, 5.243569643749998122 ) ) ;
#67072 = CARTESIAN_POINT ( 'NONE',  ( 11.78437500061451360, -2.746126346562646425, 4.756430356249996549 ) ) ;
#67073 = EDGE_LOOP ( 'NONE', ( #63093, #51604, #5634, #36043 ) ) ;
#67074 = CARTESIAN_POINT ( 'NONE',  ( 20.73750000000000071, -2.886751345948125991, -5.000000000000000000 ) ) ;
#67075 = CARTESIAN_POINT ( 'NONE',  ( 21.12187500061451573, 3.027376345333613106, -5.243569643749998122 ) ) ;
#67076 = CARTESIAN_POINT ( 'NONE',  ( 26.80312500061451431, -4.541064518000417216, -2.621784821875001281 ) ) ;
#67077 = ORIENTED_EDGE ( 'NONE', *, *, #12941, .F. ) ;
#67078 = CARTESIAN_POINT ( 'NONE',  ( 34.99999999999999289, -4.500000000000000000, 3.499999999999999556 ) ) ;
#67079 = CARTESIAN_POINT ( 'NONE',  ( 11.31562500061451892, 3.027376345333611329, 5.243569643749999010 ) ) ;
#67080 = CARTESIAN_POINT ( 'NONE',  ( 6.225000000000001421, -4.330127018922194537, 2.499999999999995559 ) ) ;
#67081 = CARTESIAN_POINT ( 'NONE',  ( 16.53750000000000142, -2.886751345948129988, 4.999999999999997335 ) ) ;
#67082 = CARTESIAN_POINT ( 'NONE',  ( 23.66250000000000142, 2.886751345948126879, 4.999999999999999112 ) ) ;
#67083 = CARTESIAN_POINT ( 'NONE',  ( 7.800000000000001599, 4.330127018922192761, -2.499999999999997780 ) ) ;
#67084 = CARTESIAN_POINT ( 'NONE',  ( 5.409375000614516260, 4.541064518000418104, -2.621784821874998173 ) ) ;
#67085 = CARTESIAN_POINT ( 'NONE',  ( 29.37187500061451928, 3.027376345333611329, 5.243569643749999010 ) ) ;
#67086 = ORIENTED_EDGE ( 'NONE', *, *, #47391, .T. ) ;
#67087 = CARTESIAN_POINT ( 'NONE',  ( 23.24062500061451786, -3.027376345333610441, -5.243569643749999898 ) ) ;
#67088 = CARTESIAN_POINT ( 'NONE',  ( 25.58437500061451431, 6.421520780324663323E-16, -5.243569643749999010 ) ) ;
#67089 = CARTESIAN_POINT ( 'NONE',  ( 4.243569643749999898, 19.54062500061459318, -27.54997392385601529 ) ) ;
#67090 = CARTESIAN_POINT ( 'NONE',  ( 13.98750000000000249, -2.886751345948125991, -5.000000000000000000 ) ) ;
#67091 = CARTESIAN_POINT ( 'NONE',  ( 7.828125000614517326, -4.541064518000419881, 2.621784821874995952 ) ) ;
#67092 = CARTESIAN_POINT ( 'NONE',  ( 1.999999999999997335, 17.31874999877096499, 33.46410161513775705 ) ) ;
#67093 = CARTESIAN_POINT ( 'NONE',  ( 26.35312500061451857, -4.541064518000417216, -2.621784821875001281 ) ) ;
#67094 = CARTESIAN_POINT ( 'NONE',  ( 15.63750000122903216, 4.330127018922191873, 2.499999999999999556 ) ) ;
#67095 = CARTESIAN_POINT ( 'NONE',  ( -3.999999999999999112, 18.19999999999999929, 30.00000000000000000 ) ) ;
#67096 = CARTESIAN_POINT ( 'NONE',  ( 16.02187500061451786, -5.492252693125287522, -1.008910452111647106E-15 ) ) ;
#67097 = CARTESIAN_POINT ( 'NONE',  ( 3.890625000614517326, -3.027376345333610441, -5.243569643749999898 ) ) ;
#67098 = CARTESIAN_POINT ( 'NONE',  ( 19.20937500061451786, -4.541064518000417216, -2.621784821875001281 ) ) ;
#67099 = CARTESIAN_POINT ( 'NONE',  ( 2.121784821874999061, 13.85937500061451821, 26.32496088578401583 ) ) ;
#67100 = CARTESIAN_POINT ( 'NONE',  ( 21.83437500061451786, -4.541064518000419881, 2.621784821874995952 ) ) ;
#67101 = CARTESIAN_POINT ( 'NONE',  ( 28.47187500061451715, 3.027376345333611329, 5.243569643749999010 ) ) ;
#67102 = CARTESIAN_POINT ( 'NONE',  ( 10.49999999999999822, 4.330127018922192761, -2.499999999999997780 ) ) ;
#67103 = CARTESIAN_POINT ( 'NONE',  ( 10.79062500061451679, 6.054752690667223547, 3.707466751127219781E-16 ) ) ;
#67104 = CARTESIAN_POINT ( 'NONE',  ( -3.999999999999997335, 15.20000000122903572, 32.30940107675850470 ) ) ;
#67105 = ADVANCED_FACE ( 'NONE', ( #49304 ), #9769, .F. ) ;
#67106 = CARTESIAN_POINT ( 'NONE',  ( 6.271875000614517859, 3.027376345333613106, -5.243569643749998122 ) ) ;
#67107 = DIRECTION ( 'NONE',  ( -0.000000000000000000, -1.000000000000000000, -0.000000000000000000 ) ) ;
#67108 = ADVANCED_FACE ( 'NONE', ( #43761 ), #27137, .F. ) ;
#67109 = CARTESIAN_POINT ( 'NONE',  ( 7.528125000614515727, 6.421520780324663323E-16, -5.243569643749999010 ) ) ;
#67110 = CARTESIAN_POINT ( 'NONE',  ( 11.44687500061451857, -3.027376345333614438, 5.243569643749998122 ) ) ;
#67111 = CARTESIAN_POINT ( 'NONE',  ( 19.42500000122903714, -5.773502691896255534, -1.060575238724906372E-15 ) ) ;
#67112 = CARTESIAN_POINT ( 'NONE',  ( 8.034375000614518925, 6.421520780324663323E-16, -5.243569643749999010 ) ) ;
#67113 = CARTESIAN_POINT ( 'NONE',  ( 10.71562500061451928, 3.027376345333613106, -5.243569643749998122 ) ) ;
#67114 = CARTESIAN_POINT ( 'NONE',  ( 6.140625000614516438, -3.027376345333610441, -5.243569643749999898 ) ) ;
#67115 = CARTESIAN_POINT ( 'NONE',  ( 25.33125000122903003, 6.123233995736764310E-16, -4.999999999999998224 ) ) ;
#67116 = CARTESIAN_POINT ( 'NONE',  ( 18.45937500061451431, 4.541064518000418104, -2.621784821874998173 ) ) ;
#67117 = CARTESIAN_POINT ( 'NONE',  ( 11.10000000000000142, 0.000000000000000000, 4.999999999999998224 ) ) ;
#67118 = CARTESIAN_POINT ( 'NONE',  ( 27.81562500061452070, 3.027376345333613106, -5.243569643749998122 ) ) ;
#67119 = CARTESIAN_POINT ( 'NONE',  ( 12.62812500061451537, 4.541064518000418104, 2.621784821874999949 ) ) ;
#67120 = CARTESIAN_POINT ( 'NONE',  ( 28.84687500061452425, 6.054752690667223547, 3.707466751127219781E-16 ) ) ;
#67121 = CARTESIAN_POINT ( 'NONE',  ( 9.001249775931846008E-16, 13.22187500061451892, -25.09994784771203058 ) ) ;
#67122 = ADVANCED_FACE ( 'NONE', ( #66286 ), #15664, .T. ) ;
#67123 = CARTESIAN_POINT ( 'NONE',  ( 14.06250000122903288, -4.330127018922190985, -2.500000000000001332 ) ) ;
#67124 = CARTESIAN_POINT ( 'NONE',  ( 4.243569643749999010, 16.01562500061451644, -32.45002607614398471 ) ) ;
#67125 = CARTESIAN_POINT ( 'NONE',  ( 14.10000000122903252, -2.886751345948125991, -5.000000000000000000 ) ) ;
#67126 = CARTESIAN_POINT ( 'NONE',  ( 9.215625000614515727, -6.054752690667223547, -1.112240025338166033E-15 ) ) ;
#67127 = CARTESIAN_POINT ( 'NONE',  ( 12.82499999999999929, 4.330127018922191873, 2.499999999999999556 ) ) ;
#67128 = CARTESIAN_POINT ( 'NONE',  ( -5.810221930991193690E-16, 13.58750000000000036, -34.00000000000000000 ) ) ;
#67129 = CARTESIAN_POINT ( 'NONE',  ( 23.50312500061451360, 0.000000000000000000, 5.243569643749999010 ) ) ;
#67130 = CARTESIAN_POINT ( 'NONE',  ( 7.321875000614516793, 3.027376345333611329, 5.243569643749999010 ) ) ;
#67131 = ADVANCED_FACE ( 'NONE', ( #55572 ), #50034, .F. ) ;
#67132 = CARTESIAN_POINT ( 'NONE',  ( 9.900000001229033231, -2.886751345948129988, 4.999999999999997335 ) ) ;
#67133 = CARTESIAN_POINT ( 'NONE',  ( 17.40000000122903145, 5.773502691896255534, 3.535250795749688894E-16 ) ) ;
#67134 = CARTESIAN_POINT ( 'NONE',  ( 14.50312500061451537, 0.000000000000000000, 5.243569643749999010 ) ) ;
#67135 = CARTESIAN_POINT ( 'NONE',  ( 18.06562500061451715, 3.027376345333611329, 5.243569643749999010 ) ) ;
#67136 = CARTESIAN_POINT ( 'NONE',  ( 25.50000000122903288, 5.773502691896255534, 3.535250795749688894E-16 ) ) ;
#67137 = CARTESIAN_POINT ( 'NONE',  ( 28.57500000122903572, 2.886751345948129099, -4.999999999999998224 ) ) ;
#67138 = CARTESIAN_POINT ( 'NONE',  ( 22.68750000000000000, 5.773502691896255534, 3.535250795749688894E-16 ) ) ;
#67139 = CARTESIAN_POINT ( 'NONE',  ( -3.756430356249999214, 13.72812499938548392, 27.83122392262697531 ) ) ;
#67140 = CARTESIAN_POINT ( 'NONE',  ( 25.95937500061451431, -4.541064518000417216, -2.621784821875001281 ) ) ;
#67141 = CARTESIAN_POINT ( 'NONE',  ( 45.00000000000000000, 0.000000000000000000, 0.000000000000000000 ) ) ;
#67142 = CARTESIAN_POINT ( 'NONE',  ( 11.40000000122903501, -2.886751345948125991, -5.000000000000000000 ) ) ;
#67143 = CARTESIAN_POINT ( 'NONE',  ( 27.75937500061451502, -4.541064518000417216, -2.621784821875001281 ) ) ;
#67144 = CARTESIAN_POINT ( 'NONE',  ( 3.889232029978275662, 3.142875762045684418, 3.889232029978275662 ) ) ;
#67145 = CARTESIAN_POINT ( 'NONE',  ( 4.134375000614517681, 4.541064518000418104, 2.621784821874999949 ) ) ;
#67146 = CARTESIAN_POINT ( 'NONE',  ( 23.95312500061451289, 0.000000000000000000, 5.243569643749999010 ) ) ;
#67147 = CARTESIAN_POINT ( 'NONE',  ( -3.756430356250000102, 14.77812499938548463, 30.00000000000000000 ) ) ;
#67148 = CARTESIAN_POINT ( 'NONE',  ( 4.586250975554630571, -1.994072912278271881, -4.586250975554630571 ) ) ;
#67149 = CARTESIAN_POINT ( 'NONE',  ( 9.496875000614517504, 6.054752690667223547, 3.707466751127219781E-16 ) ) ;
#67150 = CARTESIAN_POINT ( 'NONE',  ( 2.393811435568372112E-14, 16.88750000000000284, 34.00000000000000000 ) ) ;
#67151 = CARTESIAN_POINT ( 'NONE',  ( 29.39062500061451289, -3.027376345333614438, 5.243569643749998122 ) ) ;
#67152 = CARTESIAN_POINT ( 'NONE',  ( 7.396875000614519635, -3.027376345333614438, 5.243569643749998122 ) ) ;
#67153 = CARTESIAN_POINT ( 'NONE',  ( 29.78437500061451715, 4.541064518000418104, 2.621784821874999949 ) ) ;
#67154 = CARTESIAN_POINT ( 'NONE',  ( 28.96875000122903288, 2.886751345948158409, -4.999999999999947597 ) ) ;
#67155 = CARTESIAN_POINT ( 'NONE',  ( 20.21250000000000213, -5.773502691896255534, -1.060575238724906372E-15 ) ) ;
#67156 = EDGE_LOOP ( 'NONE', ( #16289, #45158, #28888, #60027 ) ) ;
#67157 = CARTESIAN_POINT ( 'NONE',  ( 27.03750000000000142, -2.886751345948125991, -5.000000000000000000 ) ) ;
#67158 = CARTESIAN_POINT ( 'NONE',  ( 29.70937500061451431, 4.541064518000418104, -2.621784821874998173 ) ) ;
#67159 = EDGE_LOOP ( 'NONE', ( #30343, #56692, #70072 ) ) ;
#67160 = CARTESIAN_POINT ( 'NONE',  ( 17.50312500061451715, 4.541064518000418104, -2.621784821874998173 ) ) ;
#67161 = CARTESIAN_POINT ( 'NONE',  ( 8.915625000614515017, 3.027376345333613106, -5.243569643749998122 ) ) ;
#67162 = CARTESIAN_POINT ( 'NONE',  ( 21.15937500061451715, 2.746126346562643317, 4.756430356249998326 ) ) ;
#67163 = CARTESIAN_POINT ( 'NONE',  ( 4.059375000614519280, 4.541064518000418104, -2.621784821874998173 ) ) ;
#67164 = CARTESIAN_POINT ( 'NONE',  ( 18.63750000122903216, 6.123233995736764310E-16, -4.999999999999998224 ) ) ;
#67165 = CARTESIAN_POINT ( 'NONE',  ( 0.000000000000000000, 20.00000000000000000, -33.99999999999999289 ) ) ;
#67166 = CARTESIAN_POINT ( 'NONE',  ( 7.809375000614519280, 0.000000000000000000, 5.243569643749999010 ) ) ;
#67167 = CARTESIAN_POINT ( 'NONE',  ( 11.78437500061451892, 4.541064518000418104, 2.621784821874999949 ) ) ;
#67168 = CARTESIAN_POINT ( 'NONE',  ( 21.75937500061451502, 0.000000000000000000, 5.243569643749999010 ) ) ;
#67169 = CARTESIAN_POINT ( 'NONE',  ( 4.423774761630055785, -2.331624301134462396, 4.423774761630055785 ) ) ;
#67170 = ORIENTED_EDGE ( 'NONE', *, *, #49427, .F. ) ;
#67171 = CARTESIAN_POINT ( 'NONE',  ( 4.884375000614518569, 6.421520780324663323E-16, -5.243569643749999010 ) ) ;
#67172 = CARTESIAN_POINT ( 'NONE',  ( 11.02500000000000036, 4.330127018922191873, 2.499999999999999556 ) ) ;
#67173 = CARTESIAN_POINT ( 'NONE',  ( 7.471875000614519813, -6.054752690667223547, -1.112240025338166033E-15 ) ) ;
#67174 = CARTESIAN_POINT ( 'NONE',  ( -1.878215178125001827, 16.09062499938548285, 33.25316411605952283 ) ) ;
#67175 = CARTESIAN_POINT ( 'NONE',  ( 21.63749999999999929, -2.886751345948125991, -5.000000000000000000 ) ) ;
#67176 = CARTESIAN_POINT ( 'NONE',  ( 17.35312500061451502, -4.541064518000417216, -2.621784821875001281 ) ) ;
#67177 = CARTESIAN_POINT ( 'NONE',  ( -1.999999999999999112, 18.05000000000000071, 26.53589838486224650 ) ) ;
#67178 = CARTESIAN_POINT ( 'NONE',  ( 4.182001429795429104, 2.740687966149290222, 4.445321778319560657 ) ) ;
#67179 = CARTESIAN_POINT ( 'NONE',  ( 22.02187500061452141, 2.746126346562645981, -4.756430356249997438 ) ) ;
#67180 = CARTESIAN_POINT ( 'NONE',  ( 11.24062500061451608, 6.054752690667223547, 3.707466751127219781E-16 ) ) ;
#67181 = CARTESIAN_POINT ( 'NONE',  ( 3.187500000000002220, -2.886751345948125991, -5.000000000000000000 ) ) ;
#67182 = CARTESIAN_POINT ( 'NONE',  ( 12.82499999999999929, 4.330127018922191873, 2.499999999999999556 ) ) ;
#67183 = CARTESIAN_POINT ( 'NONE',  ( 29.70937500061451431, 4.541064518000418104, -2.621784821874998173 ) ) ;
#67184 = CARTESIAN_POINT ( 'NONE',  ( 9.337500000000000355, -2.886751345948129988, 4.999999999999997335 ) ) ;
#67185 = CARTESIAN_POINT ( 'NONE',  ( 8.484601909799253346E-16, 14.82500000122903216, 34.61880215351700230 ) ) ;
#67186 = CARTESIAN_POINT ( 'NONE',  ( 10.01250000122903394, -4.330127018922190985, -2.500000000000001332 ) ) ;
#67187 = CARTESIAN_POINT ( 'NONE',  ( 19.20937500061451786, -4.541064518000417216, -2.621784821875001281 ) ) ;
#67188 = CARTESIAN_POINT ( 'NONE',  ( 14.37187500061451928, 3.027376345333613106, -5.243569643749998122 ) ) ;
#67189 = CARTESIAN_POINT ( 'NONE',  ( -1.999999999999997113, 12.42500000000000249, 33.46410161513775705 ) ) ;
#67190 = ORIENTED_EDGE ( 'NONE', *, *, #43763, .T. ) ;
#67191 = CARTESIAN_POINT ( 'NONE',  ( 14.76562500061451821, 3.027376345333613106, -5.243569643749998122 ) ) ;
#67192 = CARTESIAN_POINT ( 'NONE',  ( 26.85000000122903430, 5.773502691896255534, 3.535250795749688894E-16 ) ) ;
#67193 = CARTESIAN_POINT ( 'NONE',  ( 16.24687500061451573, 6.054752690667223547, 3.707466751127219781E-16 ) ) ;
#67194 = CARTESIAN_POINT ( 'NONE',  ( 8.175000000000002487, 6.123233995736764310E-16, -4.999999999999998224 ) ) ;
#67195 = CARTESIAN_POINT ( 'NONE',  ( 16.75312500061451715, 0.000000000000000000, 5.243569643749999010 ) ) ;
#67196 = CARTESIAN_POINT ( 'NONE',  ( 17.96250000122903501, 0.000000000000000000, 4.999999999999998224 ) ) ;
#67197 = CARTESIAN_POINT ( 'NONE',  ( 26.89687500061451431, -3.027376345333610441, -5.243569643749999898 ) ) ;
#67198 = CARTESIAN_POINT ( 'NONE',  ( 4.243569643749999898, 11.47812500061451679, 30.00000000000000000 ) ) ;
#67199 = CARTESIAN_POINT ( 'NONE',  ( 15.49687500061451750, -3.027376345333614438, 5.243569643749998122 ) ) ;
#67200 = CARTESIAN_POINT ( 'NONE',  ( 15.30000000122903359, -2.886751345948129988, 4.999999999999997335 ) ) ;
#67201 = CARTESIAN_POINT ( 'NONE',  ( 8.709375000614517859, 0.000000000000000000, 4.756430356249998326 ) ) ;
#67202 = CARTESIAN_POINT ( 'NONE',  ( 3.354550016499390441, -3.707702085728201702, 3.707832566801417595 ) ) ;
#67203 = EDGE_CURVE ( 'NONE', #15264, #36412, #69740, .T. ) ;
#67204 = CARTESIAN_POINT ( 'NONE',  ( 20.63437500061451857, 6.421520780324663323E-16, -5.243569643749999010 ) ) ;
#67205 = CARTESIAN_POINT ( 'NONE',  ( 18.97500000122903074, -5.773502691896255534, -1.060575238724906372E-15 ) ) ;
#67206 = CARTESIAN_POINT ( 'NONE',  ( 16.73437500061451644, 4.541064518000418104, 2.621784821874999949 ) ) ;
#67207 = CARTESIAN_POINT ( 'NONE',  ( 2.121784821874999061, 12.95937500061451786, 26.32496088578401583 ) ) ;
#67208 = CARTESIAN_POINT ( 'NONE',  ( 18.32812500061451644, 6.421520780324663323E-16, -5.243569643749999010 ) ) ;
#67209 = ORIENTED_EDGE ( 'NONE', *, *, #17293, .F. ) ;
#67210 = ORIENTED_EDGE ( 'NONE', *, *, #39975, .T. ) ;
#67211 = CARTESIAN_POINT ( 'NONE',  ( 20.92500000000000071, 4.330127018922191873, 2.499999999999999556 ) ) ;
#67212 = FACE_OUTER_BOUND ( 'NONE', #3132, .T. ) ;
#67213 = CARTESIAN_POINT ( 'NONE',  ( 23.42812500061451786, 4.541064518000418104, 2.621784821874999949 ) ) ;
#67214 = CARTESIAN_POINT ( 'NONE',  ( 4.040625000614517681, 6.054752690667223547, 3.707466751127219781E-16 ) ) ;
#67215 = CARTESIAN_POINT ( 'NONE',  ( 18.15000000122903501, -2.886751345948125991, -5.000000000000000000 ) ) ;
#67216 = CARTESIAN_POINT ( 'NONE',  ( 22.34062500061451573, -3.027376345333610441, -5.243569643749999898 ) ) ;
#67217 = CARTESIAN_POINT ( 'NONE',  ( 21.63749999999999929, -2.886751345948125991, -5.000000000000000000 ) ) ;
#67218 = CARTESIAN_POINT ( 'NONE',  ( 24.74062500061451786, 6.054752690667223547, 3.707466751127219781E-16 ) ) ;
#67219 = CARTESIAN_POINT ( 'NONE',  ( 5.990625000614517859, -3.027376345333614438, 5.243569643749998122 ) ) ;
#67220 = ORIENTED_EDGE ( 'NONE', *, *, #64836, .F. ) ;
#67221 = CARTESIAN_POINT ( 'NONE',  ( 29.73750000000000071, -2.886751345948125991, -5.000000000000000000 ) ) ;
#67222 = CARTESIAN_POINT ( 'NONE',  ( 3.590625000614518836, 6.054752690667223547, 3.707466751127219781E-16 ) ) ;
#67223 = CARTESIAN_POINT ( 'NONE',  ( 11.59687500061451892, -2.746126346562642428, -4.756430356249999214 ) ) ;
#67224 = CARTESIAN_POINT ( 'NONE',  ( -1.999999999999997113, 11.18750000122903288, 33.46410161513775705 ) ) ;
#67225 = CARTESIAN_POINT ( 'NONE',  ( -3.999999999999999556, 12.42500000122903359, -32.30940107675850470 ) ) ;
#67226 = CARTESIAN_POINT ( 'NONE',  ( 2.121784821875001281, 18.65937500061451715, -26.32496088578401938 ) ) ;
#67227 = EDGE_CURVE ( 'NONE', #47560, #46789, #45111, .T. ) ;
#67228 = CARTESIAN_POINT ( 'NONE',  ( 9.262499999999999289, 2.886751345948126879, 4.999999999999999112 ) ) ;
#67229 =( BOUNDED_CURVE ( )  B_SPLINE_CURVE ( 2, ( #53103, #2499, #36478, #52743, #19105, #2148, #18382 ),
 .UNSPECIFIED., .F., .F. ) 
 B_SPLINE_CURVE_WITH_KNOTS ( ( 3, 2, 2, 3 ),
 ( 0.2750000000000000777, 0.2777777777777778456, 0.2805555555555556135, 0.2833333333333333814 ),
 .UNSPECIFIED. ) 
 CURVE ( )  GEOMETRIC_REPRESENTATION_ITEM ( )  RATIONAL_B_SPLINE_CURVE ( ( 0.9999999999999973355, 0.8660254037844413721, 1.000000000000000000, 0.8660254037844387076, 1.000000000000000000, 0.8660254037844360431, 1.000000000000002665 ) ) 
 REPRESENTATION_ITEM ( '' )  );
#67230 = CARTESIAN_POINT ( 'NONE',  ( 5.737500001229033586, 4.330127018922191873, 2.499999999999999556 ) ) ;
#67231 = CARTESIAN_POINT ( 'NONE',  ( 13.13437500061451857, 4.541064518000418104, 2.621784821874999949 ) ) ;
#67232 = CARTESIAN_POINT ( 'NONE',  ( 29.72812500061451502, 4.541064518000418104, 2.621784821874999949 ) ) ;
#67233 = CARTESIAN_POINT ( 'NONE',  ( 4.134375000614517681, 4.541064518000418104, 2.621784821874999949 ) ) ;
#67234 = CARTESIAN_POINT ( 'NONE',  ( 30.00000000000000000, 6.123233995736764310E-16, -4.999999999999998224 ) ) ;
#67235 = CARTESIAN_POINT ( 'NONE',  ( 5.857864376269046325, -9.999999999999998224, -5.857864376269046325 ) ) ;
#67236 = CARTESIAN_POINT ( 'NONE',  ( 9.609375000614518214, 0.000000000000000000, 5.243569643749999010 ) ) ;
#67237 = LINE ( 'NONE', #39149, #38348 ) ;
#67238 = EDGE_CURVE ( 'NONE', #56470, #9094, #22309, .T. ) ;
#67239 = CARTESIAN_POINT ( 'NONE',  ( 20.72812500061451502, 4.541064518000418104, 2.621784821874999949 ) ) ;
#67240 = CARTESIAN_POINT ( 'NONE',  ( -3.999999999999999112, 12.42500000122903536, -32.30940107675850470 ) ) ;
#67241 = CARTESIAN_POINT ( 'NONE',  ( 2.121784821875001281, 18.15312500061459389, 33.67503911421598417 ) ) ;
#67242 = CARTESIAN_POINT ( 'NONE',  ( 23.07187500061451857, 3.027376345333611329, 5.243569643749999010 ) ) ;
#67243 =( NAMED_UNIT ( * ) PLANE_ANGLE_UNIT ( ) SI_UNIT ( $, .RADIAN. ) );
#67244 = CARTESIAN_POINT ( 'NONE',  ( 2.840625000614518392, -3.027376345333614438, 5.243569643749998122 ) ) ;
#67245 = CARTESIAN_POINT ( 'NONE',  ( 19.35937500061451644, 2.746126346562643317, 4.756430356249998326 ) ) ;
#67246 = CARTESIAN_POINT ( 'NONE',  ( 24.14062500061451289, -3.027376345333610441, -5.243569643749999898 ) ) ;
#67247 = CARTESIAN_POINT ( 'NONE',  ( 14.72812500061451679, 6.421520780324663323E-16, -5.243569643749999010 ) ) ;
#67248 = CARTESIAN_POINT ( 'NONE',  ( 14.94375000122903252, -2.886751345948125991, -5.000000000000000000 ) ) ;
#67249 = CARTESIAN_POINT ( 'NONE',  ( 11.52187500061451608, -6.054752690667223547, -1.112240025338166033E-15 ) ) ;
#67250 = DIRECTION ( 'NONE',  ( 0.000000000000000000, 0.000000000000000000, -1.000000000000000000 ) ) ;
#67251 = CARTESIAN_POINT ( 'NONE',  ( 25.27500000122903145, -5.773502691896255534, -1.060575238724906372E-15 ) ) ;
#67252 = CARTESIAN_POINT ( 'NONE',  ( 4.584375000614516971, 4.541064518000418104, 2.621784821874999949 ) ) ;
#67253 = CARTESIAN_POINT ( 'NONE',  ( 14.78437500061451715, 6.421520780324663323E-16, -5.243569643749999010 ) ) ;
#67254 = CARTESIAN_POINT ( 'NONE',  ( 27.79687500061451999, -3.027376345333610441, -5.243569643749999898 ) ) ;
#67255 = DIRECTION ( 'NONE',  ( -0.000000000000000000, -1.000000000000000000, -0.000000000000000000 ) ) ;
#67256 = CARTESIAN_POINT ( 'NONE',  ( 17.39999999999999858, 0.000000000000000000, 4.999999999999998224 ) ) ;
#67257 = CARTESIAN_POINT ( 'NONE',  ( 24.75937500061451502, 4.541064518000418104, -2.621784821874998173 ) ) ;
#67258 = CARTESIAN_POINT ( 'NONE',  ( 16.58437500061451786, 6.421520780324663323E-16, -5.243569643749999010 ) ) ;
#67259 = CARTESIAN_POINT ( 'NONE',  ( -1.878215178124999163, 15.15312499938548285, 26.74683588394047007 ) ) ;
#67260 = CARTESIAN_POINT ( 'NONE',  ( 28.38749999999999929, -2.886751345948125991, -5.000000000000000000 ) ) ;
#67261 = CARTESIAN_POINT ( 'NONE',  ( 4.687500001229034652, 6.123233995736764310E-16, -4.999999999999998224 ) ) ;
#67262 = CARTESIAN_POINT ( 'NONE',  ( 5.700000000000000178, 0.000000000000000000, 4.999999999999998224 ) ) ;
#67263 = CARTESIAN_POINT ( 'NONE',  ( 7.959375000614516082, 2.746126346562645981, -4.756430356249997438 ) ) ;
#67264 = CARTESIAN_POINT ( 'NONE',  ( 19.41562500061451146, 3.027376345333611329, 5.243569643749999010 ) ) ;
#67265 = CARTESIAN_POINT ( 'NONE',  ( 8.962500000000002132, -5.773502691896255534, -1.060575238724906372E-15 ) ) ;
#67266 = CARTESIAN_POINT ( 'NONE',  ( 1.626862140677534273E-15, 14.26250000000000107, 34.00000000000000000 ) ) ;
#67267 = CARTESIAN_POINT ( 'NONE',  ( 16.35000000000000142, 4.330127018922192761, -2.499999999999997780 ) ) ;
#67268 = CARTESIAN_POINT ( 'NONE',  ( -4.243569643749999898, 11.66562500061451679, 27.54997392385601529 ) ) ;
#67269 = CARTESIAN_POINT ( 'NONE',  ( 1.071796769724500997, 18.25759618943233065, 33.99999999999999289 ) ) ;
#67270 = CARTESIAN_POINT ( 'NONE',  ( 19.68750000122903288, 4.330127018922191873, 2.499999999999999556 ) ) ;
#67271 = CARTESIAN_POINT ( 'NONE',  ( 7.285825576177820915E-16, 10.00000000000000000, 36.00000000000000000 ) ) ;
#67272 = CARTESIAN_POINT ( 'NONE',  ( 27.72187500061451715, -6.054752690667223547, -1.112240025338166033E-15 ) ) ;
#67273 = ORIENTED_EDGE ( 'NONE', *, *, #39819, .F. ) ;
#67274 = CARTESIAN_POINT ( 'NONE',  ( 16.00312500061451715, -4.541064518000417216, -2.621784821875001281 ) ) ;
#67275 = CARTESIAN_POINT ( 'NONE',  ( 23.12812500061451360, -4.541064518000419881, 2.621784821874995952 ) ) ;
#67276 = CARTESIAN_POINT ( 'NONE',  ( 22.09687500061451715, 6.054752690667223547, 3.707466751127219781E-16 ) ) ;
#67277 = CARTESIAN_POINT ( 'NONE',  ( 7.500000000000000000, 0.000000000000000000, 4.999999999999998224 ) ) ;
#67278 = CARTESIAN_POINT ( 'NONE',  ( 9.140625000614518214, -3.027376345333614438, 5.243569643749998122 ) ) ;
#67279 = CARTESIAN_POINT ( 'NONE',  ( 25.37812500061451715, -4.541064518000419881, 2.621784821874995952 ) ) ;
#67280 = CARTESIAN_POINT ( 'NONE',  ( 13.80937500061451750, -4.541064518000417216, -2.621784821875001281 ) ) ;
#67281 = CARTESIAN_POINT ( 'NONE',  ( 18.34687500061451715, -3.027376345333610441, -5.243569643749999898 ) ) ;
#67282 = CARTESIAN_POINT ( 'NONE',  ( 4.027635003466097707, 2.962795348797195416, -4.326299380533228600 ) ) ;
#67283 = CARTESIAN_POINT ( 'NONE',  ( -4.243569643749999898, 17.55312500061451786, 30.00000000000000000 ) ) ;
#67284 = CARTESIAN_POINT ( 'NONE',  ( 22.46250000122903501, 0.000000000000000000, 4.999999999999998224 ) ) ;
#67285 = CARTESIAN_POINT ( 'NONE',  ( 17.25937500061451502, 0.000000000000000000, 4.756430356249998326 ) ) ;
#67286 = CARTESIAN_POINT ( 'NONE',  ( 11.72812500061451857, 4.541064518000418104, 2.621784821874999949 ) ) ;
#67287 = CARTESIAN_POINT ( 'NONE',  ( 5.971875000614516260, 3.027376345333611329, 5.243569643749999010 ) ) ;
#67288 = CARTESIAN_POINT ( 'NONE',  ( 4.659375000614518925, 0.000000000000000000, 5.243569643749999010 ) ) ;
#67289 = VERTEX_POINT ( 'NONE', #52199 ) ;
#67290 = EDGE_CURVE ( 'NONE', #66820, #26491, #16433, .T. ) ;
#67291 = CARTESIAN_POINT ( 'NONE',  ( 28.88437500061451502, 4.541064518000418104, 2.621784821874999949 ) ) ;
#67292 = CARTESIAN_POINT ( 'NONE',  ( 18.96562500061451573, 3.027376345333611329, 5.243569643749999010 ) ) ;
#67293 = CARTESIAN_POINT ( 'NONE',  ( 3.890625000614517326, -3.027376345333610441, -5.243569643749999898 ) ) ;
#67294 = CARTESIAN_POINT ( 'NONE',  ( 27.70312500061451289, -4.541064518000417216, -2.621784821875001281 ) ) ;
#67295 = CARTESIAN_POINT ( 'NONE',  ( 23.14687500061451786, -3.027376345333614438, 5.243569643749998122 ) ) ;
#67296 = CARTESIAN_POINT ( 'NONE',  ( 18.44062500061451715, 6.054752690667223547, 3.707466751127219781E-16 ) ) ;
#67297 = CARTESIAN_POINT ( 'NONE',  ( -4.243569643749997233, 19.44687500061451502, 32.45002607614398471 ) ) ;
#67298 = CARTESIAN_POINT ( 'NONE',  ( 25.15312500061451217, 4.541064518000418104, -2.621784821874998173 ) ) ;
#67299 = CARTESIAN_POINT ( 'NONE',  ( 4.612500001229032698, -4.330127018922190985, -2.500000000000001332 ) ) ;
#67300 = ORIENTED_EDGE ( 'NONE', *, *, #51252, .F. ) ;
#67301 = CARTESIAN_POINT ( 'NONE',  ( 27.18750000000000000, 5.773502691896255534, 3.535250795749688894E-16 ) ) ;
#67302 = CARTESIAN_POINT ( 'NONE',  ( 3.999999999999999112, 14.82500000000000107, -30.00000000000000000 ) ) ;
#67303 = CARTESIAN_POINT ( 'NONE',  ( 3.756430356250000102, 17.70312499938548356, 30.00000000000000000 ) ) ;
#67304 = CARTESIAN_POINT ( 'NONE',  ( 5.559375000614517504, 0.000000000000000000, 5.243569643749999010 ) ) ;
#67305 = CARTESIAN_POINT ( 'NONE',  ( 11.61562500061451608, 3.027376345333613106, -5.243569643749998122 ) ) ;
#67306 = CARTESIAN_POINT ( 'NONE',  ( 7.134375000614516793, 6.421520780324663323E-16, -5.243569643749999010 ) ) ;
#67307 = CARTESIAN_POINT ( 'NONE',  ( 24.63750000122903216, 4.330127018922191873, 2.499999999999999556 ) ) ;
#67308 = CARTESIAN_POINT ( 'NONE',  ( 15.94687500061451502, -3.027376345333614438, 5.243569643749998122 ) ) ;
#67309 = CARTESIAN_POINT ( 'NONE',  ( 3.459375000614519635, -4.541064518000417216, -2.621784821875001281 ) ) ;
#67310 = CARTESIAN_POINT ( 'NONE',  ( 27.75000000000000000, 0.000000000000000000, 4.999999999999998224 ) ) ;
#67311 = CARTESIAN_POINT ( 'NONE',  ( 26.67187500061451644, 3.027376345333611329, 5.243569643749999010 ) ) ;
#67312 = CARTESIAN_POINT ( 'NONE',  ( 4.190625000614518925, -3.027376345333614438, 5.243569643749998122 ) ) ;
#67313 = CARTESIAN_POINT ( 'NONE',  ( 12.66562500061451502, 3.027376345333611329, 5.243569643749999010 ) ) ;
#67314 = ORIENTED_EDGE ( 'NONE', *, *, #46318, .F. ) ;
#67315 = CARTESIAN_POINT ( 'NONE',  ( 9.590625000614517504, -3.027376345333614438, 5.243569643749998122 ) ) ;
#67316 = CARTESIAN_POINT ( 'NONE',  ( 6.815625000614517148, 3.027376345333611329, 5.243569643749999010 ) ) ;
#67317 = CARTESIAN_POINT ( 'NONE',  ( 18.60937500061451644, 0.000000000000000000, 4.756430356249998326 ) ) ;
#67318 = CARTESIAN_POINT ( 'NONE',  ( 0.000000000000000000, 20.00000000000000000, -30.00000000000000000 ) ) ;
#67319 = CARTESIAN_POINT ( 'NONE',  ( 15.41250000000000142, 2.886751345948129099, -4.999999999999998224 ) ) ;
#67320 = CARTESIAN_POINT ( 'NONE',  ( 15.83437500061451608, 4.541064518000418104, 2.621784821874999949 ) ) ;
#67321 = CARTESIAN_POINT ( 'NONE',  ( 13.76250000122903394, 4.330127018922192761, -2.499999999999997780 ) ) ;
#67322 = CARTESIAN_POINT ( 'NONE',  ( 19.42499999999999716, 6.123233995736764310E-16, -4.999999999999998224 ) ) ;
#67323 = CARTESIAN_POINT ( 'NONE',  ( 19.95937500061451786, 0.000000000000000000, 5.243569643749999010 ) ) ;
#67324 = CARTESIAN_POINT ( 'NONE',  ( -3.000416591977282496E-16, 13.84062500061451928, -34.90005215228797653 ) ) ;
#67325 = FACE_OUTER_BOUND ( 'NONE', #5322, .T. ) ;
#67326 = CARTESIAN_POINT ( 'NONE',  ( 26.48437500061450933, 5.492252693125287522, 3.363034840372157021E-16 ) ) ;
#67327 = CARTESIAN_POINT ( 'NONE',  ( 20.66250000000000142, -5.773502691896255534, -1.060575238724906372E-15 ) ) ;
#67328 = EDGE_CURVE ( 'NONE', #60454, #20630, #1348, .T. ) ;
#67329 = CARTESIAN_POINT ( 'NONE',  ( 26.39062500061451644, -3.027376345333610441, -5.243569643749999898 ) ) ;
#67330 = CARTESIAN_POINT ( 'NONE',  ( 2.000000000000001332, 16.10000000000000142, -26.53589838486224650 ) ) ;
#67331 = CARTESIAN_POINT ( 'NONE',  ( 25.61250000000000071, -5.773502691896255534, -1.060575238724906372E-15 ) ) ;
#67332 = CARTESIAN_POINT ( 'NONE',  ( 10.26562500061451644, 3.027376345333613106, -5.243569643749998122 ) ) ;
#67333 = CARTESIAN_POINT ( 'NONE',  ( 28.39687500061451431, 0.000000000000000000, 4.756430356249998326 ) ) ;
#67334 = CARTESIAN_POINT ( 'NONE',  ( 20.59687500061451360, -3.027376345333610441, -5.243569643749999898 ) ) ;
#67335 = CARTESIAN_POINT ( 'NONE',  ( 14.67187500061451644, 5.824947211148865298E-16, -4.756430356249998326 ) ) ;
#67336 = CARTESIAN_POINT ( 'NONE',  ( 4.453125000614517326, 4.541064518000418104, -2.621784821874998173 ) ) ;
#67337 = CARTESIAN_POINT ( 'NONE',  ( 11.37187500061451750, 3.027376345333611329, 5.243569643749999010 ) ) ;
#67338 = VERTEX_POINT ( 'NONE', #17481 ) ;
#67339 = CARTESIAN_POINT ( 'NONE',  ( 20.70937500061451786, 4.541064518000418104, -2.621784821874998173 ) ) ;
#67340 = FACE_OUTER_BOUND ( 'NONE', #2762, .T. ) ;
#67341 = CARTESIAN_POINT ( 'NONE',  ( 29.77499999999999858, 6.123233995736764310E-16, -4.999999999999998224 ) ) ;
#67342 = CARTESIAN_POINT ( 'NONE',  ( 4.387500000000002842, -2.886751345948129988, 4.999999999999997335 ) ) ;
#67343 = CARTESIAN_POINT ( 'NONE',  ( 15.67500000122903181, 2.886751345948126879, 4.999999999999999112 ) ) ;
#67344 = CARTESIAN_POINT ( 'NONE',  ( 20.83125000122903359, 6.123233995736764310E-16, -4.999999999999998224 ) ) ;
#67345 = CARTESIAN_POINT ( 'NONE',  ( -1.999999999999997113, 19.17500000000000071, -26.53589838486224295 ) ) ;
#67346 = VERTEX_POINT ( 'NONE', #62911 ) ;
#67347 = CARTESIAN_POINT ( 'NONE',  ( 12.48750000000000249, -2.886751345948129988, 4.999999999999997335 ) ) ;
#67348 = CARTESIAN_POINT ( 'NONE',  ( 27.55312500061451786, 0.000000000000000000, 5.243569643749999010 ) ) ;
#67349 = CARTESIAN_POINT ( 'NONE',  ( 16.98750000000000426, -2.886751345948129988, 4.999999999999997335 ) ) ;
#67350 = CARTESIAN_POINT ( 'NONE',  ( 9.562500001229032875, -4.330127018922190985, -2.500000000000001332 ) ) ;
#67351 = CARTESIAN_POINT ( 'NONE',  ( 8.015625000614518214, 3.027376345333613106, -5.243569643749998122 ) ) ;
#67352 = CARTESIAN_POINT ( 'NONE',  ( 8.587500000000002132, -2.886751345948125991, -5.000000000000000000 ) ) ;
#67353 = CARTESIAN_POINT ( 'NONE',  ( 1.626862140677534273E-15, 11.11250000000000071, -26.00000000000000355 ) ) ;
#67354 = CARTESIAN_POINT ( 'NONE',  ( 2.121784821874999061, 14.75937500061451679, -33.67503911421598417 ) ) ;
#67355 = CARTESIAN_POINT ( 'NONE',  ( 27.45000000122903572, -2.886751345948129988, 4.999999999999997335 ) ) ;
#67356 = CARTESIAN_POINT ( 'NONE',  ( -7.967954043666661671E-16, 15.22812499938548392, 34.33755215474603517 ) ) ;
#67357 = CARTESIAN_POINT ( 'NONE',  ( 7.237500000000000711, -2.886751345948125991, -5.000000000000000000 ) ) ;
#67358 = DIRECTION ( 'NONE',  ( -1.000000000000000000, -0.000000000000000000, -0.000000000000000000 ) ) ;
#67359 = VERTEX_POINT ( 'NONE', #57727 ) ;
#67360 = CARTESIAN_POINT ( 'NONE',  ( 24.10312500061451502, -4.541064518000417216, -2.621784821875001281 ) ) ;
#67361 = CARTESIAN_POINT ( 'NONE',  ( 29.20312500061451644, 4.541064518000418104, -2.621784821874998173 ) ) ;
#67362 = CARTESIAN_POINT ( 'NONE',  ( 29.25937500061451502, 4.541064518000418104, -2.621784821874998173 ) ) ;
#67363 = CARTESIAN_POINT ( 'NONE',  ( 22.50937500061451857, 4.541064518000418104, -2.621784821874998173 ) ) ;
#67364 = CARTESIAN_POINT ( 'NONE',  ( 15.59062500061451573, -3.027376345333610441, -5.243569643749999898 ) ) ;
#67365 = CARTESIAN_POINT ( 'NONE',  ( -4.243569643749999898, 11.70312500061459282, -30.00000000000000000 ) ) ;
#67366 = CARTESIAN_POINT ( 'NONE',  ( 7.340625000614518392, -3.027376345333614438, 5.243569643749998122 ) ) ;
#67367 = CARTESIAN_POINT ( 'NONE',  ( 28.08750000122903145, 6.123233995736764310E-16, -4.999999999999998224 ) ) ;
#67368 = CARTESIAN_POINT ( 'NONE',  ( 23.37187500061451573, 2.746126346562645981, -4.756430356249997438 ) ) ;
#67369 = CARTESIAN_POINT ( 'NONE',  ( 18.47812500061451857, 4.541064518000418104, 2.621784821874999949 ) ) ;
#67370 = DIRECTION ( 'NONE',  ( 1.000000000000000000, 0.000000000000000000, 0.000000000000000000 ) ) ;
#67371 = CARTESIAN_POINT ( 'NONE',  ( -3.756430356250000102, 19.61562499938548143, 30.00000000000000000 ) ) ;
#67372 = CARTESIAN_POINT ( 'NONE',  ( 11.59687500061451892, -3.027376345333610441, -5.243569643749999898 ) ) ;
#67373 = CARTESIAN_POINT ( 'NONE',  ( 14.97187500061451892, 3.027376345333611329, 5.243569643749999010 ) ) ;
#67374 = CARTESIAN_POINT ( 'NONE',  ( 22.58437500061451431, 4.541064518000418104, 2.621784821874999949 ) ) ;
#67375 = VERTEX_POINT ( 'NONE', #6775 ) ;
#67376 = CARTESIAN_POINT ( 'NONE',  ( 20.06250000000000000, 2.886751345948126879, 4.999999999999998224 ) ) ;
#67377 = CARTESIAN_POINT ( 'NONE',  ( 25.82812500061451644, -4.541064518000419881, 2.621784821874995952 ) ) ;
#67378 = EDGE_CURVE ( 'NONE', #31619, #14728, #19214, .T. ) ;
#67379 = CARTESIAN_POINT ( 'NONE',  ( 27.85312500061451502, 4.541064518000418104, -2.621784821874998173 ) ) ;
#67380 = CARTESIAN_POINT ( 'NONE',  ( -2.672702088255949472E-15, 13.06250000000000355, 26.00000000000000000 ) ) ;
#67381 = CARTESIAN_POINT ( 'NONE',  ( -2.000000000000000000, 15.87500000000000000, 26.53589838486224650 ) ) ;
#67382 = CARTESIAN_POINT ( 'NONE',  ( 4.434375000614519280, 6.421520780324663323E-16, -5.243569643749999010 ) ) ;
#67383 = CARTESIAN_POINT ( 'NONE',  ( 12.00000000122903465, 5.773502691896255534, 3.535250795749688894E-16 ) ) ;
#67384 = CARTESIAN_POINT ( 'NONE',  ( 6.862500001229034474, -4.330127018922190985, -2.500000000000001332 ) ) ;
#67385 = CARTESIAN_POINT ( 'NONE',  ( 29.58750000122903501, 4.330127018922191873, 2.499999999999999556 ) ) ;
#67386 = CARTESIAN_POINT ( 'NONE',  ( -1.999999999999999112, 18.44374999877096499, 26.53589838486224650 ) ) ;
#67387 = CARTESIAN_POINT ( 'NONE',  ( 19.14375000122903003, 5.773502691896255534, 3.535250795749688894E-16 ) ) ;
#67388 = CARTESIAN_POINT ( 'NONE',  ( 11.18437500061451928, 6.421520780324663323E-16, -5.243569643749999010 ) ) ;
#67389 = CARTESIAN_POINT ( 'NONE',  ( 4.000000000000000000, 12.98749999999999893, 27.69059892324149885 ) ) ;
#67390 = VERTEX_POINT ( 'NONE', #11597 ) ;
#67391 = CARTESIAN_POINT ( 'NONE',  ( 20.57812500061451644, 6.421520780324663323E-16, -5.243569643749999010 ) ) ;
#67392 = CARTESIAN_POINT ( 'NONE',  ( 12.90937500061451537, -4.541064518000417216, -2.621784821875001281 ) ) ;
#67393 = CARTESIAN_POINT ( 'NONE',  ( 4.303125000614516971, -4.541064518000417216, -2.621784821875001281 ) ) ;
#67394 = CARTESIAN_POINT ( 'NONE',  ( 22.17187500061451644, 3.027376345333611329, 5.243569643749999010 ) ) ;
#67395 = CARTESIAN_POINT ( 'NONE',  ( 9.684375000614517504, -4.541064518000419881, 2.621784821874995952 ) ) ;
#67396 = CARTESIAN_POINT ( 'NONE',  ( 4.528125000614516615, 4.541064518000418104, 2.621784821874999949 ) ) ;
#67397 = CARTESIAN_POINT ( 'NONE',  ( 5.810221930991193690E-16, 14.41249999999999787, 26.00000000000000000 ) ) ;
#67398 =( BOUNDED_CURVE ( )  B_SPLINE_CURVE ( 2, ( #34823, #17464, #50741, #5676, #865, #6393, #16742 ),
 .UNSPECIFIED., .F., .F. ) 
 B_SPLINE_CURVE_WITH_KNOTS ( ( 3, 2, 2, 3 ),
 ( 0.6400000000000001243, 0.6433333333333334236, 0.6466666666666666119, 0.6500000000000000222 ),
 .UNSPECIFIED. ) 
 CURVE ( )  GEOMETRIC_REPRESENTATION_ITEM ( )  RATIONAL_B_SPLINE_CURVE ( ( 0.9999999999999955591, 0.8660254037844431485, 1.000000000000000000, 0.8660254037844387076, 1.000000000000000000, 0.8660254037844387076, 1.000000000000000000 ) ) 
 REPRESENTATION_ITEM ( '' )  );
#67399 = CARTESIAN_POINT ( 'NONE',  ( 6.037500001229035185, 6.123233995736764310E-16, -4.999999999999998224 ) ) ;
#67400 = CARTESIAN_POINT ( 'NONE',  ( 18.96562500061451573, 3.027376345333611329, 5.243569643749999010 ) ) ;
#67401 = CARTESIAN_POINT ( 'NONE',  ( 9.112500001229033586, -4.330127018922190985, -2.500000000000001332 ) ) ;
#67402 = CARTESIAN_POINT ( 'NONE',  ( 18.10312500061451502, 0.000000000000000000, 5.243569643749999010 ) ) ;
#67403 = CARTESIAN_POINT ( 'NONE',  ( 14.84062500061451750, 6.054752690667223547, 3.707466751127219781E-16 ) ) ;
#67404 = CARTESIAN_POINT ( 'NONE',  ( 26.82187500061451857, -5.492252693125287522, -1.008910452111647106E-15 ) ) ;
#67405 = CARTESIAN_POINT ( 'NONE',  ( 15.26249999999999929, -5.773502691896255534, -1.060575238724906372E-15 ) ) ;
#67406 = CARTESIAN_POINT ( 'NONE',  ( 8.400000001229035007, 5.773502691896255534, 3.535250795749688894E-16 ) ) ;
#67407 = CARTESIAN_POINT ( 'NONE',  ( 5.390625000614518214, 6.054752690667223547, 3.707466751127219781E-16 ) ) ;
#67408 = CARTESIAN_POINT ( 'NONE',  ( 19.95000000122903572, -2.886751345948125991, -5.000000000000000000 ) ) ;
#67409 = CARTESIAN_POINT ( 'NONE',  ( 25.87500000000000000, 4.330127018922191873, 2.499999999999999556 ) ) ;
#67410 = CARTESIAN_POINT ( 'NONE',  ( -2.121784821874996840, 10.03437500061451892, -26.32496088578401583 ) ) ;
#67411 = LINE ( 'NONE', #11249, #27699 ) ;
#67412 = CARTESIAN_POINT ( 'NONE',  ( 24.03750000000000142, 5.773502691896255534, 3.535250795749688401E-16 ) ) ;
#67413 = CARTESIAN_POINT ( 'NONE',  ( 3.159375000614518036, 4.541064518000418104, -2.621784821874998173 ) ) ;
#67414 = CARTESIAN_POINT ( 'NONE',  ( 21.72187500061451715, 3.027376345333611329, 5.243569643749999010 ) ) ;
#67415 = CARTESIAN_POINT ( 'NONE',  ( 45.00000000000000000, 6.123233995736764310E-16, -4.999999999999998224 ) ) ;
#67416 = CARTESIAN_POINT ( 'NONE',  ( 15.59062500061451573, -3.027376345333610441, -5.243569643749999898 ) ) ;
#67417 = CARTESIAN_POINT ( 'NONE',  ( 12.28125000122903110, 6.123233995736764310E-16, -4.999999999999998224 ) ) ;
#67418 = CARTESIAN_POINT ( 'NONE',  ( -2.498395430326213790E-14, 20.65624999877097068, 26.00000000000000000 ) ) ;
#67419 = CARTESIAN_POINT ( 'NONE',  ( 14.04375000122903216, -2.886751345948181946, -4.999999999999904077 ) ) ;
#67420 = CARTESIAN_POINT ( 'NONE',  ( 28.43437500061451573, 4.541064518000418104, 2.621784821874999949 ) ) ;
#67421 = CARTESIAN_POINT ( 'NONE',  ( 21.83437500061451786, -2.746126346562641984, -4.756430356249999214 ) ) ;
#67422 = CARTESIAN_POINT ( 'NONE',  ( 13.41562500061451502, 3.027376345333613106, -5.243569643749998122 ) ) ;
#67423 = CARTESIAN_POINT ( 'NONE',  ( 10.62187500061451928, -6.054752690667223547, -1.112240025338166033E-15 ) ) ;
#67424 = VERTEX_POINT ( 'NONE', #67397 ) ;
#67425 = CARTESIAN_POINT ( 'NONE',  ( 29.69062500061451715, 6.054752690667223547, 3.707466751127219781E-16 ) ) ;
#67426 = CARTESIAN_POINT ( 'NONE',  ( 23.87812500061451715, 4.541064518000418104, 2.621784821874999949 ) ) ;
#67427 = CARTESIAN_POINT ( 'NONE',  ( 17.73750000122903359, 6.123233995736764310E-16, -4.999999999999998224 ) ) ;
#67428 = CARTESIAN_POINT ( 'NONE',  ( -3.999999999999999112, 12.87500000122903465, 27.69059892324149885 ) ) ;
#67429 =( BOUNDED_CURVE ( )  B_SPLINE_CURVE ( 2, ( #9525, #54591, #65667, #66037, #26520, #49418, #49786, #59751, #67150 ),
 .UNSPECIFIED., .F., .F. ) 
 B_SPLINE_CURVE_WITH_KNOTS ( ( 3, 2, 2, 2, 3 ),
 ( 0.5138888888888889506, 0.5185185185185184897, 0.5277777777777777901, 0.5370370370370370905, 0.5416666666666667407 ),
 .UNSPECIFIED. ) 
 CURVE ( )  GEOMETRIC_REPRESENTATION_ITEM ( )  RATIONAL_B_SPLINE_CURVE ( ( 0.9330127018922192983, 0.9330127018922200755, 1.000000000000000000, 0.8660254037844387076, 1.000000000000000000, 0.8660254037844387076, 1.000000000000000000, 0.9330127018922185211, 0.9330127018922192983 ) ) 
 REPRESENTATION_ITEM ( '' )  );
#67430 = CARTESIAN_POINT ( 'NONE',  ( 12.56250000000000178, -5.773502691896255534, -1.060575238724906372E-15 ) ) ;
#67431 = CARTESIAN_POINT ( 'NONE',  ( 22.16250000122903074, -4.330127018922190985, -2.500000000000001332 ) ) ;
#67432 = CARTESIAN_POINT ( 'NONE',  ( 17.01562500061451644, 3.027376345333613106, -5.243569643749998122 ) ) ;
#67433 = CARTESIAN_POINT ( 'NONE',  ( 13.77187500061451431, 5.824947211148865298E-16, -4.756430356249998326 ) ) ;
#67434 = ORIENTED_EDGE ( 'NONE', *, *, #6454, .T. ) ;
#67435 = CARTESIAN_POINT ( 'NONE',  ( 18.86249999999999716, -5.773502691896255534, -1.060575238724906372E-15 ) ) ;
#67436 = CARTESIAN_POINT ( 'NONE',  ( 23.28750000000000142, -2.886751345948129988, 4.999999999999997335 ) ) ;
#67437 =( BOUNDED_CURVE ( )  B_SPLINE_CURVE ( 2, ( #30163, #34610, #57862, #2102, #69692, #12803, #52696 ),
 .UNSPECIFIED., .F., .F. ) 
 B_SPLINE_CURVE_WITH_KNOTS ( ( 3, 2, 2, 3 ),
 ( 0.8000000000000000444, 0.8033333333333333437, 0.8066666666666666430, 0.8100000000000000533 ),
 .UNSPECIFIED. ) 
 CURVE ( )  GEOMETRIC_REPRESENTATION_ITEM ( )  RATIONAL_B_SPLINE_CURVE ( ( 1.000000000000000000, 0.8660254037844387076, 1.000000000000000000, 0.8660254037844387076, 1.000000000000000000, 0.8660254037844387076, 1.000000000000000000 ) ) 
 REPRESENTATION_ITEM ( '' )  );
#67438 = CARTESIAN_POINT ( 'NONE',  ( 20.85937500061451644, 0.000000000000000000, 5.243569643749999010 ) ) ;
#67439 = CARTESIAN_POINT ( 'NONE',  ( 28.15312500061451573, -4.541064518000417216, -2.621784821875001281 ) ) ;
#67440 = ORIENTED_EDGE ( 'NONE', *, *, #32319, .F. ) ;
#67441 = ADVANCED_FACE ( 'NONE', ( #51119 ), #40041, .T. ) ;
#67442 = CARTESIAN_POINT ( 'NONE',  ( 20.02500000000000213, 4.330127018922191873, 2.499999999999999556 ) ) ;
#67443 = CARTESIAN_POINT ( 'NONE',  ( 8.315625000614515372, -6.054752690667223547, -1.112240025338166033E-15 ) ) ;
#67444 = CARTESIAN_POINT ( 'NONE',  ( 14.58750000000000036, 5.773502691896255534, 3.535250795749688894E-16 ) ) ;
#67445 = CARTESIAN_POINT ( 'NONE',  ( 4.243569643749999898, 19.54062500061451857, 32.45002607614398471 ) ) ;
#67446 = CARTESIAN_POINT ( 'NONE',  ( 5.334375000614517859, 6.421520780324663323E-16, -5.243569643749999010 ) ) ;
#67447 = CARTESIAN_POINT ( 'NONE',  ( 29.52187500061451431, -6.054752690667223547, -1.112240025338166033E-15 ) ) ;
#67448 = ORIENTED_EDGE ( 'NONE', *, *, #24383, .T. ) ;
#67449 = CARTESIAN_POINT ( 'NONE',  ( 25.11562500061451431, 3.027376345333613106, -5.243569643749998122 ) ) ;
#67450 = CARTESIAN_POINT ( 'NONE',  ( 26.14687500061451431, 6.054752690667223547, 3.707466751127219781E-16 ) ) ;
#67451 = CARTESIAN_POINT ( 'NONE',  ( 2.121784821874999061, 18.30312500061459247, -33.67503911421598417 ) ) ;
#67452 = CARTESIAN_POINT ( 'NONE',  ( 12.11250000000000249, -5.773502691896255534, -1.060575238724906372E-15 ) ) ;
#67453 = CARTESIAN_POINT ( 'NONE',  ( 9.928125000614517859, 4.541064518000418104, 2.621784821874999949 ) ) ;
#67454 = CARTESIAN_POINT ( 'NONE',  ( 0.3499497844256071466, 20.88781155722894312, 33.99999999999999289 ) ) ;
#67455 = CARTESIAN_POINT ( 'NONE',  ( 26.16562500061451502, 3.027376345333611329, 5.243569643749999010 ) ) ;
#67456 = CARTESIAN_POINT ( 'NONE',  ( -1.999999999999997113, 18.27499999999999858, 33.46410161513775705 ) ) ;
#67457 = CARTESIAN_POINT ( 'NONE',  ( 15.75937500061451857, 4.119189519843966529, -2.378215178124998275 ) ) ;
#67458 = CARTESIAN_POINT ( 'NONE',  ( 3.590625000614518836, 6.054752690667223547, 3.707466751127219781E-16 ) ) ;
#67459 = CARTESIAN_POINT ( 'NONE',  ( 19.80937500061451573, 4.541064518000418104, -2.621784821874998173 ) ) ;
#67460 = CARTESIAN_POINT ( 'NONE',  ( 2.121784821875001281, 15.50937500061451857, 33.67503911421598417 ) ) ;
#67461 = CARTESIAN_POINT ( 'NONE',  ( 21.57187500061451502, 3.027376345333613106, -5.243569643749998122 ) ) ;
#67462 = CARTESIAN_POINT ( 'NONE',  ( 29.29687500061451644, 6.054752690667223547, 3.707466751127219781E-16 ) ) ;
#67463 = CARTESIAN_POINT ( 'NONE',  ( -4.243569643749998122, 18.99687500061451928, 32.45002607614398471 ) ) ;
#67464 = CARTESIAN_POINT ( 'NONE',  ( 10.26562500061451644, 3.027376345333613106, -5.243569643749998122 ) ) ;
#67465 = CARTESIAN_POINT ( 'NONE',  ( 3.037500001229032964, 4.330127018922191873, 2.499999999999999556 ) ) ;
#67466 = EDGE_CURVE ( 'NONE', #68632, #8399, #29177, .T. ) ;
#67467 = CARTESIAN_POINT ( 'NONE',  ( 6.234375000614519102, 6.421520780324663323E-16, -5.243569643749999010 ) ) ;
#67468 = CARTESIAN_POINT ( 'NONE',  ( 11.68125000122903145, -4.330127018922194537, 2.499999999999995559 ) ) ;
#67469 = CARTESIAN_POINT ( 'NONE',  ( 6.740625000614516082, 6.054752690667223547, 3.707466751127219781E-16 ) ) ;
#67470 = CARTESIAN_POINT ( 'NONE',  ( 13.09687500061451892, 6.054752690667223547, 3.707466751127219781E-16 ) ) ;
#67471 = CARTESIAN_POINT ( 'NONE',  ( 18.30000000122903359, 5.773502691896255534, 3.535250795749688894E-16 ) ) ;
#67472 = CARTESIAN_POINT ( 'NONE',  ( 7.284375000614518036, 4.541064518000418104, 2.621784821874999949 ) ) ;
#67473 = CARTESIAN_POINT ( 'NONE',  ( 9.890625000614516438, 6.054752690667223547, 3.707466751127219781E-16 ) ) ;
#67474 = CARTESIAN_POINT ( 'NONE',  ( 5.278125000614516615, 6.421520780324663323E-16, -5.243569643749999010 ) ) ;
#67475 = CARTESIAN_POINT ( 'NONE',  ( 25.48125000122903216, 4.330127018922191873, 2.499999999999999556 ) ) ;
#67476 = CARTESIAN_POINT ( 'NONE',  ( 19.32187500061451857, 3.027376345333613106, -5.243569643749998122 ) ) ;
#67477 = CARTESIAN_POINT ( 'NONE',  ( -0.7368881354385758975, 9.803648613939513368, -34.17910028561248481 ) ) ;
#67478 = CARTESIAN_POINT ( 'NONE',  ( 27.29062500061451502, -3.027376345333610441, -5.243569643749999898 ) ) ;
#67479 = CARTESIAN_POINT ( 'NONE',  ( 12.51562500061451821, 3.027376345333613106, -5.243569643749998122 ) ) ;
#67480 = CARTESIAN_POINT ( 'NONE',  ( 28.24687500061451573, -3.027376345333610441, -5.243569643749999898 ) ) ;
#67481 = CARTESIAN_POINT ( 'NONE',  ( -2.121784821874999949, 11.68437500061451750, -33.67503911421598417 ) ) ;
#67482 = CARTESIAN_POINT ( 'NONE',  ( 12.03750000122903430, 4.330127018922191873, 2.499999999999999556 ) ) ;
#67483 = CARTESIAN_POINT ( 'NONE',  ( 27.17812500061451786, -4.541064518000419881, 2.621784821874995952 ) ) ;
#67484 = CARTESIAN_POINT ( 'NONE',  ( -3.000416591977282496E-16, 16.09062500061451573, -34.90005215228797653 ) ) ;
#67485 = CARTESIAN_POINT ( 'NONE',  ( 14.96250000122903323, -4.330127018922190985, -2.500000000000001332 ) ) ;
#67486 = CARTESIAN_POINT ( 'NONE',  ( 13.19999999999999929, 4.330127018922192761, -2.499999999999997780 ) ) ;
#67487 = CARTESIAN_POINT ( 'NONE',  ( 10.35000000122903074, -2.886751345948063374, 5.000000000000112799 ) ) ;
#67488 = CARTESIAN_POINT ( 'NONE',  ( 22.90312500061451573, 4.541064518000418104, -2.621784821874998173 ) ) ;
#67489 = CARTESIAN_POINT ( 'NONE',  ( 8.596875000614518925, 6.054752690667223547, 3.707466751127219781E-16 ) ) ;
#67490 = CARTESIAN_POINT ( 'NONE',  ( 8.887500001229033941, 4.330127018922191873, 2.499999999999999556 ) ) ;
#67491 = CARTESIAN_POINT ( 'NONE',  ( 16.72500000122903430, -5.773502691896255534, -1.060575238724906372E-15 ) ) ;
#67492 = CARTESIAN_POINT ( 'NONE',  ( 12.17812500061451608, 4.541064518000418104, 2.621784821874999949 ) ) ;
#67493 = CARTESIAN_POINT ( 'NONE',  ( 18.62812500061451715, -4.541064518000419881, 2.621784821874995952 ) ) ;
#67494 = CARTESIAN_POINT ( 'NONE',  ( 26.32500000122903216, 2.886751345948129099, -4.999999999999998224 ) ) ;
#67495 = CARTESIAN_POINT ( 'NONE',  ( 28.95000000122903572, -2.886751345948125991, -5.000000000000000000 ) ) ;
#67496 = CARTESIAN_POINT ( 'NONE',  ( 23.77499999999999858, -4.330127018922194537, 2.499999999999995559 ) ) ;
#67497 = CARTESIAN_POINT ( 'NONE',  ( 26.89687500061451431, -3.027376345333610441, -5.243569643749999898 ) ) ;
#67498 = DIRECTION ( 'NONE',  ( 0.000000000000000000, 0.000000000000000000, 1.000000000000000000 ) ) ;
#67499 = CARTESIAN_POINT ( 'NONE',  ( 9.262500001229033941, 4.330127018922192761, -2.499999999999997780 ) ) ;
#67500 = CARTESIAN_POINT ( 'NONE',  ( 28.73437500061451644, 6.421520780324663323E-16, -5.243569643749999010 ) ) ;
#67501 = CARTESIAN_POINT ( 'NONE',  ( 5.259375000614518569, -4.541064518000417216, -2.621784821875001281 ) ) ;
#67502 = CARTESIAN_POINT ( 'NONE',  ( 24.81562500061451715, 3.027376345333611329, 5.243569643749999010 ) ) ;
#67503 = CARTESIAN_POINT ( 'NONE',  ( 3.756430356250000546, 14.14062499938548356, 27.83122392262697886 ) ) ;
#67504 = CARTESIAN_POINT ( 'NONE',  ( 26.19375000122903074, -2.886751345948126435, -5.000000000000000000 ) ) ;
#67505 = CARTESIAN_POINT ( 'NONE',  ( 9.459375000614517859, 4.541064518000418104, -2.621784821874998173 ) ) ;
#67506 = CARTESIAN_POINT ( 'NONE',  ( 4.967063083088209652, -0.5913641066433281690, 5.048674133904348160 ) ) ;
#67507 = CARTESIAN_POINT ( 'NONE',  ( 3.534375000614518036, 6.421520780324663323E-16, -5.243569643749999010 ) ) ;
#67508 = CARTESIAN_POINT ( 'NONE',  ( 7.134375000614516793, 6.421520780324663323E-16, -5.243569643749999010 ) ) ;
#67509 = CARTESIAN_POINT ( 'NONE',  ( -1.999999999999997113, 16.58750000122903501, -26.53589838486224295 ) ) ;
#67510 = CARTESIAN_POINT ( 'NONE',  ( 28.69687500061451502, -3.027376345333610441, -5.243569643749999898 ) ) ;
#67511 = CARTESIAN_POINT ( 'NONE',  ( 2.121784821874999061, 10.20312500061459637, 26.32496088578401583 ) ) ;
#67512 = CARTESIAN_POINT ( 'NONE',  ( 18.86249999999999716, -5.773502691896255534, -1.060575238724906372E-15 ) ) ;
#67513 = ORIENTED_EDGE ( 'NONE', *, *, #31048, .T. ) ;
#67514 = CARTESIAN_POINT ( 'NONE',  ( 26.43750000000000000, -2.886751345948129988, 4.999999999999997335 ) ) ;
#67515 = CARTESIAN_POINT ( 'NONE',  ( 29.18437500061451573, 6.421520780324663323E-16, -5.243569643749999010 ) ) ;
#67516 = ORIENTED_EDGE ( 'NONE', *, *, #33822, .T. ) ;
#67517 = CARTESIAN_POINT ( 'NONE',  ( 15.89062500061451289, -3.027376345333614438, 5.243569643749998122 ) ) ;
#67518 = CARTESIAN_POINT ( 'NONE',  ( 9.440625000614517148, 6.054752690667223547, 3.707466751127219781E-16 ) ) ;
#67519 = CARTESIAN_POINT ( 'NONE',  ( 18.87187500061451573, 4.119189519843966529, 2.378215178124999607 ) ) ;
#67520 = CARTESIAN_POINT ( 'NONE',  ( 3.534375000614518036, 6.421520780324663323E-16, -5.243569643749999010 ) ) ;
#67521 = CARTESIAN_POINT ( 'NONE',  ( 18.41250000122903430, 0.000000000000000000, 4.999999999999998224 ) ) ;
#67522 = CARTESIAN_POINT ( 'NONE',  ( 23.66250000000000142, 2.886751345948126879, 4.999999999999999112 ) ) ;
#67523 = DIRECTION ( 'NONE',  ( -0.000000000000000000, -1.000000000000000000, -0.000000000000000000 ) ) ;
#67524 = CARTESIAN_POINT ( 'NONE',  ( 6.871875000614517504, 3.027376345333611329, 5.243569643749999010 ) ) ;
#67525 = CARTESIAN_POINT ( 'NONE',  ( 11.74687500061451573, 6.054752690667223547, 3.707466751127219781E-16 ) ) ;
#67526 = CARTESIAN_POINT ( 'NONE',  ( 21.87187500061451573, -6.054752690667223547, -1.112240025338166033E-15 ) ) ;
#67527 = EDGE_CURVE ( 'NONE', #675, #38481, #22666, .T. ) ;
#67528 = PLANE ( 'NONE',  #21857 ) ;
#67529 = ORIENTED_EDGE ( 'NONE', *, *, #68939, .T. ) ;
#67530 = CARTESIAN_POINT ( 'NONE',  ( 4.284375000614518925, -4.541064518000419881, 2.621784821874995952 ) ) ;
#67531 = CARTESIAN_POINT ( 'NONE',  ( 6.909375000614518036, 0.000000000000000000, 5.243569643749999010 ) ) ;
#67532 = CARTESIAN_POINT ( 'NONE',  ( 17.69999999999999929, 4.330127018922192761, -2.499999999999997780 ) ) ;
#67533 = CARTESIAN_POINT ( 'NONE',  ( 16.94062500061451715, -3.027376345333610441, -5.243569643749999898 ) ) ;
#67534 = CARTESIAN_POINT ( 'NONE',  ( 4.000000000000000000, 17.93750000000000355, 27.69059892324149530 ) ) ;
#67535 = DIRECTION ( 'NONE',  ( 0.000000000000000000, 0.000000000000000000, 1.000000000000000000 ) ) ;
#67536 = CARTESIAN_POINT ( 'NONE',  ( 22.65937500061451715, 0.000000000000000000, 4.756430356249998326 ) ) ;
#67537 = CARTESIAN_POINT ( 'NONE',  ( 11.09062500061451573, -3.027376345333610441, -5.243569643749999898 ) ) ;
#67538 = CARTESIAN_POINT ( 'NONE',  ( 25.88437500061451502, -4.541064518000419881, 2.621784821874995952 ) ) ;
#67539 = PLANE ( 'NONE',  #23040 ) ;
#67540 = CARTESIAN_POINT ( 'NONE',  ( 29.33437500061451431, 4.541064518000418104, 2.621784821874999949 ) ) ;
#67541 = CARTESIAN_POINT ( 'NONE',  ( 10.65000000000000036, 0.000000000000000000, 4.999999999999998224 ) ) ;
#67542 = CARTESIAN_POINT ( 'NONE',  ( -1.999999999999997113, 15.23750000122903536, 33.46410161513775705 ) ) ;
#67543 = CARTESIAN_POINT ( 'NONE',  ( 10.16250000122903252, 4.330127018922192761, -2.499999999999997780 ) ) ;
#67544 = CARTESIAN_POINT ( 'NONE',  ( 20.82187500061451857, 3.027376345333611329, 5.243569643749999010 ) ) ;
#67545 = CARTESIAN_POINT ( 'NONE',  ( 14.40937500061451715, 4.541064518000418104, -2.621784821874998173 ) ) ;
#67546 = DIRECTION ( 'NONE',  ( -1.000000000000000000, -0.000000000000000000, -0.000000000000000000 ) ) ;
#67547 = ORIENTED_EDGE ( 'NONE', *, *, #1251, .F. ) ;
#67548 = CARTESIAN_POINT ( 'NONE',  ( 14.57812500061451644, -4.541064518000419881, 2.621784821874995952 ) ) ;
#67549 = CARTESIAN_POINT ( 'NONE',  ( 26.55000000122902648, -2.886751345948129988, 4.999999999999997335 ) ) ;
#67550 = CARTESIAN_POINT ( 'NONE',  ( 16.20937500061451786, 4.541064518000418104, -2.621784821874998173 ) ) ;
#67551 = CARTESIAN_POINT ( 'NONE',  ( 5.378878668797003826, 8.432125716319053055, -32.68706799072294444 ) ) ;
#67552 = CARTESIAN_POINT ( 'NONE',  ( 15.96562500061451573, -6.054752690667223547, -1.112240025338166033E-15 ) ) ;
#67553 = CARTESIAN_POINT ( 'NONE',  ( 18.33749999999999858, -2.886751345948130876, 4.999999999999996447 ) ) ;
#67554 = CARTESIAN_POINT ( 'NONE',  ( 25.77187500061451075, 3.027376345333611329, 5.243569643749999010 ) ) ;
#67555 = CARTESIAN_POINT ( 'NONE',  ( 4.243569643749999898, 11.44062500061451715, 32.45002607614398471 ) ) ;
#67556 = CARTESIAN_POINT ( 'NONE',  ( 16.13437500061451502, 6.421520780324663323E-16, -5.243569643749999010 ) ) ;
#67557 = CARTESIAN_POINT ( 'NONE',  ( 13.91250000122903252, 0.000000000000000000, 4.999999999999998224 ) ) ;
#67558 = DIRECTION ( 'NONE',  ( 0.000000000000000000, 0.000000000000000000, 1.000000000000000000 ) ) ;
#67559 = FACE_OUTER_BOUND ( 'NONE', #2475, .T. ) ;
#67560 = CARTESIAN_POINT ( 'NONE',  ( 18.23437500061451999, -4.541064518000419881, 2.621784821874995952 ) ) ;
#67561 = CARTESIAN_POINT ( 'NONE',  ( 20.58750000122903145, 4.330127018922191873, 2.499999999999999556 ) ) ;
#67562 = CARTESIAN_POINT ( 'NONE',  ( 13.69687500061451679, -3.027376345333614438, 5.243569643749998122 ) ) ;
#67563 = CARTESIAN_POINT ( 'NONE',  ( -2.121784821874999949, 12.13437500061451857, 26.32496088578401938 ) ) ;
#67564 = CARTESIAN_POINT ( 'NONE',  ( 22.72500000122903430, 2.886751345948129099, -4.999999999999998224 ) ) ;
#67565 = CARTESIAN_POINT ( 'NONE',  ( 17.95312500061451644, 4.541064518000418104, -2.621784821874998173 ) ) ;
#67566 = ORIENTED_EDGE ( 'NONE', *, *, #66718, .F. ) ;
#67567 = ORIENTED_EDGE ( 'NONE', *, *, #2964, .T. ) ;
#67568 = CARTESIAN_POINT ( 'NONE',  ( 21.41250000000000497, 2.886751345948126879, 4.999999999999999112 ) ) ;
#67569 = CARTESIAN_POINT ( 'NONE',  ( 45.00000000000000000, -3.142333204958820020E-14, -9.000000000000000000 ) ) ;
#67570 = CARTESIAN_POINT ( 'NONE',  ( 22.64062500061451644, -3.027376345333614438, 5.243569643749998122 ) ) ;
#67571 = CARTESIAN_POINT ( 'NONE',  ( 3.992467690304758232, 3.010110221998377078, 29.71877081132206655 ) ) ;
#67572 = CARTESIAN_POINT ( 'NONE',  ( 14.17500000122903536, 2.886751345948129099, -4.999999999999998224 ) ) ;
#67573 = CARTESIAN_POINT ( 'NONE',  ( 21.40312500061451573, -4.541064518000417216, -2.621784821875001281 ) ) ;
#67574 = CARTESIAN_POINT ( 'NONE',  ( 24.40312500061451573, 0.000000000000000000, 5.243569643749999010 ) ) ;
#67575 = CARTESIAN_POINT ( 'NONE',  ( 5.428125000614517859, 4.541064518000418104, 2.621784821874999949 ) ) ;
#67576 = ORIENTED_EDGE ( 'NONE', *, *, #48137, .F. ) ;
#67577 = VECTOR ( 'NONE', #55265, 1000.000000000000000 ) ;
#67578 = DIRECTION ( 'NONE',  ( -0.000000000000000000, -1.000000000000000000, -0.000000000000000000 ) ) ;
#67579 = CARTESIAN_POINT ( 'NONE',  ( 17.32499999999999929, 4.330127018922191873, 2.499999999999999556 ) ) ;
#67580 = CARTESIAN_POINT ( 'NONE',  ( 10.99687500061451750, -2.746126346562646425, 4.756430356249996549 ) ) ;
#67581 = CARTESIAN_POINT ( 'NONE',  ( 45.00000000000000000, 0.000000000000000000, 0.000000000000000000 ) ) ;
#67582 = CARTESIAN_POINT ( 'NONE',  ( -3.999999999999999112, 11.11250000122903536, -30.00000000000000000 ) ) ;
#67583 = CARTESIAN_POINT ( 'NONE',  ( -4.243569643749999898, 18.02187500061452141, -32.45002607614398471 ) ) ;
#67584 = CARTESIAN_POINT ( 'NONE',  ( 5.625000001229036428, 2.886751345948129099, -4.999999999999998224 ) ) ;
#67585 = CARTESIAN_POINT ( 'NONE',  ( 7.275000000000000355, 6.123233995736764310E-16, -4.999999999999998224 ) ) ;
#67586 = EDGE_CURVE ( 'NONE', #59214, #3561, #26810, .T. ) ;
#67587 = CARTESIAN_POINT ( 'NONE',  ( 4.087500001229035007, -4.330127018922194537, 2.499999999999995559 ) ) ;
#67588 = CARTESIAN_POINT ( 'NONE',  ( 12.79687500061451821, -3.027376345333614438, 5.243569643749998122 ) ) ;
#67589 = CARTESIAN_POINT ( 'NONE',  ( 3.999999999999999112, 16.73750000122903359, -30.00000000000000000 ) ) ;
#67590 = CARTESIAN_POINT ( 'NONE',  ( 2.971875000614517592, -6.054752690667223547, -1.112240025338166033E-15 ) ) ;
#67591 = CARTESIAN_POINT ( 'NONE',  ( 12.93750000122903465, 4.330127018922191873, 2.499999999999999556 ) ) ;
#67592 = CARTESIAN_POINT ( 'NONE',  ( 12.69375000122903430, -2.886751345948126435, -5.000000000000000000 ) ) ;
#67593 = CARTESIAN_POINT ( 'NONE',  ( 10.62187500061451928, -6.054752690667223547, -1.112240025338166033E-15 ) ) ;
#67594 = CARTESIAN_POINT ( 'NONE',  ( 1.071796769724495668, 17.09509619066136921, -26.00000000000000711 ) ) ;
#67595 = CARTESIAN_POINT ( 'NONE',  ( 4.494741915665276366, -2.190272839526016924, 4.494741915664858922 ) ) ;
#67596 = CARTESIAN_POINT ( 'NONE',  ( -2.121784821874999949, 17.02812500061459744, 26.32496088578401938 ) ) ;
#67597 = CARTESIAN_POINT ( 'NONE',  ( 20.67187500061451289, 3.027376345333613106, -5.243569643749998122 ) ) ;
#67598 = SURFACE_STYLE_USAGE ( .BOTH. , #34683 ) ;
#67599 = CARTESIAN_POINT ( 'NONE',  ( 2.953125000614516438, -4.541064518000417216, -2.621784821875001281 ) ) ;
#67600 = CARTESIAN_POINT ( 'NONE',  ( 17.37187500061451573, 5.824947211148865298E-16, -4.756430356249998326 ) ) ;
#67601 = CARTESIAN_POINT ( 'NONE',  ( 25.15312500061451217, 4.541064518000418104, -2.621784821874998173 ) ) ;
#67602 = CARTESIAN_POINT ( 'NONE',  ( 14.39062500061451821, 6.054752690667223547, 3.707466751127219781E-16 ) ) ;
#67603 = CARTESIAN_POINT ( 'NONE',  ( 15.09375000122903110, 5.773502691896255534, 3.535250795749688894E-16 ) ) ;
#67604 = CARTESIAN_POINT ( 'NONE',  ( 11.70937500061451608, 4.541064518000418104, -2.621784821874998173 ) ) ;
#67605 = CARTESIAN_POINT ( 'NONE',  ( 29.51249999999999929, 2.886751345948126879, 4.999999999999999112 ) ) ;
#67606 = CARTESIAN_POINT ( 'NONE',  ( 25.80000000122903714, -2.886751345948125991, -5.000000000000000000 ) ) ;
#67607 = CARTESIAN_POINT ( 'NONE',  ( 3.159375000614518036, 4.541064518000418104, -2.621784821874998173 ) ) ;
#67608 = CARTESIAN_POINT ( 'NONE',  ( 15.27187500061451786, 3.027376345333613106, -5.243569643749998122 ) ) ;
#67609 = CARTESIAN_POINT ( 'NONE',  ( 21.11250000000000071, -5.773502691896255534, -1.060575238724906372E-15 ) ) ;
#67610 = CARTESIAN_POINT ( 'NONE',  ( 30.00000000000000000, 6.123233995736764310E-16, -4.999999999999998224 ) ) ;
#67611 = CARTESIAN_POINT ( 'NONE',  ( 21.83437500061451786, -4.541064518000419881, 2.621784821874995952 ) ) ;
#67612 = CARTESIAN_POINT ( 'NONE',  ( 13.73437500061451821, -4.541064518000419881, 2.621784821874995952 ) ) ;
#67613 = CARTESIAN_POINT ( 'NONE',  ( 2.655984681222220721E-16, 16.91562499938548214, 25.66244784525396483 ) ) ;
#67614 = CARTESIAN_POINT ( 'NONE',  ( 27.82499999999999929, -4.330127018922194537, 2.499999999999995559 ) ) ;
#67615 = CARTESIAN_POINT ( 'NONE',  ( 0.000000000000000000, 20.00000000000000000, 30.00000000000000000 ) ) ;
#67616 = CARTESIAN_POINT ( 'NONE',  ( 29.52187500061451431, -5.492252693125287522, -1.008910452111647106E-15 ) ) ;
#67617 = CARTESIAN_POINT ( 'NONE',  ( 17.31562500061451715, -6.054752690667223547, -1.112240025338166033E-15 ) ) ;
#67618 = CARTESIAN_POINT ( 'NONE',  ( 7.650000000000000355, -4.330127018922190985, -2.500000000000001332 ) ) ;
#67619 = CARTESIAN_POINT ( 'NONE',  ( 15.37500000000000000, 6.123233995736764310E-16, -4.999999999999998224 ) ) ;
#67620 = CARTESIAN_POINT ( 'NONE',  ( 15.97499999999999964, 4.330127018922191873, 2.499999999999999556 ) ) ;
#67621 = CARTESIAN_POINT ( 'NONE',  ( 2.121784821874999061, 13.35312500061451679, 26.32496088578401583 ) ) ;
#67622 = CARTESIAN_POINT ( 'NONE',  ( -1.071796769724492115, 16.41740381056766651, 34.00000000000000000 ) ) ;
#67623 = CARTESIAN_POINT ( 'NONE',  ( 20.85000000122903430, -2.886751345948125991, -5.000000000000000000 ) ) ;
#67624 = CARTESIAN_POINT ( 'NONE',  ( 11.30625000122903501, -4.330127018922190985, -2.500000000000001332 ) ) ;
#67625 = CARTESIAN_POINT ( 'NONE',  ( 28.20937500061451786, -4.541064518000417216, -2.621784821875001281 ) ) ;
#67626 = ORIENTED_EDGE ( 'NONE', *, *, #51739, .F. ) ;
#67627 = CARTESIAN_POINT ( 'NONE',  ( 22.45312500061451644, 4.541064518000418104, -2.621784821874998173 ) ) ;
#67628 = CARTESIAN_POINT ( 'NONE',  ( 22.39687500061451075, -3.027376345333610441, -5.243569643749999898 ) ) ;
#67629 = CARTESIAN_POINT ( 'NONE',  ( 7.537500000000002309, -2.886751345948129988, 4.999999999999997335 ) ) ;
#67630 = CARTESIAN_POINT ( 'NONE',  ( 10.00312500061451715, 0.000000000000000000, 5.243569643749999010 ) ) ;
#67631 = CARTESIAN_POINT ( 'NONE',  ( 24.32812500061451289, 4.541064518000418104, 2.621784821874999949 ) ) ;
#67632 = CARTESIAN_POINT ( 'NONE',  ( 15.53437500061451715, -4.541064518000419881, 2.621784821874995952 ) ) ;
#67633 = CARTESIAN_POINT ( 'NONE',  ( 16.95937500061451786, -4.541064518000417216, -2.621784821875001281 ) ) ;
#67634 = CARTESIAN_POINT ( 'NONE',  ( 19.31250000000000000, -5.773502691896255534, -1.060575238724906372E-15 ) ) ;
#67635 = CARTESIAN_POINT ( 'NONE',  ( 4.243569643749999898, 18.67812500061451431, 30.00000000000000000 ) ) ;
#67636 = EDGE_CURVE ( 'NONE', #71649, #12198, #23746, .T. ) ;
#67637 = CARTESIAN_POINT ( 'NONE',  ( 21.30000000122903359, -2.886751345948125991, -5.000000000000000000 ) ) ;
#67638 = CARTESIAN_POINT ( 'NONE',  ( 13.80937500061451750, -4.119189519843965641, -2.378215178125001383 ) ) ;
#67639 = CARTESIAN_POINT ( 'NONE',  ( 12.21562500061451573, 3.027376345333611329, 5.243569643749999010 ) ) ;
#67640 = CARTESIAN_POINT ( 'NONE',  ( 6.384375000614516793, 4.541064518000418104, 2.621784821874999949 ) ) ;
#67641 = CARTESIAN_POINT ( 'NONE',  ( 3.834375000614519635, -4.541064518000419881, 2.621784821874995952 ) ) ;
#67642 = ORIENTED_EDGE ( 'NONE', *, *, #67328, .F. ) ;
#67643 = CARTESIAN_POINT ( 'NONE',  ( 27.23437500061451644, -4.541064518000419881, 2.621784821874995952 ) ) ;
#67644 = CARTESIAN_POINT ( 'NONE',  ( 16.67812500061451786, 4.541064518000418104, 2.621784821874999949 ) ) ;
#67645 = CARTESIAN_POINT ( 'NONE',  ( 27.07500000122903216, -5.773502691896255534, -1.060575238724906372E-15 ) ) ;
#67646 = CARTESIAN_POINT ( 'NONE',  ( 26.61562500061451786, 3.027376345333611329, 5.243569643749999010 ) ) ;
#67647 = CARTESIAN_POINT ( 'NONE',  ( 21.94687500061451857, -3.027376345333610441, -5.243569643749999898 ) ) ;
#67648 = CARTESIAN_POINT ( 'NONE',  ( 17.65312500061451573, 0.000000000000000000, 5.243569643749999010 ) ) ;
#67649 = CARTESIAN_POINT ( 'NONE',  ( 8.484601909799253346E-16, 10.66250000000000142, 34.61880215351700230 ) ) ;
#67650 = CARTESIAN_POINT ( 'NONE',  ( 25.00312500061451715, -4.541064518000417216, -2.621784821875001281 ) ) ;
#67651 = CARTESIAN_POINT ( 'NONE',  ( 5.475000001229035185, -5.773502691896255534, -1.060575238724906372E-15 ) ) ;
#67652 = ORIENTED_EDGE ( 'NONE', *, *, #13859, .T. ) ;
#67653 = CARTESIAN_POINT ( 'NONE',  ( 28.08749999999999858, 5.773502691896255534, 3.535250795749688894E-16 ) ) ;
#67654 = CARTESIAN_POINT ( 'NONE',  ( 8.484601909799253346E-16, 12.01250000000000107, -25.38119784648299770 ) ) ;
#67655 = CARTESIAN_POINT ( 'NONE',  ( 3.756430356250000102, 16.80312499938548498, 30.00000000000000000 ) ) ;
#67656 = CARTESIAN_POINT ( 'NONE',  ( 4.209375000614516971, 0.000000000000000000, 5.243569643749999010 ) ) ;
#67657 = CARTESIAN_POINT ( 'NONE',  ( 9.590625000614517504, -3.027376345333614438, 5.243569643749998122 ) ) ;
#67658 = CARTESIAN_POINT ( 'NONE',  ( 6.234375000614519102, 6.421520780324663323E-16, -5.243569643749999010 ) ) ;
#67659 = CARTESIAN_POINT ( 'NONE',  ( 24.11250000122903359, 4.330127018922192761, -2.499999999999997780 ) ) ;
#67660 = CARTESIAN_POINT ( 'NONE',  ( 12.12187500061451573, 3.027376345333612662, -5.243569643749998122 ) ) ;
#67661 = CARTESIAN_POINT ( 'NONE',  ( 28.64062500061451289, -3.027376345333610441, -5.243569643749999898 ) ) ;
#67662 = CARTESIAN_POINT ( 'NONE',  ( 26.92499999999999716, -4.330127018922194537, 2.499999999999995559 ) ) ;
#67663 = DIRECTION ( 'NONE',  ( -1.000000000000000000, -0.000000000000000000, -0.000000000000000000 ) ) ;
#67664 = CARTESIAN_POINT ( 'NONE',  ( 13.94062500061451892, 6.054752690667223547, 3.707466751127219781E-16 ) ) ;
#67665 =( BOUNDED_CURVE ( )  B_SPLINE_CURVE ( 2, ( #52147, #56951, #62500, #17429, #30342, #828, #63587 ),
 .UNSPECIFIED., .F., .F. ) 
 B_SPLINE_CURVE_WITH_KNOTS ( ( 3, 2, 2, 3 ),
 ( 0.9770271732711595103, 0.9777777777777777457, 0.9805555555555555136, 0.9812341018960827332 ),
 .UNSPECIFIED. ) 
 CURVE ( )  GEOMETRIC_REPRESENTATION_ITEM ( )  RATIONAL_B_SPLINE_CURVE ( ( 0.9471604034606007083, 0.9637977031509668002, 1.000000000000000000, 0.8660254037844387076, 1.000000000000000000, 0.9672731300851546976, 0.9505350825990019903 ) ) 
 REPRESENTATION_ITEM ( '' )  );
#67666 = EDGE_LOOP ( 'NONE', ( #17773, #28121, #58726, #63946 ) ) ;
#67667 = CARTESIAN_POINT ( 'NONE',  ( 10.79062500061451679, 6.054752690667223547, 3.707466751127219781E-16 ) ) ;
#67668 = CARTESIAN_POINT ( 'NONE',  ( 6.065625000614516260, -6.054752690667223547, -1.112240025338166033E-15 ) ) ;
#67669 = CARTESIAN_POINT ( 'NONE',  ( 18.83437500061451431, 5.824947211148865298E-16, -4.756430356249998326 ) ) ;
#67670 = CARTESIAN_POINT ( 'NONE',  ( 25.38750000122903216, 6.123233995736764310E-16, -4.999999999999998224 ) ) ;
#67671 = CARTESIAN_POINT ( 'NONE',  ( 16.12500000000000000, -4.330127018922194537, 2.499999999999995559 ) ) ;
#67672 = CARTESIAN_POINT ( 'NONE',  ( 16.84687500061451715, -3.027376345333614438, 5.243569643749998122 ) ) ;
#67673 = CARTESIAN_POINT ( 'NONE',  ( 11.88750000122903216, 6.123233995736764310E-16, -4.999999999999998224 ) ) ;
#67674 = CARTESIAN_POINT ( 'NONE',  ( 20.28750000000000142, -2.886751345948125991, -5.000000000000000000 ) ) ;
#67675 = CARTESIAN_POINT ( 'NONE',  ( 20.14687500061451786, -3.027376345333610441, -5.243569643749999898 ) ) ;
#67676 = CARTESIAN_POINT ( 'NONE',  ( 4.243569643749999898, 15.04062500061451679, -27.54997392385601529 ) ) ;
#67677 = LINE ( 'NONE', #40319, #35927 ) ;
#67678 = CARTESIAN_POINT ( 'NONE',  ( 26.70937500061451075, -5.492252693125287522, -1.008910452111647106E-15 ) ) ;
#67679 = CARTESIAN_POINT ( 'NONE',  ( 2.000000000000001332, 11.60000000000000142, -26.53589838486224650 ) ) ;
#67680 = CARTESIAN_POINT ( 'NONE',  ( 26.80312500061451431, -4.541064518000417216, -2.621784821875001281 ) ) ;
#67681 = LINE ( 'NONE', #22243, #44429 ) ;
#67682 = EDGE_CURVE ( 'NONE', #43575, #20886, #63276, .T. ) ;
#67683 = CARTESIAN_POINT ( 'NONE',  ( 24.89999999999999858, 4.330127018922192761, -2.499999999999997780 ) ) ;
#67684 = CARTESIAN_POINT ( 'NONE',  ( 10.15312500061451750, -4.541064518000417216, -2.621784821875001281 ) ) ;
#67685 = CARTESIAN_POINT ( 'NONE',  ( 28.32187500061451502, 4.119189519843966529, 2.378215178124999607 ) ) ;
#67686 = CARTESIAN_POINT ( 'NONE',  ( 18.04687500061451999, 6.054752690667223547, 3.707466751127219781E-16 ) ) ;
#67687 = CARTESIAN_POINT ( 'NONE',  ( 11.25937500061451679, 2.746126346562643317, 4.756430356249998326 ) ) ;
#67688 = CARTESIAN_POINT ( 'NONE',  ( 5.840625000614516615, 6.054752690667223547, 3.707466751127219781E-16 ) ) ;
#67689 = CARTESIAN_POINT ( 'NONE',  ( 9.796875000614519990, -3.027376345333610441, -5.243569643749999898 ) ) ;
#67690 = ORIENTED_EDGE ( 'NONE', *, *, #63077, .F. ) ;
#67691 = CARTESIAN_POINT ( 'NONE',  ( 20.55937500061451573, -4.541064518000417216, -2.621784821875001281 ) ) ;
#67692 = CARTESIAN_POINT ( 'NONE',  ( 28.31250000000000000, -5.773502691896255534, -1.060575238724906372E-15 ) ) ;
#67693 = CARTESIAN_POINT ( 'NONE',  ( 5.962500000000002132, 2.886751345948129099, -4.999999999999998224 ) ) ;
#67694 = CARTESIAN_POINT ( 'NONE',  ( 14.28750000122903430, 4.330127018922191873, 2.499999999999999556 ) ) ;
#67695 = CARTESIAN_POINT ( 'NONE',  ( 3.999999999999999112, 12.23750000122903359, 30.00000000000000000 ) ) ;
#67696 = CARTESIAN_POINT ( 'NONE',  ( -1.071796769724490783, 19.19240381056767220, -26.00000000000000355 ) ) ;
#67697 = ORIENTED_EDGE ( 'NONE', *, *, #32153, .T. ) ;
#67698 = CARTESIAN_POINT ( 'NONE',  ( 13.50000000000000178, -4.330127018922190985, -2.500000000000001332 ) ) ;
#67699 = CARTESIAN_POINT ( 'NONE',  ( 24.06562500061451715, -6.054752690667223547, -1.112240025338166033E-15 ) ) ;
#67700 = CARTESIAN_POINT ( 'NONE',  ( 16.12500000000000000, -4.330127018922194537, 2.499999999999995559 ) ) ;
#67701 = CARTESIAN_POINT ( 'NONE',  ( 10.08750000122903323, 6.123233995736764310E-16, -4.999999999999998224 ) ) ;
#67702 = CARTESIAN_POINT ( 'NONE',  ( 9.515625000614518214, 3.027376345333611329, 5.243569643749999010 ) ) ;
#67703 = CARTESIAN_POINT ( 'NONE',  ( 9.074999999999999289, 6.123233995736764310E-16, -4.999999999999998224 ) ) ;
#67704 = CARTESIAN_POINT ( 'NONE',  ( 18.86250000122903359, 0.000000000000000000, 4.999999999999998224 ) ) ;
#67705 = CARTESIAN_POINT ( 'NONE',  ( -4.243569643749997233, 14.49687500061451928, -27.54997392385601174 ) ) ;
#67706 = CARTESIAN_POINT ( 'NONE',  ( 26.96250000122903145, 0.000000000000000000, 4.999999999999998224 ) ) ;
#67707 = CARTESIAN_POINT ( 'NONE',  ( 3.756430356250000546, 14.02812499938548285, 27.83122392262697886 ) ) ;
#67708 = CARTESIAN_POINT ( 'NONE',  ( 7.950000000000001954, 0.000000000000000000, 4.999999999999998224 ) ) ;
#67709 = CARTESIAN_POINT ( 'NONE',  ( 4.898587196589411843E-16, 20.00000000000000000, 33.99999999999999289 ) ) ;
#67710 = ORIENTED_EDGE ( 'NONE', *, *, #16678, .T. ) ;
#67711 = CARTESIAN_POINT ( 'NONE',  ( 23.54062500061451146, -3.027376345333614438, 5.243569643749998122 ) ) ;
#67712 = CARTESIAN_POINT ( 'NONE',  ( 13.16250000122903430, -4.330127018922190985, -2.500000000000001332 ) ) ;
#67713 = CARTESIAN_POINT ( 'NONE',  ( 29.31562500061451715, 3.027376345333611329, 5.243569643749999010 ) ) ;
#67714 = CARTESIAN_POINT ( 'NONE',  ( 29.37187500061451928, 3.027376345333611329, 5.243569643749999010 ) ) ;
#67715 = CARTESIAN_POINT ( 'NONE',  ( 18.64687500061451786, -3.027376345333614438, 5.243569643749998122 ) ) ;
#67716 = CARTESIAN_POINT ( 'NONE',  ( 16.82812500061451644, -4.541064518000419881, 2.621784821874995952 ) ) ;
#67717 = CARTESIAN_POINT ( 'NONE',  ( -4.243569643749998122, 12.19062500061459353, -27.54997392385601174 ) ) ;
#67718 = CARTESIAN_POINT ( 'NONE',  ( 5.915625000614515905, 3.027376345333611329, 5.243569643749999010 ) ) ;
#67719 = CARTESIAN_POINT ( 'NONE',  ( 28.35000000122903430, -2.886751345948129988, 4.999999999999997335 ) ) ;
#67720 = CARTESIAN_POINT ( 'NONE',  ( 21.75937500061451502, 0.000000000000000000, 4.756430356249998326 ) ) ;
#67721 = CARTESIAN_POINT ( 'NONE',  ( 19.52812500061451573, -4.541064518000419881, 2.621784821874995952 ) ) ;
#67722 = CARTESIAN_POINT ( 'NONE',  ( 24.88125000122903074, 6.123233995736764310E-16, -4.999999999999998224 ) ) ;
#67723 = CARTESIAN_POINT ( 'NONE',  ( -3.756430356249999214, 19.12812499938548427, 27.83122392262697531 ) ) ;
#67724 = CARTESIAN_POINT ( 'NONE',  ( 13.95937500061451786, 4.541064518000418104, -2.621784821874998173 ) ) ;
#67725 = CARTESIAN_POINT ( 'NONE',  ( 10.84687500061451892, 6.054752690667223547, 3.707466751127219781E-16 ) ) ;
#67726 = CARTESIAN_POINT ( 'NONE',  ( 20.33437500061451786, 4.541064518000418104, 2.621784821874999949 ) ) ;
#67727 = ORIENTED_EDGE ( 'NONE', *, *, #57642, .T. ) ;
#67728 = CARTESIAN_POINT ( 'NONE',  ( 27.25312500061451360, -4.541064518000417216, -2.621784821875001281 ) ) ;
#67729 = CARTESIAN_POINT ( 'NONE',  ( 25.11562500061451431, 3.027376345333613106, -5.243569643749998122 ) ) ;
#67730 = CARTESIAN_POINT ( 'NONE',  ( 17.23125000122903572, 6.123233995736764310E-16, -4.999999999999998224 ) ) ;
#67731 = CARTESIAN_POINT ( 'NONE',  ( 2.000000000000001332, 17.00000000000000000, 33.46410161513774995 ) ) ;
#67732 = AXIS2_PLACEMENT_3D ( 'NONE', #62659, #10609, #67498 ) ;
#67733 = CARTESIAN_POINT ( 'NONE',  ( 4.396875000614516971, -3.027376345333610441, -5.243569643749999898 ) ) ;
#67734 = ITEM_DEFINED_TRANSFORMATION ( 'NONE', 'NONE', #69825,  #23765 ) ;
#67735 = CARTESIAN_POINT ( 'NONE',  ( 11.77500000122903501, -5.773502691896255534, -1.060575238724906372E-15 ) ) ;
#67736 = CARTESIAN_POINT ( 'NONE',  ( 8.137500001229033941, -4.330127018922194537, 2.499999999999995559 ) ) ;
#67737 = CARTESIAN_POINT ( 'NONE',  ( 21.67500000122902648, -5.773502691896255534, -1.060575238724906372E-15 ) ) ;
#67738 = CARTESIAN_POINT ( 'NONE',  ( 28.65000000122903145, 5.773502691896255534, 3.535250795749688894E-16 ) ) ;
#67739 = CARTESIAN_POINT ( 'NONE',  ( -4.000000000000000000, 17.61874999877096570, 30.00000000000000000 ) ) ;
#67740 = CARTESIAN_POINT ( 'NONE',  ( 15.65625000122903465, 0.000000000000000000, 4.999999999999998224 ) ) ;
#67741 = CARTESIAN_POINT ( 'NONE',  ( 10.99687500061451750, -3.027376345333614438, 5.243569643749998122 ) ) ;
#67742 = CARTESIAN_POINT ( 'NONE',  ( -4.000000000000000000, 17.61874999877096570, 30.00000000000000000 ) ) ;
#67743 = EDGE_CURVE ( 'NONE', #60188, #29691, #18918, .T. ) ;
#67744 = CARTESIAN_POINT ( 'NONE',  ( 16.52812500061451573, 6.421520780324663323E-16, -5.243569643749999010 ) ) ;
#67745 = CARTESIAN_POINT ( 'NONE',  ( 13.32187500061451502, -6.054752690667223547, -1.112240025338166033E-15 ) ) ;
#67746 = CARTESIAN_POINT ( 'NONE',  ( 4.715625000614516615, -6.054752690667223547, -1.112240025338166033E-15 ) ) ;
#67747 = CARTESIAN_POINT ( 'NONE',  ( 22.09687500061451715, 6.054752690667223547, 3.707466751127219781E-16 ) ) ;
#67748 = CARTESIAN_POINT ( 'NONE',  ( 10.50937500061451679, 0.000000000000000000, 5.243569643749999010 ) ) ;
#67749 = CARTESIAN_POINT ( 'NONE',  ( 4.040625000614517681, 6.054752690667223547, 3.707466751127219781E-16 ) ) ;
#67750 = CARTESIAN_POINT ( 'NONE',  ( 10.76250000000000107, -5.773502691896255534, -1.060575238724906372E-15 ) ) ;
#67751 = CARTESIAN_POINT ( 'NONE',  ( 5.887500001229034829, -4.330127018922194537, 2.499999999999995559 ) ) ;
#67752 = CARTESIAN_POINT ( 'NONE',  ( 20.42812500061451431, -4.541064518000419881, 2.621784821874995952 ) ) ;
#67753 = CARTESIAN_POINT ( 'NONE',  ( 7.350000001229033408, -2.886751345948125991, -5.000000000000000000 ) ) ;
#67754 = CARTESIAN_POINT ( 'NONE',  ( 18.44062500061451715, 6.054752690667223547, 3.707466751127219781E-16 ) ) ;
#67755 = CARTESIAN_POINT ( 'NONE',  ( 12.77812500061451750, -4.541064518000419881, 2.621784821874995952 ) ) ;
#67756 = CARTESIAN_POINT ( 'NONE',  ( 26.85937500061451644, -4.119189519843965641, -2.378215178125001383 ) ) ;
#67757 = CARTESIAN_POINT ( 'NONE',  ( 14.24999999999999822, 0.000000000000000000, 4.999999999999998224 ) ) ;
#67758 = CARTESIAN_POINT ( 'NONE',  ( 9.562500001229032875, -4.330127018922190985, -2.500000000000001332 ) ) ;
#67759 = CARTESIAN_POINT ( 'NONE',  ( 6.590625000614518392, -3.027376345333610441, -5.243569643749999898 ) ) ;
#67760 = CARTESIAN_POINT ( 'NONE',  ( 21.93750000122903288, 4.330127018922191873, 2.499999999999999556 ) ) ;
#67761 = CARTESIAN_POINT ( 'NONE',  ( 27.03750000000000142, -2.886751345948125991, -5.000000000000000000 ) ) ;
#67762 = CARTESIAN_POINT ( 'NONE',  ( -4.243569643749999898, 10.85937500061451821, -30.00000000000000000 ) ) ;
#67763 = CARTESIAN_POINT ( 'NONE',  ( 1.626862140677534273E-15, 17.86250000000000071, 34.00000000000000000 ) ) ;
#67764 = FACE_OUTER_BOUND ( 'NONE', #640, .T. ) ;
#67765 = CARTESIAN_POINT ( 'NONE',  ( -3.999999999999999112, 11.45000000000000107, -30.00000000000000000 ) ) ;
#67766 = CARTESIAN_POINT ( 'NONE',  ( 21.64687500061451786, 6.054752690667223547, 3.707466751127219781E-16 ) ) ;
#67767 = ADVANCED_FACE ( 'NONE', ( #8221 ), #64730, .T. ) ;
#67768 = CARTESIAN_POINT ( 'NONE',  ( 2.000000000000001332, 18.46250000122903501, 33.46410161513774995 ) ) ;
#67769 = CARTESIAN_POINT ( 'NONE',  ( 16.86562500061451786, -6.054752690667223547, -1.112240025338166033E-15 ) ) ;
#67770 = CARTESIAN_POINT ( 'NONE',  ( 10.63125000122903252, 4.330127018922191873, 2.499999999999999556 ) ) ;
#67771 = CARTESIAN_POINT ( 'NONE',  ( -2.000000000000001776, 20.84374999877096357, 33.46410161513775705 ) ) ;
#67772 = CARTESIAN_POINT ( 'NONE',  ( 4.385796401931335353, -2.400997692794667682, 4.385796401931427724 ) ) ;
#67773 = CARTESIAN_POINT ( 'NONE',  ( 26.52187500061451431, 3.027376345333613106, -5.243569643749998122 ) ) ;
#67774 = CARTESIAN_POINT ( 'NONE',  ( 21.90937500061451715, 2.746126346562645981, -4.756430356249997438 ) ) ;
#67775 = AXIS2_PLACEMENT_3D ( 'NONE', #58826, #31869, #8973 ) ;
#67776 = CARTESIAN_POINT ( 'NONE',  ( 12.55312500061451786, 4.541064518000418104, -2.621784821874998173 ) ) ;
#67777 = CARTESIAN_POINT ( 'NONE',  ( 9.796875000614519990, -3.027376345333610441, -5.243569643749999898 ) ) ;
#67778 = ORIENTED_EDGE ( 'NONE', *, *, #24990, .F. ) ;
#67779 = CARTESIAN_POINT ( 'NONE',  ( -5.810221930991193690E-16, 14.03750000000000142, -34.00000000000000000 ) ) ;
#67780 = CARTESIAN_POINT ( 'NONE',  ( 23.76562500061451644, 3.027376345333613106, -5.243569643749998122 ) ) ;
#67781 = CARTESIAN_POINT ( 'NONE',  ( 30.00000000000000000, 0.000000000000000000, 0.000000000000000000 ) ) ;
#67782 = CARTESIAN_POINT ( 'NONE',  ( 26.62500000000000000, 6.123233995736764310E-16, -4.999999999999998224 ) ) ;
#67783 = CARTESIAN_POINT ( 'NONE',  ( 11.92500000000000071, 4.330127018922191873, 2.499999999999999556 ) ) ;
#67784 = CARTESIAN_POINT ( 'NONE',  ( 21.78750000122903074, 6.123233995736764310E-16, -4.999999999999998224 ) ) ;
#67785 = CARTESIAN_POINT ( 'NONE',  ( 16.37812500061451715, -4.541064518000419881, 2.621784821874995952 ) ) ;
#67786 = CARTESIAN_POINT ( 'NONE',  ( 12.27187500061451608, -4.119189519843968306, 2.378215178124996054 ) ) ;
#67787 = ORIENTED_EDGE ( 'NONE', *, *, #5869, .F. ) ;
#67788 = CARTESIAN_POINT ( 'NONE',  ( 20.47500000000000142, 4.330127018922191873, 2.499999999999999556 ) ) ;
#67789 = CARTESIAN_POINT ( 'NONE',  ( 23.69999999999999929, 0.000000000000000000, 4.999999999999998224 ) ) ;
#67790 = CARTESIAN_POINT ( 'NONE',  ( 22.09687500061451715, 6.054752690667223547, 3.707466751127219781E-16 ) ) ;
#67791 = CARTESIAN_POINT ( 'NONE',  ( 25.22812500061451502, 4.541064518000418104, 2.621784821874999949 ) ) ;
#67792 = ORIENTED_EDGE ( 'NONE', *, *, #44624, .T. ) ;
#67793 = CARTESIAN_POINT ( 'NONE',  ( 45.00000000000000000, 0.000000000000000000, 4.999999999999998224 ) ) ;
#67794 = CARTESIAN_POINT ( 'NONE',  ( 8.765625000614518214, -6.054752690667223547, -1.112240025338166033E-15 ) ) ;
#67795 = CARTESIAN_POINT ( 'NONE',  ( 3.313217074437887266, 3.744712918542242974, 3.512650841967440041 ) ) ;
#67796 = CARTESIAN_POINT ( 'NONE',  ( 15.18750000000000000, -2.886751345948129988, 4.999999999999997335 ) ) ;
#67797 = CARTESIAN_POINT ( 'NONE',  ( 9.001249775931846008E-16, 18.11562500061451786, 34.90005215228797653 ) ) ;
#67798 = CARTESIAN_POINT ( 'NONE',  ( 5.709375000614517859, -4.541064518000417216, -2.621784821875001281 ) ) ;
#67799 = VECTOR ( 'NONE', #37036, 1000.000000000000000 ) ;
#67800 = CARTESIAN_POINT ( 'NONE',  ( 26.37187500061451217, -6.054752690667223547, -1.112240025338166033E-15 ) ) ;
#67801 = VERTEX_POINT ( 'NONE', #14116 ) ;
#67802 = CARTESIAN_POINT ( 'NONE',  ( 23.42812500061451786, 4.541064518000418104, 2.621784821874999949 ) ) ;
#67803 = CARTESIAN_POINT ( 'NONE',  ( 24.72187500061451360, 3.027376345333613106, -5.243569643749998122 ) ) ;
#67804 = CARTESIAN_POINT ( 'NONE',  ( 2.121784821874999061, 19.20312500061459460, -33.67503911421598417 ) ) ;
#67805 = CARTESIAN_POINT ( 'NONE',  ( 12.18750000000000000, -2.886751345948125991, -5.000000000000000000 ) ) ;
#67806 = CARTESIAN_POINT ( 'NONE',  ( 8.390625000614518214, -3.027376345333610441, -5.243569643749999898 ) ) ;
#67807 = DIRECTION ( 'NONE',  ( -0.000000000000000000, -1.000000000000000000, -0.000000000000000000 ) ) ;
#67808 = CARTESIAN_POINT ( 'NONE',  ( 28.37812500061451715, 4.541064518000418104, 2.621784821874999949 ) ) ;
#67809 = CARTESIAN_POINT ( 'NONE',  ( 27.14062500061451644, -3.027376345333614438, 5.243569643749998122 ) ) ;
#67810 = CARTESIAN_POINT ( 'NONE',  ( 29.10937500061452354, 2.746126346562645981, -4.756430356249997438 ) ) ;
#67811 = CARTESIAN_POINT ( 'NONE',  ( 11.78437500061451892, 4.119189519843966529, 2.378215178124999607 ) ) ;
#67812 = CARTESIAN_POINT ( 'NONE',  ( 4.003125000614518925, 4.541064518000418104, -2.621784821874998173 ) ) ;
#67813 = CARTESIAN_POINT ( 'NONE',  ( 19.73437500061451644, 6.421520780324663323E-16, -5.243569643749999010 ) ) ;
#67815 = CARTESIAN_POINT ( 'NONE',  ( 4.243569643749999898, 14.68437500061451750, 30.00000000000000000 ) ) ;
#67814 =( BOUNDED_CURVE ( )  B_SPLINE_CURVE ( 2, ( #20860, #3525, #37494, #31591, #37856, #26046, #71112 ),
 .UNSPECIFIED., .F., .F. ) 
 B_SPLINE_CURVE_WITH_KNOTS ( ( 3, 2, 2, 3 ),
 ( 0.3300000000000000711, 0.3333333333333333703, 0.3366666666666667251, 0.3400000000000000799 ),
 .UNSPECIFIED. ) 
 CURVE ( )  GEOMETRIC_REPRESENTATION_ITEM ( )  RATIONAL_B_SPLINE_CURVE ( ( 0.9999999999999977796, 0.8660254037844409281, 1.000000000000000000, 0.8660254037844387076, 1.000000000000000000, 0.8660254037844364872, 1.000000000000002220 ) ) 
 REPRESENTATION_ITEM ( '' )  );
#67816 = CARTESIAN_POINT ( 'NONE',  ( 19.43437500061451928, 4.541064518000418104, 2.621784821874999949 ) ) ;
#67817 = CARTESIAN_POINT ( 'NONE',  ( 3.262500000000001510, 2.886751345948129099, -4.999999999999998224 ) ) ;
#67818 = CARTESIAN_POINT ( 'NONE',  ( 4.243569643749999898, 18.28437500061451715, 30.00000000000000000 ) ) ;
#67819 = CARTESIAN_POINT ( 'NONE',  ( 10.56562500061451715, -6.054752690667223547, -1.112240025338166033E-15 ) ) ;
#67820 = DIRECTION ( 'NONE',  ( -0.000000000000000000, -1.000000000000000000, -0.000000000000000000 ) ) ;
#67821 = CARTESIAN_POINT ( 'NONE',  ( 7.546875000614517326, -3.027376345333610441, -5.243569643749999898 ) ) ;
#67822 = CARTESIAN_POINT ( 'NONE',  ( 25.87500000122903643, 2.886751345948146419, -4.999999999999968914 ) ) ;
#67823 = CARTESIAN_POINT ( 'NONE',  ( 7.415625000614516793, -6.054752690667223547, -1.112240025338166033E-15 ) ) ;
#67824 = CARTESIAN_POINT ( 'NONE',  ( 12.87187500061451750, -6.054752690667223547, -1.112240025338166033E-15 ) ) ;
#67825 = CARTESIAN_POINT ( 'NONE',  ( 20.10000000122903074, 5.773502691896255534, 3.535250795749688894E-16 ) ) ;
#67826 = CARTESIAN_POINT ( 'NONE',  ( 6.009375000614519458, 0.000000000000000000, 5.243569643749999010 ) ) ;
#67827 = CARTESIAN_POINT ( 'NONE',  ( 8.803125000614517859, -4.541064518000417216, -2.621784821875001281 ) ) ;
#67828 = CARTESIAN_POINT ( 'NONE',  ( 5.840625000614517504, 6.054752690667223547, 3.707466751127219781E-16 ) ) ;
#67829 = CARTESIAN_POINT ( 'NONE',  ( 23.08125000122903359, 6.123233995736764310E-16, -4.999999999999998224 ) ) ;
#67830 = CARTESIAN_POINT ( 'NONE',  ( 19.35937500061451644, 4.541064518000418104, -2.621784821874998173 ) ) ;
#67831 = CARTESIAN_POINT ( 'NONE',  ( -3.999999999999997335, 11.60000000122903430, 32.30940107675850470 ) ) ;
#67832 = EDGE_LOOP ( 'NONE', ( #56417, #35908, #2806, #18880 ) ) ;
#67833 = CARTESIAN_POINT ( 'NONE',  ( 26.05312500061451431, 4.541064518000418104, -2.621784821874998173 ) ) ;
#67834 = CARTESIAN_POINT ( 'NONE',  ( 12.70312500061451821, 0.000000000000000000, 5.243569643749999010 ) ) ;
#67835 = CARTESIAN_POINT ( 'NONE',  ( 28.62187500061451573, -6.054752690667223547, -1.112240025338166033E-15 ) ) ;
#67836 = CARTESIAN_POINT ( 'NONE',  ( 13.04062500061451502, 6.054752690667223547, 3.707466751127219781E-16 ) ) ;
#67837 = CARTESIAN_POINT ( 'NONE',  ( 4.456355333853387890, -2.267705344768013553, -4.623151165536616425 ) ) ;
#67838 = CARTESIAN_POINT ( 'NONE',  ( 12.45000000122903394, 5.773502691896255534, 3.535250795749688894E-16 ) ) ;
#67839 = EDGE_CURVE ( 'NONE', #69508, #43636, #4166, .T. ) ;
#67840 = CARTESIAN_POINT ( 'NONE',  ( 26.65312500061451573, 0.000000000000000000, 5.243569643749999010 ) ) ;
#67841 = CARTESIAN_POINT ( 'NONE',  ( -3.000416591977282496E-16, 14.74062500061451786, -34.90005215228797653 ) ) ;
#67842 = CARTESIAN_POINT ( 'NONE',  ( 16.20000000122903216, -2.886751345948129988, 4.999999999999997335 ) ) ;
#67843 = AXIS2_PLACEMENT_3D ( 'NONE', #47482, #29051, #41943 ) ;
#67844 = CARTESIAN_POINT ( 'NONE',  ( 14.40000000000000036, -4.330127018922190985, -2.500000000000001332 ) ) ;
#67845 = CARTESIAN_POINT ( 'NONE',  ( 20.39062500061451644, -3.027376345333614438, 5.243569643749998122 ) ) ;
#67846 = CARTESIAN_POINT ( 'NONE',  ( 7.509375000614517681, -4.541064518000417216, -2.621784821875001281 ) ) ;
#67847 = CARTESIAN_POINT ( 'NONE',  ( 7.650000001229034119, -2.886751345948129988, 4.999999999999997335 ) ) ;
#67848 = CARTESIAN_POINT ( 'NONE',  ( 16.16250000122903430, 0.000000000000000000, 4.999999999999998224 ) ) ;
#67849 = CARTESIAN_POINT ( 'NONE',  ( 13.19062500061451537, -3.027376345333614438, 5.243569643749998122 ) ) ;
#67850 = CARTESIAN_POINT ( 'NONE',  ( 15.21562500061451750, 3.027376345333613106, -5.243569643749998122 ) ) ;
#67851 = CARTESIAN_POINT ( 'NONE',  ( 28.68750000122903288, 4.330127018922191873, 2.499999999999999556 ) ) ;
#67852 = CARTESIAN_POINT ( 'NONE',  ( 21.63749999999999929, -2.886751345948125991, -5.000000000000000000 ) ) ;
#67853 = CARTESIAN_POINT ( 'NONE',  ( 23.33437500061451786, 6.421520780324663323E-16, -5.243569643749999010 ) ) ;
#67854 = FACE_OUTER_BOUND ( 'NONE', #56945, .T. ) ;
#67855 = CARTESIAN_POINT ( 'NONE',  ( 9.525000001229033231, -5.773502691896255534, -1.060575238724906372E-15 ) ) ;
#67856 = CARTESIAN_POINT ( 'NONE',  ( 28.05937500061451573, 0.000000000000000000, 5.243569643749999010 ) ) ;
#67857 =( BOUNDED_CURVE ( )  B_SPLINE_CURVE ( 2, ( #19953, #13684, #46592, #53584, #36590, #65029, #42506, #63929, #18493 ),
 .UNSPECIFIED., .F., .F. ) 
 B_SPLINE_CURVE_WITH_KNOTS ( ( 3, 2, 2, 2, 3 ),
 ( 0.9305555555555555802, 0.9351851851851852304, 0.9444444444444444198, 0.9537037037037037202, 0.9583333333333333703 ),
 .UNSPECIFIED. ) 
 CURVE ( )  GEOMETRIC_REPRESENTATION_ITEM ( )  RATIONAL_B_SPLINE_CURVE ( ( 0.9330127018922194093, 0.9330127018922194093, 1.000000000000000000, 0.8660254037844387076, 1.000000000000000000, 0.8660254037844387076, 1.000000000000000000, 0.9330127018922185211, 0.9330127018922192983 ) ) 
 REPRESENTATION_ITEM ( '' )  );
#67858 = EDGE_CURVE ( 'NONE', #4158, #41395, #36655, .T. ) ;
#67859 = CARTESIAN_POINT ( 'NONE',  ( 5.034375000614519813, 4.541064518000418104, 2.621784821874999949 ) ) ;
#67860 = CARTESIAN_POINT ( 'NONE',  ( 23.01562500061451644, 3.027376345333611329, 5.243569643749999010 ) ) ;
#67861 = CARTESIAN_POINT ( 'NONE',  ( 2.655984681222220721E-16, 13.76562499938548534, 25.66244784525396483 ) ) ;
#67862 = CARTESIAN_POINT ( 'NONE',  ( 6.862500000000002487, 2.886751345948129099, -4.999999999999997335 ) ) ;
#67863 = CARTESIAN_POINT ( 'NONE',  ( 11.10937500061451644, -4.541064518000417216, -2.621784821875001281 ) ) ;
#67864 = DIRECTION ( 'NONE',  ( 0.000000000000000000, -0.000000000000000000, -1.000000000000000000 ) ) ;
#67865 = CARTESIAN_POINT ( 'NONE',  ( 2.896875000614518747, -3.027376345333614438, 5.243569643749998122 ) ) ;
#67866 = CARTESIAN_POINT ( 'NONE',  ( 7.621875000614519280, 3.027376345333613106, -5.243569643749998122 ) ) ;
#67867 = CARTESIAN_POINT ( 'NONE',  ( 6.750000000000002665, -4.330127018922190985, -2.500000000000001332 ) ) ;
#67868 = CARTESIAN_POINT ( 'NONE',  ( 27.38437500061451857, 6.421520780324663323E-16, -5.243569643749999010 ) ) ;
#67869 = CARTESIAN_POINT ( 'NONE',  ( 4.243569643749999010, 10.61562500061459602, 27.54997392385601174 ) ) ;
#67870 = CARTESIAN_POINT ( 'NONE',  ( 18.45000000000000284, -4.330127018922190985, -2.500000000000001332 ) ) ;
#67871 = ORIENTED_EDGE ( 'NONE', *, *, #5151, .T. ) ;
#67872 = CARTESIAN_POINT ( 'NONE',  ( 27.82499999999999929, -4.330127018922194537, 2.499999999999995559 ) ) ;
#67873 = CARTESIAN_POINT ( 'NONE',  ( 29.63437500061451502, 6.421520780324663323E-16, -5.243569643749999010 ) ) ;
#67874 = ORIENTED_EDGE ( 'NONE', *, *, #27421, .F. ) ;
#67875 = CARTESIAN_POINT ( 'NONE',  ( 14.80312500061451608, 4.541064518000418104, -2.621784821874998173 ) ) ;
#67876 = CARTESIAN_POINT ( 'NONE',  ( 7.303125000614516082, 0.000000000000000000, 5.243569643749999010 ) ) ;
#67877 = CARTESIAN_POINT ( 'NONE',  ( 19.95937500061451786, -5.492252693125287522, -1.008910452111647106E-15 ) ) ;
#67878 = CARTESIAN_POINT ( 'NONE',  ( 4.734375000614518214, -4.541064518000419881, 2.621784821874995952 ) ) ;
#67879 = CARTESIAN_POINT ( 'NONE',  ( 18.03750000122903430, -4.330127018922194537, 2.499999999999995559 ) ) ;
#67880 = CARTESIAN_POINT ( 'NONE',  ( 22.50000000000000000, -4.330127018922190985, -2.500000000000001332 ) ) ;
#67881 = CARTESIAN_POINT ( 'NONE',  ( 1.071796769724489895, 14.01740381056766793, -34.00000000000000000 ) ) ;
#67882 = CARTESIAN_POINT ( 'NONE',  ( 6.909375000614518036, 0.000000000000000000, 5.243569643749999010 ) ) ;
#67883 = CARTESIAN_POINT ( 'NONE',  ( 10.62187500061451928, -6.054752690667223547, -1.112240025338166033E-15 ) ) ;
#67884 = CARTESIAN_POINT ( 'NONE',  ( 21.34687500061451715, -3.027376345333614438, 5.243569643749998122 ) ) ;
#67885 = CARTESIAN_POINT ( 'NONE',  ( -2.000000000000000000, 16.32499999999999929, 26.53589838486224650 ) ) ;
#67886 = ORIENTED_EDGE ( 'NONE', *, *, #57999, .F. ) ;
#67887 = CARTESIAN_POINT ( 'NONE',  ( 4.734375000614518214, -4.541064518000419881, 2.621784821874995952 ) ) ;
#67888 = CARTESIAN_POINT ( 'NONE',  ( 6.234375000614519102, 6.421520780324663323E-16, -5.243569643749999010 ) ) ;
#67889 = CARTESIAN_POINT ( 'NONE',  ( 18.82500000000000284, -4.330127018922194537, 2.499999999999995559 ) ) ;
#67890 = CARTESIAN_POINT ( 'NONE',  ( 15.77812500061451573, 4.541064518000418104, 2.621784821874999949 ) ) ;
#67891 = CARTESIAN_POINT ( 'NONE',  ( 2.000000000000000444, 18.42500000000000071, 26.53589838486224650 ) ) ;
#67892 = CARTESIAN_POINT ( 'NONE',  ( 24.86250000122903359, -4.330127018922190985, -2.500000000000001332 ) ) ;
#67893 = CARTESIAN_POINT ( 'NONE',  ( 20.97187500061451715, -5.492252693125287522, -1.008910452111647106E-15 ) ) ;
#67894 = CARTESIAN_POINT ( 'NONE',  ( 10.19062500061451892, -3.027376345333610441, -5.243569643749999898 ) ) ;
#67895 = CARTESIAN_POINT ( 'NONE',  ( 27.68437500061451573, -4.541064518000419881, 2.621784821874995952 ) ) ;
#67896 = FACE_OUTER_BOUND ( 'NONE', #28902, .T. ) ;
#67897 = CARTESIAN_POINT ( 'NONE',  ( 28.47187500061451715, 3.027376345333611329, 5.243569643749999010 ) ) ;
#67898 = CARTESIAN_POINT ( 'NONE',  ( 9.262499999999999289, 2.886751345948126879, 4.999999999999999112 ) ) ;
#67899 = CARTESIAN_POINT ( 'NONE',  ( 2.000000000000001332, 14.41250000122903430, 33.46410161513774995 ) ) ;
#67900 = CARTESIAN_POINT ( 'NONE',  ( 9.562500001229032875, -4.330127018922190985, -2.500000000000001332 ) ) ;
#67901 = CIRCLE ( 'NONE', #12469, 10.00000000000000000 ) ;
#67902 = CARTESIAN_POINT ( 'NONE',  ( 20.18437500061451573, 6.421520780324663323E-16, -5.243569643749999010 ) ) ;
#67903 = CARTESIAN_POINT ( 'NONE',  ( 14.48437500061451821, 4.541064518000418104, 2.621784821874999949 ) ) ;
#67904 = CARTESIAN_POINT ( 'NONE',  ( 45.00000000000000000, 0.000000000000000000, 0.000000000000000000 ) ) ;
#67905 = ORIENTED_EDGE ( 'NONE', *, *, #10225, .T. ) ;
#67906 = CARTESIAN_POINT ( 'NONE',  ( 13.79062500061451502, -3.027376345333610441, -5.243569643749999898 ) ) ;
#67907 = VECTOR ( 'NONE', #39987, 1000.000000000000000 ) ;
#67908 = CARTESIAN_POINT ( 'NONE',  ( 26.17500000122903359, -5.773502691896255534, -1.060575238724906372E-15 ) ) ;
#67909 = CARTESIAN_POINT ( 'NONE',  ( 15.68437500061451573, 6.421520780324663323E-16, -5.243569643749999010 ) ) ;
#67910 = CARTESIAN_POINT ( 'NONE',  ( 3.403125000614518836, -4.541064518000417216, -2.621784821875001281 ) ) ;
#67911 = CARTESIAN_POINT ( 'NONE',  ( 17.05312500061451786, 4.541064518000418104, -2.621784821874998173 ) ) ;
#67912 = CARTESIAN_POINT ( 'NONE',  ( 20.88750000122903572, 6.123233995736764310E-16, -4.999999999999998224 ) ) ;
#67913 = CARTESIAN_POINT ( 'NONE',  ( 25.50937500061451502, -4.541064518000417216, -2.621784821875001281 ) ) ;
#67914 = CARTESIAN_POINT ( 'NONE',  ( -4.243569643749997233, 10.39062500061451644, 32.45002607614398471 ) ) ;
#67915 = CARTESIAN_POINT ( 'NONE',  ( 15.45937500061451608, 0.000000000000000000, 5.243569643749999010 ) ) ;
#67916 = CARTESIAN_POINT ( 'NONE',  ( 14.02500000122903323, -5.773502691896255534, -1.060575238724906372E-15 ) ) ;
#67917 = CARTESIAN_POINT ( 'NONE',  ( 8.371875000614515727, -5.492252693125287522, -1.008910452111647106E-15 ) ) ;
#67918 = CARTESIAN_POINT ( 'NONE',  ( 4.243569643749999898, 15.99687500061451573, -27.54997392385601529 ) ) ;
#67919 = CARTESIAN_POINT ( 'NONE',  ( 18.49687500061452283, 6.054752690667223547, 3.707466751127219781E-16 ) ) ;
#67920 = CARTESIAN_POINT ( 'NONE',  ( 20.51250000122903216, 4.330127018922192761, -2.499999999999997780 ) ) ;
#67921 = CARTESIAN_POINT ( 'NONE',  ( 14.40937500061451715, 4.541064518000418104, -2.621784821874998173 ) ) ;
#67922 = CARTESIAN_POINT ( 'NONE',  ( -2.121784821874999949, 13.48437500061451821, 26.32496088578401938 ) ) ;
#67923 = CARTESIAN_POINT ( 'NONE',  ( 23.47500000122903430, -5.773502691896255534, -1.060575238724906372E-15 ) ) ;
#67924 = CARTESIAN_POINT ( 'NONE',  ( 14.46562500061451750, 3.027376345333611329, 5.243569643749999010 ) ) ;
#67925 = CARTESIAN_POINT ( 'NONE',  ( 29.39062500061451289, -3.027376345333614438, 5.243569643749998122 ) ) ;
#67926 = VERTEX_POINT ( 'NONE', #35562 ) ;
#67927 = ORIENTED_EDGE ( 'NONE', *, *, #8491, .T. ) ;
#67928 = CARTESIAN_POINT ( 'NONE',  ( 20.69999999999999929, -4.330127018922190985, -2.500000000000001332 ) ) ;
#67929 = CARTESIAN_POINT ( 'NONE',  ( -3.999999999999999112, 17.82500000122903572, 27.69059892324149885 ) ) ;
#67930 = CARTESIAN_POINT ( 'NONE',  ( 3.779877903161418473, 3.276378095916668620, 28.66642532236455665 ) ) ;
#67931 = CARTESIAN_POINT ( 'NONE',  ( 16.08750000122903501, 4.330127018922191873, 2.499999999999999556 ) ) ;
#67932 = CARTESIAN_POINT ( 'NONE',  ( 19.71562500061451928, 3.027376345333613106, -5.243569643749998122 ) ) ;
#67933 = CARTESIAN_POINT ( 'NONE',  ( 23.42812500061451786, 4.541064518000418104, 2.621784821874999949 ) ) ;
#67934 = CARTESIAN_POINT ( 'NONE',  ( 6.328125000614515550, 4.541064518000418104, 2.621784821874999949 ) ) ;
#67935 = CARTESIAN_POINT ( 'NONE',  ( -2.000000000000001776, 20.39374999877096428, 33.46410161513775705 ) ) ;
#67936 = CARTESIAN_POINT ( 'NONE',  ( 4.589319506978690733, 1.984554166263133856, 4.853542117982821757 ) ) ;
#67937 = AXIS2_PLACEMENT_3D ( 'NONE', #69721, #40935, #58982 ) ;
#67938 = CARTESIAN_POINT ( 'NONE',  ( 9.121875000614517504, 2.746126346562643317, 4.756430356249998326 ) ) ;
#67939 = CYLINDRICAL_SURFACE ( 'NONE', #18176, 4.000000000000000000 ) ;
#67940 = CARTESIAN_POINT ( 'NONE',  ( 1.999999999999998668, 10.51250000122903572, -33.46410161513775705 ) ) ;
#67941 = CARTESIAN_POINT ( 'NONE',  ( -4.243569643749997233, 19.44687500061451502, -27.54997392385601174 ) ) ;
#67942 = CARTESIAN_POINT ( 'NONE',  ( 6.750000001229033764, -2.886751345948129988, 4.999999999999997335 ) ) ;
#67943 = CARTESIAN_POINT ( 'NONE',  ( 7.312500000000000000, 2.886751345948129099, -4.999999999999998224 ) ) ;
#67944 = ADVANCED_FACE ( 'NONE', ( #31113 ), #19280, .F. ) ;
#67945 = CARTESIAN_POINT ( 'NONE',  ( 3.375000001229033320, 2.886751345948129099, -4.999999999999998224 ) ) ;
#67946 = CARTESIAN_POINT ( 'NONE',  ( 12.83437500061451786, -4.541064518000419881, 2.621784821874995952 ) ) ;
#67947 = CARTESIAN_POINT ( 'NONE',  ( 24.67500000122903359, 2.886751345948126879, 4.999999999999998224 ) ) ;
#67948 = CARTESIAN_POINT ( 'NONE',  ( 3.271875000614519635, 3.027376345333611329, 5.243569643749999010 ) ) ;
#67949 = CARTESIAN_POINT ( 'NONE',  ( -5.810221930991193690E-16, 15.83749999999999680, 26.00000000000000355 ) ) ;
#67950 = VECTOR ( 'NONE', #19039, 1000.000000000000000 ) ;
#67951 = CARTESIAN_POINT ( 'NONE',  ( 9.562500000000001776, 2.886751345948129099, -4.999999999999997335 ) ) ;
#67952 = CARTESIAN_POINT ( 'NONE',  ( 9.871875000614517504, 3.027376345333613106, -5.243569643749998122 ) ) ;
#67953 = CARTESIAN_POINT ( 'NONE',  ( 12.98437500061451821, 6.421520780324663323E-16, -5.243569643749999010 ) ) ;
#67954 = CARTESIAN_POINT ( 'NONE',  ( -1.071796769724488563, 18.74240381056766935, -26.00000000000000000 ) ) ;
#67955 = CARTESIAN_POINT ( 'NONE',  ( 6.187500000000002665, -2.886751345948129988, 4.999999999999997335 ) ) ;
#67956 = CARTESIAN_POINT ( 'NONE',  ( 4.243569643749999898, 16.39062500061459815, 32.45002607614398471 ) ) ;
#67957 = CARTESIAN_POINT ( 'NONE',  ( 21.57187500061451502, 3.027376345333613106, -5.243569643749998122 ) ) ;
#67958 = CARTESIAN_POINT ( 'NONE',  ( 27.48750000122903359, -4.330127018922194537, 2.499999999999995559 ) ) ;
#67959 = CARTESIAN_POINT ( 'NONE',  ( 18.79687500061451289, 4.119189519843966529, -2.378215178124998275 ) ) ;
#67960 = CARTESIAN_POINT ( 'NONE',  ( 23.61562500061451431, -6.054752690667223547, -1.112240025338166033E-15 ) ) ;
#67961 = CARTESIAN_POINT ( 'NONE',  ( 15.17812500061451608, 6.421520780324663323E-16, -5.243569643749999010 ) ) ;
#67962 = CARTESIAN_POINT ( 'NONE',  ( 25.32187500061451502, -4.119189519843968306, 2.378215178124996054 ) ) ;
#67963 = CARTESIAN_POINT ( 'NONE',  ( 12.53437500061451537, 6.421520780324663323E-16, -5.243569643749999010 ) ) ;
#67964 = CARTESIAN_POINT ( 'NONE',  ( 27.71250000000000568, 2.886751345948126879, 4.999999999999999112 ) ) ;
#67965 = CARTESIAN_POINT ( 'NONE',  ( 24.78750000122903074, -4.330127018922194537, 2.499999999999995559 ) ) ;
#67966 = CARTESIAN_POINT ( 'NONE',  ( 3.721875000614518036, 3.027376345333611329, 5.243569643749999010 ) ) ;
#67967 = CARTESIAN_POINT ( 'NONE',  ( 13.62187500061451750, 3.027376345333611329, 5.243569643749999010 ) ) ;
#67968 = CARTESIAN_POINT ( 'NONE',  ( 28.62187500061451573, -6.054752690667223547, -1.112240025338166033E-15 ) ) ;
#67969 = CYLINDRICAL_SURFACE ( 'NONE', #54859, 4.999999999999998224 ) ;
#67970 = CARTESIAN_POINT ( 'NONE',  ( 24.03750000122903430, 6.123233995736764310E-16, -4.999999999999998224 ) ) ;
#67971 = CARTESIAN_POINT ( 'NONE',  ( 22.13437500061451502, 4.541064518000418104, 2.621784821874999949 ) ) ;
#67972 = CARTESIAN_POINT ( 'NONE',  ( 14.07187500061451679, 3.027376345333611329, 5.243569643749999010 ) ) ;
#67973 = CARTESIAN_POINT ( 'NONE',  ( 2.655984681222220721E-16, 16.01562499938548356, 25.66244784525396483 ) ) ;
#67974 = CARTESIAN_POINT ( 'NONE',  ( 25.68750000000000000, -2.886751345948125991, -5.000000000000000000 ) ) ;
#67975 = CARTESIAN_POINT ( 'NONE',  ( 4.087500001229035007, -4.330127018922194537, 2.499999999999995559 ) ) ;
#67976 = CARTESIAN_POINT ( 'NONE',  ( 28.65937500061451715, -4.119189519843965641, -2.378215178125001383 ) ) ;
#67977 = CARTESIAN_POINT ( 'NONE',  ( 16.19062500061451715, 6.054752690667223547, 3.707466751127219781E-16 ) ) ;
#67978 = CARTESIAN_POINT ( 'NONE',  ( 6.562500000000001776, 2.886751345948126879, 4.999999999999999112 ) ) ;
#67979 = CARTESIAN_POINT ( 'NONE',  ( -5.810221930991193690E-16, 14.03750000000000142, 26.00000000000000355 ) ) ;
#67980 = CARTESIAN_POINT ( 'NONE',  ( 16.46249999999999503, 2.886751345948126879, 4.999999999999999112 ) ) ;
#67981 = CARTESIAN_POINT ( 'NONE',  ( 4.243569643749999898, 13.24062500061451786, 32.45002607614398471 ) ) ;
#67982 = CARTESIAN_POINT ( 'NONE',  ( 14.47499999999999964, 6.123233995736764310E-16, -4.999999999999998224 ) ) ;
#67983 = CARTESIAN_POINT ( 'NONE',  ( 21.86250000122903003, 4.330127018922192761, -2.499999999999997780 ) ) ;
#67984 = CARTESIAN_POINT ( 'NONE',  ( 1.594043775273459307, 9.879932731042712746, 24.20196496940534914 ) ) ;
#67985 = CARTESIAN_POINT ( 'NONE',  ( 27.60937500061451644, 0.000000000000000000, 5.243569643749999010 ) ) ;
#67986 = ORIENTED_EDGE ( 'NONE', *, *, #53130, .F. ) ;
#67987 = CARTESIAN_POINT ( 'NONE',  ( 22.60312500061451857, 0.000000000000000000, 5.243569643749999010 ) ) ;
#67988 = CARTESIAN_POINT ( 'NONE',  ( 23.29687500061451644, -3.027376345333610441, -5.243569643749999898 ) ) ;
#67989 = CARTESIAN_POINT ( 'NONE',  ( 5.812500000000001776, -5.773502691896255534, -1.060575238724906372E-15 ) ) ;
#67990 = CARTESIAN_POINT ( 'NONE',  ( 8.765625000614518214, -6.054752690667223547, -1.112240025338166033E-15 ) ) ;
#67991 = CARTESIAN_POINT ( 'NONE',  ( 24.81562500061451715, 3.027376345333611329, 5.243569643749999010 ) ) ;
#67992 = CARTESIAN_POINT ( 'NONE',  ( 13.35937500061451821, -4.541064518000417216, -2.621784821875001281 ) ) ;
#67993 = CARTESIAN_POINT ( 'NONE',  ( 16.05937500061451573, -4.541064518000417216, -2.621784821875001281 ) ) ;
#67994 = CARTESIAN_POINT ( 'NONE',  ( -0.6945831915928805111, 10.00052343484236950, 26.06076730949330411 ) ) ;
#67995 = CARTESIAN_POINT ( 'NONE',  ( -2.121784821874999949, 17.92812500061451786, 26.32496088578401938 ) ) ;
#67996 = CARTESIAN_POINT ( 'NONE',  ( 20.58750000122903145, 4.330127018922191873, 2.499999999999999556 ) ) ;
#67997 = CARTESIAN_POINT ( 'NONE',  ( 14.74687500061451750, -2.746126346562641984, -4.756430356249999214 ) ) ;
#67998 = CARTESIAN_POINT ( 'NONE',  ( 12.77812500061451750, -4.541064518000419881, 2.621784821874995952 ) ) ;
#67999 = CARTESIAN_POINT ( 'NONE',  ( 6.534375000614517148, -4.541064518000419881, 2.621784821874995952 ) ) ;
#68000 = CARTESIAN_POINT ( 'NONE',  ( 3.796875000614517326, -3.027376345333614438, 5.243569643749998122 ) ) ;
#68001 = ORIENTED_EDGE ( 'NONE', *, *, #29363, .F. ) ;
#68002 = CARTESIAN_POINT ( 'NONE',  ( 26.52187500061451431, 3.027376345333613106, -5.243569643749998122 ) ) ;
#68003 = CARTESIAN_POINT ( 'NONE',  ( 18.02812500061451573, 4.541064518000418104, 2.621784821874999949 ) ) ;
#68004 = CARTESIAN_POINT ( 'NONE',  ( 26.85000000122903430, 5.773502691896255534, 3.535250795749688894E-16 ) ) ;
#68005 = EDGE_CURVE ( 'NONE', #49299, #70914, #58917, .T. ) ;
#68006 = CARTESIAN_POINT ( 'NONE',  ( 28.30312500061451431, 4.541064518000418104, -2.621784821874998173 ) ) ;
#68007 = CARTESIAN_POINT ( 'NONE',  ( 22.88437500061451857, 6.421520780324663323E-16, -5.243569643749999010 ) ) ;
#68008 = CARTESIAN_POINT ( 'NONE',  ( 16.15312500061451573, 4.541064518000418104, -2.621784821874998173 ) ) ;
#68009 = CARTESIAN_POINT ( 'NONE',  ( 2.121784821874999061, 19.70937500061451786, 26.32496088578401583 ) ) ;
#68010 = CARTESIAN_POINT ( 'NONE',  ( 21.55312500061451431, 4.541064518000418104, -2.621784821874998173 ) ) ;
#68011 = CARTESIAN_POINT ( 'NONE',  ( 3.975000001229033852, 2.886751345948126879, 4.999999999999999112 ) ) ;
#68012 = EDGE_LOOP ( 'NONE', ( #66045, #24918, #29901, #24480 ) ) ;
#68013 = CARTESIAN_POINT ( 'NONE',  ( 27.71250000000000568, 2.886751345948126879, 4.999999999999999112 ) ) ;
#68014 = CARTESIAN_POINT ( 'NONE',  ( -3.999999999999999112, 11.90000000000000036, -30.00000000000000000 ) ) ;
#68015 = CARTESIAN_POINT ( 'NONE',  ( -1.878215178125001827, 18.00312499938548427, 33.25316411605952283 ) ) ;
#68016 = CARTESIAN_POINT ( 'NONE',  ( 28.90312500061451217, 0.000000000000000000, 5.243569643749999010 ) ) ;
#68017 = CARTESIAN_POINT ( 'NONE',  ( 10.97812500061451679, -4.541064518000419881, 2.621784821874995952 ) ) ;
#68018 = CARTESIAN_POINT ( 'NONE',  ( 22.53750000122903430, -4.330127018922194537, 2.499999999999995559 ) ) ;
#68019 = CARTESIAN_POINT ( 'NONE',  ( 12.87187500061451750, -6.054752690667223547, -1.112240025338166033E-15 ) ) ;
#68020 = CARTESIAN_POINT ( 'NONE',  ( 26.24062500061451431, -3.027376345333614438, 5.243569643749998122 ) ) ;
#68021 = CARTESIAN_POINT ( 'NONE',  ( 27.89999999999999858, -4.330127018922190985, -2.500000000000001332 ) ) ;
#68022 = CARTESIAN_POINT ( 'NONE',  ( -2.000000000000000000, 18.23750000122903359, -33.46410161513775705 ) ) ;
#68023 = SHAPE_REPRESENTATION ( 'knob', ( #23765 ), #19014 ) ;
#68024 = CARTESIAN_POINT ( 'NONE',  ( 2.990625000614519191, -3.027376345333610441, -5.243569643749999898 ) ) ;
#68025 = CARTESIAN_POINT ( 'NONE',  ( 12.02812500061451573, 6.421520780324663323E-16, -5.243569643749999010 ) ) ;
#68026 = VERTEX_POINT ( 'NONE', #69557 ) ;
#68027 = CARTESIAN_POINT ( 'NONE',  ( 7.528125000614515727, 6.421520780324663323E-16, -5.243569643749999010 ) ) ;
#68028 = CARTESIAN_POINT ( 'NONE',  ( 4.865625000614517859, 3.027376345333613106, -5.243569643749998122 ) ) ;
#68029 = AXIS2_PLACEMENT_3D ( 'NONE', #26181, #64969, #37990 ) ;
#68030 = CARTESIAN_POINT ( 'NONE',  ( 16.05937500061451573, -4.119189519843965641, -2.378215178125001383 ) ) ;
#68031 = EDGE_CURVE ( 'NONE', #71801, #16431, #36296, .T. ) ;
#68032 = CARTESIAN_POINT ( 'NONE',  ( 14.13750000122903394, 6.123233995736764310E-16, -4.999999999999998224 ) ) ;
#68033 = CARTESIAN_POINT ( 'NONE',  ( 15.93750000000000000, 5.773502691896255534, 3.535250795749688894E-16 ) ) ;
#68034 = CARTESIAN_POINT ( 'NONE',  ( 15.75937500061451857, 4.541064518000418104, -2.621784821874998173 ) ) ;
#68035 = CARTESIAN_POINT ( 'NONE',  ( 10.87500000122903288, -5.773502691896255534, -1.060575238724906372E-15 ) ) ;
#68036 = CARTESIAN_POINT ( 'NONE',  ( 19.99687500061451573, -3.027376345333614438, 5.243569643749998122 ) ) ;
#68037 = CARTESIAN_POINT ( 'NONE',  ( 20.06250000000000000, 2.886751345948126879, 4.999999999999999112 ) ) ;
#68038 = AXIS2_PLACEMENT_3D ( 'NONE', #35483, #69122, #1523 ) ;
#68039 = CARTESIAN_POINT ( 'NONE',  ( 19.84687500061451360, 6.054752690667223547, 3.707466751127219781E-16 ) ) ;
#68040 = CARTESIAN_POINT ( 'NONE',  ( -4.243569643749999898, 14.81562500061451715, -32.45002607614398471 ) ) ;
#68041 = CARTESIAN_POINT ( 'NONE',  ( 25.58437500061451431, 5.492252693125287522, 3.363034840372157021E-16 ) ) ;
#68042 = CARTESIAN_POINT ( 'NONE',  ( 3.144856541311010556, 3.887142566792906706, -3.519253510942787599 ) ) ;
#68043 = CARTESIAN_POINT ( 'NONE',  ( 27.02812500061451573, 4.541064518000418104, 2.621784821874999949 ) ) ;
#68044 = DIRECTION ( 'NONE',  ( 0.000000000000000000, 0.000000000000000000, 1.000000000000000000 ) ) ;
#68045 = CARTESIAN_POINT ( 'NONE',  ( 28.62187500061451573, -6.054752690667223547, -1.112240025338166033E-15 ) ) ;
#68046 = EDGE_CURVE ( 'NONE', #6716, #9071, #23982, .T. ) ;
#68047 = CARTESIAN_POINT ( 'NONE',  ( 24.37500000000000000, 6.123233995736764310E-16, -4.999999999999998224 ) ) ;
#68048 = CARTESIAN_POINT ( 'NONE',  ( 9.853125000614516793, 4.541064518000418104, -2.621784821874998173 ) ) ;
#68049 = CARTESIAN_POINT ( 'NONE',  ( 25.24687500061451217, 0.000000000000000000, 4.756430356249998326 ) ) ;
#68050 = CARTESIAN_POINT ( 'NONE',  ( 19.77187500061451786, 3.027376345333613106, -5.243569643749998122 ) ) ;
#68051 = CARTESIAN_POINT ( 'NONE',  ( 11.78437500061451537, -2.746126346562646425, 4.756430356249996549 ) ) ;
#68052 = CARTESIAN_POINT ( 'NONE',  ( 6.215625000614517504, 3.027376345333613106, -5.243569643749998122 ) ) ;
#68053 = CARTESIAN_POINT ( 'NONE',  ( 10.47187500061451715, 3.027376345333611329, 5.243569643749999010 ) ) ;
#68054 = ORIENTED_EDGE ( 'NONE', *, *, #12973, .F. ) ;
#68055 = CARTESIAN_POINT ( 'NONE',  ( 21.34687500061451715, -3.027376345333614438, 5.243569643749998122 ) ) ;
#68056 = CARTESIAN_POINT ( 'NONE',  ( 8.156250001229034652, -4.330127018922190985, -2.500000000000001332 ) ) ;
#68057 = CARTESIAN_POINT ( 'NONE',  ( 28.38749999999999929, -2.886751345948125991, -5.000000000000000000 ) ) ;
#68058 =( BOUNDED_CURVE ( )  B_SPLINE_CURVE ( 2, ( #39870, #45401, #28405, #62745, #57560, #29135, #7323 ),
 .UNSPECIFIED., .F., .F. ) 
 B_SPLINE_CURVE_WITH_KNOTS ( ( 3, 2, 2, 3 ),
 ( 0.5200000000000000178, 0.5233333333333333171, 0.5266666666666666163, 0.5300000000000000266 ),
 .UNSPECIFIED. ) 
 CURVE ( )  GEOMETRIC_REPRESENTATION_ITEM ( )  RATIONAL_B_SPLINE_CURVE ( ( 1.000000000000000000, 0.8660254037844387076, 1.000000000000000000, 0.8660254037844387076, 1.000000000000000000, 0.8660254037844387076, 1.000000000000000000 ) ) 
 REPRESENTATION_ITEM ( '' )  );
#68059 = CARTESIAN_POINT ( 'NONE',  ( 29.52187500061451431, -6.054752690667223547, -1.112240025338166033E-15 ) ) ;
#68060 = CARTESIAN_POINT ( 'NONE',  ( 1.071796769724484344, 15.18259618943233669, -25.99999999999999645 ) ) ;
#68061 = CARTESIAN_POINT ( 'NONE',  ( 12.31875000122903430, 2.886751345948073588, -5.000000000000094147 ) ) ;
#68062 = ORIENTED_EDGE ( 'NONE', *, *, #57008, .F. ) ;
#68063 = CARTESIAN_POINT ( 'NONE',  ( 12.93750000000000178, -2.886751345948129988, 4.999999999999997335 ) ) ;
#68064 = CARTESIAN_POINT ( 'NONE',  ( 14.40937500061451537, 2.746126346562643317, 4.756430356249998326 ) ) ;
#68065 = CARTESIAN_POINT ( 'NONE',  ( 23.54062500061451146, -3.027376345333614438, 5.243569643749998122 ) ) ;
#68066 = CARTESIAN_POINT ( 'NONE',  ( 15.11249999999999893, 2.886751345948126879, 4.999999999999999112 ) ) ;
#68067 = CARTESIAN_POINT ( 'NONE',  ( 9.375000001229036428, 2.886751345948126879, 4.999999999999999112 ) ) ;
#68068 = CARTESIAN_POINT ( 'NONE',  ( 8.278125000614515727, -4.541064518000419881, 2.621784821874995952 ) ) ;
#68069 = CARTESIAN_POINT ( 'NONE',  ( 7.987500000000000711, -2.886751345948129988, 4.999999999999997335 ) ) ;
#68070 = CARTESIAN_POINT ( 'NONE',  ( 0.6945827174705067053, 27.50000000000000000, 33.93923277410605976 ) ) ;
#68071 = CARTESIAN_POINT ( 'NONE',  ( 28.72500000122903074, 2.886751345948126879, 4.999999999999999112 ) ) ;
#68072 = CARTESIAN_POINT ( 'NONE',  ( -1.878215178125001827, 16.54062499938548569, 33.25316411605952283 ) ) ;
#68073 = CARTESIAN_POINT ( 'NONE',  ( 7.837499999999999467, 5.773502691896255534, 3.535250795749688894E-16 ) ) ;
#68074 = CARTESIAN_POINT ( 'NONE',  ( 18.78749999999999432, -2.886751345948074920, 5.000000000000092371 ) ) ;
#68075 = ORIENTED_EDGE ( 'NONE', *, *, #26600, .T. ) ;
#68076 = CARTESIAN_POINT ( 'NONE',  ( 21.47812500061451502, 6.421520780324663323E-16, -5.243569643749999010 ) ) ;
#68077 = CARTESIAN_POINT ( 'NONE',  ( 28.30312500061451431, 4.541064518000418104, -2.621784821874998173 ) ) ;
#68078 = CARTESIAN_POINT ( 'NONE',  ( 29.55937500061451573, -4.541064518000417216, -2.621784821875001281 ) ) ;
#68079 = CARTESIAN_POINT ( 'NONE',  ( 19.92187500061451644, 3.027376345333611329, 5.243569643749999010 ) ) ;
#68080 = CARTESIAN_POINT ( 'NONE',  ( 16.97812500061451502, 6.421520780324663323E-16, -5.243569643749999010 ) ) ;
#68081 = AXIS2_PLACEMENT_3D ( 'NONE', #24676, #13587, #58653 ) ;
#68082 = CARTESIAN_POINT ( 'NONE',  ( 9.001249775931846008E-16, 12.26562500061459637, -25.09994784771203058 ) ) ;
#68083 = CARTESIAN_POINT ( 'NONE',  ( 5.690625000614516260, -3.027376345333610441, -5.243569643749999898 ) ) ;
#68084 = VECTOR ( 'NONE', #17283, 1000.000000000000000 ) ;
#68085 = CARTESIAN_POINT ( 'NONE',  ( 28.31250000122903288, 0.000000000000000000, 4.999999999999998224 ) ) ;
#68086 = CARTESIAN_POINT ( 'NONE',  ( 20.74687500061452283, 5.492252693125287522, 3.363034840372157021E-16 ) ) ;
#68087 = CARTESIAN_POINT ( 'NONE',  ( 19.37812500061451715, 4.541064518000418104, 2.621784821874999949 ) ) ;
#68088 = CARTESIAN_POINT ( 'NONE',  ( 3.999999999999998668, 11.37500000122903643, -32.30940107675850470 ) ) ;
#68089 = CARTESIAN_POINT ( 'NONE',  ( 4.462500001229035007, 0.000000000000000000, 4.999999999999998224 ) ) ;
#68090 = CARTESIAN_POINT ( 'NONE',  ( 13.54687500061451999, 6.054752690667223547, 3.707466751127219781E-16 ) ) ;
#68091 = CARTESIAN_POINT ( 'NONE',  ( 11.74687500061451573, 6.054752690667223547, 3.707466751127219781E-16 ) ) ;
#68092 = CARTESIAN_POINT ( 'NONE',  ( 20.14687500061451786, -3.027376345333610441, -5.243569643749999898 ) ) ;
#68093 = ORIENTED_EDGE ( 'NONE', *, *, #62835, .F. ) ;
#68094 = CARTESIAN_POINT ( 'NONE',  ( 29.51249999999999929, 2.886751345948106007, 5.000000000000033751 ) ) ;
#68095 = CARTESIAN_POINT ( 'NONE',  ( 23.84062500061451928, 6.054752690667223547, 3.707466751127219781E-16 ) ) ;
#68096 =( BOUNDED_CURVE ( )  B_SPLINE_CURVE ( 2, ( #18019, #2497, #64914, #65275, #2863, #9503, #25021 ),
 .UNSPECIFIED., .F., .F. ) 
 B_SPLINE_CURVE_WITH_KNOTS ( ( 3, 2, 2, 3 ),
 ( 0.3833333333333333037, 0.3861111111111111271, 0.3888888888888889506, 0.3916666666666667740 ),
 .UNSPECIFIED. ) 
 CURVE ( )  GEOMETRIC_REPRESENTATION_ITEM ( )  RATIONAL_B_SPLINE_CURVE ( ( 1.000000000000002665, 0.8660254037844360431, 1.000000000000000000, 0.8660254037844387076, 1.000000000000000000, 0.8660254037844333785, 1.000000000000005329 ) ) 
 REPRESENTATION_ITEM ( '' )  );
#68097 = CARTESIAN_POINT ( 'NONE',  ( 18.30937500061451928, -4.541064518000417216, -2.621784821875001281 ) ) ;
#68098 = CARTESIAN_POINT ( 'NONE',  ( 25.04062500061451502, -3.027376345333610441, -5.243569643749999898 ) ) ;
#68099 = CARTESIAN_POINT ( 'NONE',  ( -3.999999999999999112, 17.75000000000000355, 30.00000000000000000 ) ) ;
#68100 = CARTESIAN_POINT ( 'NONE',  ( 5.521875000614517859, 3.027376345333611329, 5.243569643749999010 ) ) ;
#68101 = CARTESIAN_POINT ( 'NONE',  ( 10.87500000122903288, -5.773502691896255534, -1.060575238724906372E-15 ) ) ;
#68102 = CARTESIAN_POINT ( 'NONE',  ( 7.350000001229033408, -2.886751345948125991, -5.000000000000000000 ) ) ;
#68103 = CARTESIAN_POINT ( 'NONE',  ( 2.000000000000001332, 19.25000000000000000, -26.53589838486224650 ) ) ;
#68104 = CARTESIAN_POINT ( 'NONE',  ( 27.63750000122903216, 6.123233995736764310E-16, -4.999999999999998224 ) ) ;
#68105 = CARTESIAN_POINT ( 'NONE',  ( 3.999999999999998668, 17.80624999877096215, 32.30940107675850470 ) ) ;
#68106 = CARTESIAN_POINT ( 'NONE',  ( 15.61875000122903323, 2.886751345948126879, 4.999999999999999112 ) ) ;
#68107 = CARTESIAN_POINT ( 'NONE',  ( 10.24687500061451750, -3.027376345333610441, -5.243569643749999898 ) ) ;
#68108 = DIRECTION ( 'NONE',  ( -0.000000000000000000, -1.000000000000000000, -0.000000000000000000 ) ) ;
#68109 = CARTESIAN_POINT ( 'NONE',  ( 18.51562500061451289, 3.027376345333611329, 5.243569643749999010 ) ) ;
#68110 = CARTESIAN_POINT ( 'NONE',  ( 14.33437500061451786, 6.421520780324663323E-16, -5.243569643749999010 ) ) ;
#68111 = CARTESIAN_POINT ( 'NONE',  ( 29.28750000122903074, -4.330127018922194537, 2.499999999999995559 ) ) ;
#68112 = CARTESIAN_POINT ( 'NONE',  ( 20.70937500061451786, 4.541064518000418104, -2.621784821874998173 ) ) ;
#68113 = CARTESIAN_POINT ( 'NONE',  ( 8.109375000614518214, 4.541064518000418104, -2.621784821874998173 ) ) ;
#68114 = CARTESIAN_POINT ( 'NONE',  ( 3.778125000614519280, -4.541064518000419881, 2.621784821874995952 ) ) ;
#68115 = CARTESIAN_POINT ( 'NONE',  ( -3.999999999999999112, 17.75000000000000355, 30.00000000000000000 ) ) ;
#68116 = ADVANCED_FACE ( 'NONE', ( #64364 ), #54029, .T. ) ;
#68117 = CARTESIAN_POINT ( 'NONE',  ( 20.09062500061451573, -3.027376345333610441, -5.243569643749999898 ) ) ;
#68118 = VERTEX_POINT ( 'NONE', #24111 ) ;
#68119 = CARTESIAN_POINT ( 'NONE',  ( 6.225000001229036073, 2.886751345948126879, 4.999999999999999112 ) ) ;
#68120 =( BOUNDED_CURVE ( )  B_SPLINE_CURVE ( 2, ( #50738, #11211, #43741, #61449, #5306, #10121, #61086, #32651, #50382 ),
 .UNSPECIFIED., .F., .F. ) 
 B_SPLINE_CURVE_WITH_KNOTS ( ( 3, 2, 2, 2, 3 ),
 ( 0.4673913043478261087, 0.4710144927536231707, 0.4782608695652174058, 0.4855072463768115854, 0.4891304347826087029 ),
 .UNSPECIFIED. ) 
 CURVE ( )  GEOMETRIC_REPRESENTATION_ITEM ( )  RATIONAL_B_SPLINE_CURVE ( ( 0.9330127018922194093, 0.9330127018922198534, 1.000000000000000000, 0.8660254037844387076, 1.000000000000000000, 0.8660254037844387076, 1.000000000000000000, 0.9330127018922194093, 0.9330127018922194093 ) ) 
 REPRESENTATION_ITEM ( '' )  );
#68121 = CARTESIAN_POINT ( 'NONE',  ( 16.71562500061451573, 3.027376345333611329, 5.243569643749999010 ) ) ;
#68122 = CARTESIAN_POINT ( 'NONE',  ( 12.29062500061451857, -3.027376345333614438, 5.243569643749998122 ) ) ;
#68123 = CARTESIAN_POINT ( 'NONE',  ( 25.02187500061451431, -5.492252693125287522, -1.008910452111647106E-15 ) ) ;
#68124 = CARTESIAN_POINT ( 'NONE',  ( 14.21249999999999858, 2.886751345948126879, 4.999999999999999112 ) ) ;
#68125 = CARTESIAN_POINT ( 'NONE',  ( 8.812500001229034652, 4.330127018922192761, -2.499999999999997780 ) ) ;
#68126 = CARTESIAN_POINT ( 'NONE',  ( 6.365625000614518747, 3.027376345333611329, 5.243569643749999010 ) ) ;
#68127 = CARTESIAN_POINT ( 'NONE',  ( 18.75000000122903288, 5.773502691896255534, 3.535250795749688894E-16 ) ) ;
#68128 = CARTESIAN_POINT ( 'NONE',  ( 27.59999999999999787, 4.330127018922192761, -2.499999999999997780 ) ) ;
#68129 = CARTESIAN_POINT ( 'NONE',  ( -2.121784821874999949, 11.23437500061451821, -33.67503911421598417 ) ) ;
#68130 = CARTESIAN_POINT ( 'NONE',  ( 1.592000809091587073E-14, 16.28750000000000142, -34.00000000000000000 ) ) ;
#68131 = CARTESIAN_POINT ( 'NONE',  ( 3.262500001229035718, -4.330127018922190985, -2.500000000000001332 ) ) ;
#68132 = EDGE_CURVE ( 'NONE', #68526, #42547, #46659, .T. ) ;
#68133 = AXIS2_PLACEMENT_3D ( 'NONE', #40013, #67370, #39655 ) ;
#68134 = CARTESIAN_POINT ( 'NONE',  ( -2.000000000000000000, 11.37500000000000178, -33.46410161513775705 ) ) ;
#68135 = CARTESIAN_POINT ( 'NONE',  ( 18.27187500061451431, -6.054752690667223547, -1.112240025338166033E-15 ) ) ;
#68136 = CARTESIAN_POINT ( 'NONE',  ( 6.487500001229034474, 6.123233995736764310E-16, -4.999999999999998224 ) ) ;
#68137 = CARTESIAN_POINT ( 'NONE',  ( 15.66562500061451857, 3.027376345333613106, -5.243569643749998122 ) ) ;
#68138 = CARTESIAN_POINT ( 'NONE',  ( 9.956250001229033586, -4.330127018922190985, -2.500000000000001332 ) ) ;
#68139 = CARTESIAN_POINT ( 'NONE',  ( 22.46250000122903501, 0.000000000000000000, 4.999999999999998224 ) ) ;
#68140 = CARTESIAN_POINT ( 'NONE',  ( 29.70937500061451431, 4.541064518000418104, -2.621784821874998173 ) ) ;
#68141 = CARTESIAN_POINT ( 'NONE',  ( 25.13437500061451502, 6.421520780324663323E-16, -5.243569643749999010 ) ) ;
#68142 = CARTESIAN_POINT ( 'NONE',  ( 18.42187500061451644, 4.119189519843966529, 2.378215178124999607 ) ) ;
#68143 = CARTESIAN_POINT ( 'NONE',  ( 12.77812500061451750, -4.541064518000419881, 2.621784821874995952 ) ) ;
#68144 = CARTESIAN_POINT ( 'NONE',  ( 11.74687500061451573, 6.054752690667223547, 3.707466751127219781E-16 ) ) ;
#68145 = ORIENTED_EDGE ( 'NONE', *, *, #31407, .T. ) ;
#68146 = CARTESIAN_POINT ( 'NONE',  ( 29.27812500061451573, 4.541064518000418104, 2.621784821874999949 ) ) ;
#68147 = CARTESIAN_POINT ( 'NONE',  ( 20.31562500061451715, 3.027376345333611329, 5.243569643749999010 ) ) ;
#68148 = CARTESIAN_POINT ( 'NONE',  ( 20.78732959644809952, 2.500000000000000000, -3.500000000000000000 ) ) ;
#68149 = CARTESIAN_POINT ( 'NONE',  ( 20.81249999999999645, 2.886751345948162850, -4.999999999999940492 ) ) ;
#68150 = EDGE_CURVE ( 'NONE', #32497, #46707, #36717, .T. ) ;
#68151 = CARTESIAN_POINT ( 'NONE',  ( 10.31250000000000355, -5.773502691896255534, -1.060575238724906372E-15 ) ) ;
#68152 = CARTESIAN_POINT ( 'NONE',  ( 21.15000000122903145, -2.886751345948129988, 4.999999999999997335 ) ) ;
#68153 = CARTESIAN_POINT ( 'NONE',  ( 16.41562500061451857, -6.054752690667223547, -1.112240025338166033E-15 ) ) ;
#68154 = CARTESIAN_POINT ( 'NONE',  ( 12.90937500061451537, 2.746126346562645981, -4.756430356249997438 ) ) ;
#68155 = ORIENTED_EDGE ( 'NONE', *, *, #60559, .T. ) ;
#68156 = CARTESIAN_POINT ( 'NONE',  ( 20.69999999999999929, -4.330127018922190985, -2.500000000000001332 ) ) ;
#68157 = CARTESIAN_POINT ( 'NONE',  ( 22.53750000000000142, -2.886751345948125991, -5.000000000000000000 ) ) ;
#68158 = CARTESIAN_POINT ( 'NONE',  ( 22.54687500061451999, 6.054752690667223547, 3.707466751127219781E-16 ) ) ;
#68159 = CARTESIAN_POINT ( 'NONE',  ( 24.59062500061451573, -3.027376345333610441, -5.243569643749999898 ) ) ;
#68160 = VERTEX_POINT ( 'NONE', #37753 ) ;
#68161 = CARTESIAN_POINT ( 'NONE',  ( 8.850000001229034297, 5.773502691896255534, 3.535250795749688401E-16 ) ) ;
#68162 = CARTESIAN_POINT ( 'NONE',  ( 8.428125000614517859, 6.421520780324663323E-16, -5.243569643749999010 ) ) ;
#68163 = CARTESIAN_POINT ( 'NONE',  ( 4.000000000000000000, 15.35000000122903252, 32.30940107675849760 ) ) ;
#68164 = CARTESIAN_POINT ( 'NONE',  ( 15.11249999999999893, 2.886751345948126879, 4.999999999999999112 ) ) ;
#68165 = CARTESIAN_POINT ( 'NONE',  ( -2.121784821874999949, 17.02812500061451573, 26.32496088578401938 ) ) ;
#68166 = CARTESIAN_POINT ( 'NONE',  ( 2.971875000614517592, -6.054752690667223547, -1.112240025338166033E-15 ) ) ;
#68167 = CARTESIAN_POINT ( 'NONE',  ( 26.67187500061451644, 3.027376345333611329, 5.243569643749999010 ) ) ;
#68168 = ORIENTED_EDGE ( 'NONE', *, *, #3964, .F. ) ;
#68169 = CARTESIAN_POINT ( 'NONE',  ( 24.32812500061451289, 4.541064518000418104, 2.621784821874999949 ) ) ;
#68170 = CARTESIAN_POINT ( 'NONE',  ( 26.25937500061451857, 0.000000000000000000, 5.243569643749999010 ) ) ;
#68171 = CARTESIAN_POINT ( 'NONE',  ( 4.243569643749999898, 18.19062500061459176, -27.54997392385601529 ) ) ;
#68172 = CARTESIAN_POINT ( 'NONE',  ( 11.43750000000000000, 5.773502691896255534, 3.535250795749688894E-16 ) ) ;
#68173 = CARTESIAN_POINT ( 'NONE',  ( 8.240625000614516082, -3.027376345333614438, 5.243569643749998122 ) ) ;
#68174 = CARTESIAN_POINT ( 'NONE',  ( 27.98437500061451289, 4.119189519843966529, 2.378215178124999607 ) ) ;
#68175 = CARTESIAN_POINT ( 'NONE',  ( 29.35312500061451502, 0.000000000000000000, 5.243569643749999010 ) ) ;
#68176 = CARTESIAN_POINT ( 'NONE',  ( 27.06562500061451715, 3.027376345333611329, 5.243569643749999010 ) ) ;
#68178 = EDGE_CURVE ( 'NONE', #17518, #16738, #51837, .T. ) ;
#68177 = CARTESIAN_POINT ( 'NONE',  ( 22.44375000122903785, -2.886751345948157965, 4.999999999999948486 ) ) ;
#68179 = CARTESIAN_POINT ( 'NONE',  ( 11.89687500061451608, -2.746126346562646425, 4.756430356249996549 ) ) ;
#68180 = CARTESIAN_POINT ( 'NONE',  ( 20.44687500061451857, -3.027376345333614438, 5.243569643749998122 ) ) ;
#68181 = CARTESIAN_POINT ( 'NONE',  ( -2.121784821874999949, 15.73437500061451644, 26.32496088578401938 ) ) ;
#68182 = CARTESIAN_POINT ( 'NONE',  ( 18.23437500061451999, -4.541064518000419881, 2.621784821874995952 ) ) ;
#68183 = CARTESIAN_POINT ( 'NONE',  ( 27.42187500061451644, 3.027376345333613106, -5.243569643749998122 ) ) ;
#68184 = CARTESIAN_POINT ( 'NONE',  ( 4.243569643749999010, 16.97187500061451715, 27.54997392385601174 ) ) ;
#68185 = CARTESIAN_POINT ( 'NONE',  ( 10.49062500061451431, -3.027376345333614438, 5.243569643749998122 ) ) ;
#68186 = CARTESIAN_POINT ( 'NONE',  ( 5.709375000614517859, -4.541064518000417216, -2.621784821875001281 ) ) ;
#68187 = CARTESIAN_POINT ( 'NONE',  ( 11.71875000122903465, -5.773502691896255534, -1.060575238724906372E-15 ) ) ;
#68188 = CARTESIAN_POINT ( 'NONE',  ( 8.653125000614515727, 0.000000000000000000, 5.243569643749999010 ) ) ;
#68189 = CARTESIAN_POINT ( 'NONE',  ( 11.48437500061451644, -4.541064518000419881, 2.621784821874995952 ) ) ;
#68190 = DIRECTION ( 'NONE',  ( 0.000000000000000000, 0.000000000000000000, 1.000000000000000000 ) ) ;
#68191 = CARTESIAN_POINT ( 'NONE',  ( 18.93750000122903288, -4.330127018922194537, 2.499999999999995559 ) ) ;
#68192 = CARTESIAN_POINT ( 'NONE',  ( 4.771875000614516971, -6.054752690667223547, -1.112240025338166033E-15 ) ) ;
#68193 = CARTESIAN_POINT ( 'NONE',  ( 8.165625000614516793, 3.027376345333611329, 5.243569643749999010 ) ) ;
#68194 = CARTESIAN_POINT ( 'NONE',  ( 5.465625000614517504, 3.027376345333611329, 5.243569643749999010 ) ) ;
#68195 = CARTESIAN_POINT ( 'NONE',  ( 23.34375000122903288, -2.886751345948129988, 4.999999999999997335 ) ) ;
#68196 = CARTESIAN_POINT ( 'NONE',  ( 19.58437500061451786, -4.541064518000419881, 2.621784821874995952 ) ) ;
#68197 = CARTESIAN_POINT ( 'NONE',  ( -1.071796769724491005, 11.47009619066136565, 26.00000000000000355 ) ) ;
#68198 = VERTEX_POINT ( 'NONE', #20384 ) ;
#68199 = CARTESIAN_POINT ( 'NONE',  ( 23.65312500061451573, -4.541064518000417216, -2.621784821875001281 ) ) ;
#68200 = CARTESIAN_POINT ( 'NONE',  ( 11.69062500061451360, 6.054752690667223547, 3.707466751127219781E-16 ) ) ;
#68201 = ADVANCED_FACE ( 'NONE', ( #32218 ), #42935, .T. ) ;
#68202 = AXIS2_PLACEMENT_3D ( 'NONE', #29739, #18993, #19733 ) ;
#68203 = CARTESIAN_POINT ( 'NONE',  ( 27.90937500061451715, 4.541064518000418104, -2.621784821874998173 ) ) ;
#68204 = CARTESIAN_POINT ( 'NONE',  ( 10.64062500061451644, -3.027376345333610441, -5.243569643749999898 ) ) ;
#68205 = CARTESIAN_POINT ( 'NONE',  ( 29.06249999999999289, 2.886751345948161962, 4.999999999999938716 ) ) ;
#68206 = CARTESIAN_POINT ( 'NONE',  ( 12.30000000122903181, -2.886751345948125991, -5.000000000000000000 ) ) ;
#68207 = CARTESIAN_POINT ( 'NONE',  ( 28.11562500061451431, -6.054752690667223547, -1.112240025338166033E-15 ) ) ;
#68208 = CARTESIAN_POINT ( 'NONE',  ( -3.000416591977282496E-16, 13.39062500061451644, -34.90005215228797653 ) ) ;
#68209 = CARTESIAN_POINT ( 'NONE',  ( 16.23750000122903359, -4.330127018922194537, 2.499999999999995559 ) ) ;
#68210 = CARTESIAN_POINT ( 'NONE',  ( 12.15000000000000036, -4.330127018922190985, -2.500000000000001332 ) ) ;
#68211 = CARTESIAN_POINT ( 'NONE',  ( 20.80312500061451431, 0.000000000000000000, 5.243569643749999010 ) ) ;
#68212 = CARTESIAN_POINT ( 'NONE',  ( 7.471875000614519813, -6.054752690667223547, -1.112240025338166033E-15 ) ) ;
#68213 = CARTESIAN_POINT ( 'NONE',  ( 8.700000001229032165, -2.886751345948125991, -5.000000000000000000 ) ) ;
#68214 = CARTESIAN_POINT ( 'NONE',  ( 15.67500000122903181, 2.886751345948126879, 4.999999999999999112 ) ) ;
#68215 = CARTESIAN_POINT ( 'NONE',  ( 13.71562500061451750, -6.054752690667223547, -1.112240025338166033E-15 ) ) ;
#68216 = CARTESIAN_POINT ( 'NONE',  ( 16.52812500061451573, 6.421520780324663323E-16, -5.243569643749999010 ) ) ;
#68217 = CARTESIAN_POINT ( 'NONE',  ( 25.50000000122903288, 5.773502691896255534, 3.535250795749688894E-16 ) ) ;
#68218 = CARTESIAN_POINT ( 'NONE',  ( 21.37499999999999645, 4.330127018922191873, 2.499999999999999556 ) ) ;
#68219 = CARTESIAN_POINT ( 'NONE',  ( 22.20937500061451431, 0.000000000000000000, 5.243569643749999010 ) ) ;
#68220 = CARTESIAN_POINT ( 'NONE',  ( 15.65625000122903465, 0.000000000000000000, 4.999999999999998224 ) ) ;
#68221 =( GEOMETRIC_REPRESENTATION_CONTEXT ( 3 ) GLOBAL_UNCERTAINTY_ASSIGNED_CONTEXT ( ( #1886 ) ) GLOBAL_UNIT_ASSIGNED_CONTEXT ( ( #37411, #59934, #27067 ) ) REPRESENTATION_CONTEXT ( 'NONE', 'WORKASPACE' ) );
#68222 = CARTESIAN_POINT ( 'NONE',  ( 10.95000000122903394, -2.886751345948125991, -5.000000000000000000 ) ) ;
#68223 = CARTESIAN_POINT ( 'NONE',  ( 8.221875000614518925, 3.027376345333611329, 5.243569643749999010 ) ) ;
#68224 = CARTESIAN_POINT ( 'NONE',  ( 27.30937500061451573, -4.541064518000417216, -2.621784821875001281 ) ) ;
#68225 = CARTESIAN_POINT ( 'NONE',  ( 4.196151849995945149, -2.718880220196457476, -4.196151849995952254 ) ) ;
#68226 = CARTESIAN_POINT ( 'NONE',  ( 24.51562500061451289, -6.054752690667223547, -1.112240025338166033E-15 ) ) ;
#68227 = CARTESIAN_POINT ( 'NONE',  ( -3.756430356250000102, 14.32812499938548356, 30.00000000000000000 ) ) ;
#68228 = CARTESIAN_POINT ( 'NONE',  ( 0.000000000000000000, 27.50000000000000000, 26.00000000000000000 ) ) ;
#68229 = CARTESIAN_POINT ( 'NONE',  ( 7.921875000614517326, -6.054752690667223547, -1.112240025338166033E-15 ) ) ;
#68230 = CARTESIAN_POINT ( 'NONE',  ( 28.07812500061451289, -4.541064518000419881, 2.621784821874995952 ) ) ;
#68231 = CARTESIAN_POINT ( 'NONE',  ( 6.234375000614519102, 6.421520780324663323E-16, -5.243569643749999010 ) ) ;
#68232 = CARTESIAN_POINT ( 'NONE',  ( -3.999999999999997335, 16.55000000122903359, -27.69059892324149530 ) ) ;
#68233 = CARTESIAN_POINT ( 'NONE',  ( 25.95937500061451431, -4.541064518000417216, -2.621784821875001281 ) ) ;
#68234 = CARTESIAN_POINT ( 'NONE',  ( -2.121784821874999949, 10.72812500061459318, 26.32496088578401938 ) ) ;
#68235 = CARTESIAN_POINT ( 'NONE',  ( 20.36249999999999716, 2.886751345948129099, -4.999999999999998224 ) ) ;
#68236 = ORIENTED_EDGE ( 'NONE', *, *, #34637, .F. ) ;
#68237 = CARTESIAN_POINT ( 'NONE',  ( 26.69999999999999929, 4.330127018922192761, -2.499999999999997780 ) ) ;
#68238 =( BOUNDED_SURFACE ( )  B_SPLINE_SURFACE ( 1, 2, ( 
 ( #28415, #39880, #67232, #16591, #57926, #30229, #63833, #36860, #70483, #35763, #2518, #35400, #2164, #1444, #13225, #14324, #52761, #52399, #25039, #13958, #36495, #23948, #47583, #58652, #46498, #6973, #1807, #7333, #36133, #64933, #8059, #24315, #53489, #64199, #70112, #41676, #47222, #29504, #52039, #8418, #29863, #69036, #69753, #46864, #30593, #18398, #24675, #64569, #40965, #12868, #19488, #42046, #19122, #13586, #25411, #63481, #19860, #2881, #69403, #53120, #59015, #30952, #47956, #18759, #42413, #41323, #58285, #7691, #9883, #66034, #10253, #43876, #43140, #43510, #48684, #37591, #15413, #59748, #21689, #37955, #31690, #71208, #3622, #54225, #60112, #49055, #4360, #3990, #60475, #20219, #38320, #26517, #70846, #32418, #4715, #59376, #54955, #48321, #42774, #32784, #16148, #66402, #3255, #71947, #55321, #21323, #26888, #44245, #65664, #71583, #60846, #49415, #37224, #15778, #20956, #27249, #49783, #65293, #14682, #72307, #20585, #9155, #66776, #8786, #15053, #31321, #53864, #25784, #9522, #26144, #32055, #54588, #55681, #67502, #28327, #5797, #50865, #993, #38700, #263, #45692, #68226, #17589, #44616, #44964, #12061, #34220, #56753, #61942, #5438, #23500, #22058, #51593, #27611, #27977, #50147, #67146, #72675, #39791, #16506, #39059, #34584, #68583, #23137, #5078, #51226, #62666, #630, #6158, #46048, #22417, #56406, #40148, #28687, #61573, #22772, #45324, #57112, #6524, #10976, #33497, #67860, #50508, #56046, #29056, #17231, #16866, #61220, #62308, #11704, #11346, #10614, #33143, #73034, #39421, #33863, #7596, #58193, #30135, #53395, #17944, #52666, #24945, #47489, #70019, #23859, #24222, #64471, #13488, #36036, #41230, #57833, #2788, #1350, #30857, #6884, #7242, #29417, #46407, #51950, #69661, #35311, #13865, #2073, #58556, #24582, #47130, #25313, #47859, #19390, #68944, #40506, #19026, #18302, #41585, #63021, #63742, #2422, #57480, #40873, #7964, #30500, #64103, #13131, #36406, #12420, #8327, #58919, #63390, #53028, #41951, #34952, #35670, #29771, #12775, #52307, #1709, #46771, #69307, #18668, #21230, #54860, #54135, #54497, #59655, #48592, #3898, #70749, #32696, #26419, #42679, #9064, #14591, #65202, #71117, #60019, #15322, #14961, #71490, #31224, #49326, #37499, #8692, #43420, #15686, #70388, #20867, #53766, #71858, #9431, #3161, #65942, #38224, #19764, #37863, #59283, #25690, #43782, #27158, #4268, #14228, #9790, #66309, #32323, #60382, #55233, #3530, #31959, #60754, #26792, #48225, #48960, #10162, #4628, #42315, #20124, #37126, #64841, #31598, #26052, #36766, #20489, #43045, #65571, #33778, #11256, #72947, #57024, #5710, #56321, #66681, #5349, #39336, #16778, #61849, #11973, #49692, #28246, #56671, #6069, #28602, #55592, #55953, #23048, #45236, #67769, #22329, #16416, #34496, #33053, #62576, #38604, #38972, #61130, #4987, #10525, #50777, #67057, #45604, #180, #17144, #22685, #39702, #6430, #72220, #51138, #27519, #21598, #62220, #50053, #11616, #44152, #44881, #34133, #16056, #72582, #537, #68137, #17501, #67416, #40062, #21966, #44524, #61488, #10885, #33414, #27888, #50421, #46683, #46320, #47043, #7879, #23411, #18939, #52582, #35585, #52943, #13397, #12689, #13046, #18212, #7154, #58104, #29329, #64387, #7511, #1261, #40784, #68855, #23768, #29684, #18582, #69577, #69221, #30042, #62932, #63297, #41147, #63655, #57388, #35226, #51859, #36319, #30415, #13777, #58834, #2340, #64019, #57747, #19304, #52221, #1988, #28965, #51503, #45958, #24499, #1625, #24133, #41857, #41498, #40415, #34861, #6795, #24857, #35945, #58466, #903, #47403, #69934, #12325, #68491, #17855, #59198, #70662, #26334, #20777, #8607, #31512, #65118, #38139, #71775, #37042, #3813, #36678, #3448, #2704, #14509, #15597, #54053, #53677, #48873, #15238, #37775, #25220, #71403, #59938, #47766, #8244, #3071, #31136, #37415, #66219, #14143, #20409, #25600, #48138, #70302, #20038, #30774, #42593, #43334, #65856, #4178, #59566, #60295, #19675, #9705, #42957, #71034, #25966, #8979, #32240, #48507, #53304, #42228, #65486, #14876, #64753, #26707, #9345, #54773, #31878, #49241, #54412, #21144, #43698, #44063, #21876, #27436, #38517, #27072, #67332, #27802, #33333, #67684, #10076, #50338, #4543, #56235, #49603, #5258, #45517, #68048, #72491, #22600, #50692, #60663, #61403, #44799, #72130, #55508, #21509, #448, #66589, #49967, #15967, #61040, #10438, #39249, #4901, #34047, #16692, #5628, #22245, #72862, #17417, #32607, #62133, #32968, #55145, #61762, #44437, #11166, #66966, #55871, #45152, #16331, #38886, #28165, #94, #33690, #10798, #5983, #17055, #51051, #56587, #39614, #11526, #28513, #22957, #57664, #57305, #58019, #18856, #34411, #29955, #63575, #46595, #63933, #24411, #23683, #24048, #29243, #18127, #69137, #40327, #2259, #18496, #12242, #51775, #6710, #34773, #40693, #29599, #7428, #7070, #41061, #815, #41417, #52135, #51413, #12962, #58380, #39976, #35499, #28874, #23323, #13318, #69850, #46960, #56938, #52496, #35857, #1906, #69496, #24773, #46231, #1538, #7792, #30329, #17767, #52859, #47317, #62488, #11886, #45872, #68405, #6343, #1175, #62848, #68771, #63211, #12607, #35141, #3362, #53964, #42508, #26618, #48423, #25883, #36233, #48055, #8892, #59480, #31424, #54687, #19217, #70949, #26249, #48786, #71311, #25135, #25510, #65767, #14788, #37329, #65032, #59114, #4088, #2614, #20320, #20688, #43247, #15149, #47676, #70580, #37686, #59853, #9257, #14423, #8521, #49155, #70212, #32154, #8157, #31050, #30686, #19586, #53217, #42874, #36593, #60209, #65396, #31792, #54330, #3724, #41771, #64300, #9621, #42142, #13689, #58747, #64669, #14053, #53587, #36958, #2982, #19956, #4457, #16602, #11072, #61315, #21783, #16964, #71686, #62046, #67599, #55056, #5173, #67244, #33244 ),
 ( #28426, #66496, #72041, #27708, #56500, #26987, #10712, #49516, #43976, #60576, #38424, #21058, #15879, #39158, #61673, #39519, #21419, #33599, #9982, #56144, #55782, #50249, #44350, #60947, #5538, #10350, #5893, #15509, #72772, #66875, #43609, #11441, #32880, #28076, #55420, #50604, #4813, #72402, #44708, #27346, #49877, #16243, #38799, #38050, #22156, #8, #22515, #45062, #66131, #33961, #32519, #46508, #17331, #68686, #36779, #59295, #57936, #7343, #67958, #69046, #29515, #39890, #8705, #45788, #51325, #6984, #50963, #56851, #63125, #6257, #23237, #62403, #17683, #359, #68323, #18409, #40975, #47874, #728, #63490, #11802, #35411, #12521, #40604, #23601, #40244, #12878, #62764, #22866, #34319, #35054, #46146, #45424, #70402, #28785, #29873, #12156, #53409, #34684, #51689, #23960, #57214, #6628, #29157, #1093, #18046, #57581, #52050, #1454, #2801, #25328, #19778, #42328, #64853, #14241, #48975, #16069, #38619, #43060, #66323, #21244, #31238, #31973, #15336, #20138, #26066, #42693, #37876, #65215, #65585, #71504, #65956, #59669, #14975, #54149, #61143, #10175, #66697, #53779, #32710, #15700, #60034, #21612, #31613, #60396, #3175, #25702, #48238, #20880, #54509, #9445, #44167, #26434, #14605, #37142, #9077, #55247, #9804, #32337, #70763, #4642, #3543, #48605, #27172, #71130, #20503, #37513, #49340, #43798, #3912, #43434, #54875, #4280, #26806, #71872, #38239, #60768, #49706, #72234, #16793, #17869, #56335, #55969, #6083, #45251, #194, #5725, #10898, #23063, #33426, #68506, #27535, #22699, #28260, #40428, #28980, #38986, #28615, #67070, #553, #67431, #11271, #56684, #16428, #44895, #50436, #61501, #50067, #17158, #50791, #67784, #17515, #39717, #62235, #5363, #11631, #34147, #51152, #45972, #10538, #45618, #40076, #62591, #11987, #27901, #39350, #57039, #68152, #34510, #33792, #72961, #33066, #22343, #23426, #72597, #61864, #21980, #6445, #44539, #51518, #917, #55605, #5001, #7892, #24513, #30058, #47779, #70314, #64400, #18224, #12339, #52596, #40798, #18953, #62945, #35598, #47417, #29342, #68868, #30428, #2353, #2003, #13059, #8257, #34874, #53318, #58847, #46334, #69591, #58481, #47057, #7525, #7169, #52956, #41871, #57403, #24870, #13411, #41513, #13793, #69947, #46698, #64032, #52235, #41160, #35960, #63311, #25233, #19317, #35239, #1639, #29697, #57760, #63669, #36333, #30787, #2717, #19688, #23782, #6808, #51874, #1273, #12702, #24145, #69234, #18596, #58117, #53689, #15609, #72141, #26719, #59211, #36689, #32251, #65869, #48884, #66230, #49253, #25979, #26345, #31524, #20420, #71414, #42604, #4554, #20790, #14520, #54063, #59578, #37053, #42968, #31889, #60307, #59949, #43347, #3083, #21156, #9356, #25612, #15250, #60674, #42241, #37787, #31148, #48149, #38151, #64765, #71787, #8619, #54784, #10088, #4190, #9718, #27083, #48518, #54424, #43709, #32618, #20049, #55158, #3824, #49615, #14155, #70674, #65130, #8991, #3459, #71045, #65498, #14887, #37427, #22611, #16704, #67343, #27815, #22968, #61774, #50349, #11177, #55519, #44810, #22256, #39261, #51063, #21520, #33701, #17067, #39626, #62144, #4913, #33345, #56598, #28176, #50703, #72874, #16342, #45530, #27448, #460, #10450, #38897, #32979, #49978, #72502, #56248, #66978, #5994, #5640, #106, #45163, #67694, #44075, #66604, #28524, #21891, #38528, #11539, #44448, #34058, #15978, #61051, #61416, #10809, #55882, #5270, #49051, #44241, #49779, #37586, #5073, #71578, #32050, #43505, #72303, #66771, #54582, #4356, #37951, #10970, #26882, #3986, #16144, #26511, #39055, #71204, #43872, #49411, #61568, #72672, #9518, #21684, #60108, #38696, #60469, #54950, #27242, #20952, #15408, #66030, #9878, #20580, #60842, #21319, #71942, #61215, #27608, #48680, #10610, #54221, #43135, #66397, #3618, #26139, #32413, #33139, #55676, #65659, #15773, #38315, #15048, #10247, #32780, #55317, #4711, #50143, #22052, #44612, #67142, #16501, #56403, #40869, #12416, #68940, #63386, #34948, #68579, #62305, #23855, #33860, #68222, #33493, #18298, #50503, #626, #34216, #11700, #46402, #28684, #44961, #39417, #11342, #57475, #17584, #260, #28324, #23496, #29052, #16862, #6880, #50862, #5793, #22769, #51588, #46044, #45321, #56750, #17228, #56042, #5434, #6154, #988, #61939, #51223, #27973, #39788, #73030, #23132, #67855, #17939, #40502, #63017, #22414, #29413, #12057, #67499, #45688, #40144, #62660, #34580, #57108, #6519, #51946, #1344, #58188, #1703, #52662, #42675, #30130, #53388, #2784, #8687, #35666, #25308, #24218, #70384, #47484, #2418, #70015, #30496, #47855, #19760, #46767, #69302, #19385, #2069, #18664, #42310, #24940, #41581, #64837, #41945, #64467, #36032, #20121, #13860, #58550, #36402, #41225, #58914, #53024, #8323, #48220, #12771, #30853, #14224, #36760, #59279, #63736, #19021, #31219, #53762, #3157, #7960, #24578, #70744, #13127, #25686, #7592, #47124, #69656, #64098, #13483, #35306, #57829, #7238, #29766, #52302, #26787, #32320, #50049, #72576, #66676, #20485, #14587, #54855, #43040, #21225, #65198, #37857, #49687, #31592, #71113, #10158, #9786, #54131, #65567, #44148, #37121, #55588, #61126, #48587, #71853, #60748, #49322, #4264, #9427, #32691, #16051, #59650, #55229, #15682, #43778, #38599, #72216, #48955, #66305, #54493, #43414, #38220, #14956, #27515, #4624, #37495, #3894, #31955, #60015, #65938, #27153, #21594, #10521, #33049, #26047, #4983, #21962, #3526, #9060, #26413, #71486, #20863, #15318, #60378, #17848, #1256, #28960, #61484, #57021, #68484, #6426, #11968, #29324, #28242, #62216, #45953, #40057, #22324, #11611, #45600, #5345, #23405, #34129, #55949, #17497, #62927, #44519, #68131, #33411, #27883, #40410, #67053, #51498, #10879, #898, #12321, #34856, #34492, #51853, #50773, #56669, #57383, #62572, #44877 ) ),
 .UNSPECIFIED., .F., .F., .F. ) 
 B_SPLINE_SURFACE_WITH_KNOTS ( ( 2, 2 ),
 ( 3, 2, 2, 2, 2, 2, 2, 2, 2, 2, 2, 2, 2, 2, 2, 2, 2, 2, 2, 2, 2, 2, 2, 2, 2, 2, 2, 2, 2, 2, 2, 2, 2, 2, 2, 2, 2, 2, 2, 2, 2, 2, 2, 2, 2, 2, 2, 2, 2, 2, 2, 2, 2, 2, 2, 2, 2, 2, 2, 2, 2, 2, 2, 2, 2, 2, 2, 2, 2, 2, 2, 2, 2, 2, 2, 2, 2, 2, 2, 2, 2, 2, 2, 2, 2, 2, 2, 2, 2, 2, 2, 2, 2, 2, 2, 2, 2, 2, 2, 2, 2, 2, 2, 2, 2, 2, 2, 2, 2, 2, 2, 2, 2, 2, 2, 2, 2, 2, 2, 2, 2, 2, 2, 2, 2, 2, 2, 2, 2, 2, 2, 2, 2, 2, 2, 2, 2, 2, 2, 2, 2, 2, 2, 2, 2, 2, 2, 2, 2, 2, 2, 2, 2, 2, 2, 2, 2, 2, 2, 2, 2, 2, 2, 2, 2, 2, 2, 2, 2, 2, 2, 2, 2, 2, 2, 2, 2, 2, 2, 2, 2, 2, 2, 2, 2, 2, 2, 2, 2, 2, 2, 2, 2, 2, 2, 2, 2, 2, 2, 2, 2, 2, 2, 2, 2, 2, 2, 2, 2, 2, 2, 2, 2, 2, 2, 2, 2, 2, 2, 2, 2, 2, 2, 2, 2, 2, 2, 2, 2, 2, 2, 2, 2, 2, 2, 2, 2, 2, 2, 2, 2, 2, 2, 2, 2, 2, 2, 2, 2, 2, 2, 2, 2, 2, 2, 2, 2, 2, 2, 2, 2, 2, 2, 2, 2, 2, 2, 2, 2, 2, 2, 2, 2, 2, 2, 2, 2, 2, 2, 2, 2, 2, 2, 2, 2, 2, 2, 2, 2, 2, 2, 2, 2, 2, 2, 2, 2, 2, 2, 2, 2, 2, 2, 2, 2, 2, 2, 2, 2, 2, 2, 2, 2, 2, 2, 2, 2, 2, 2, 2, 2, 2, 2, 2, 2, 2, 2, 2, 2, 2, 2, 2, 2, 2, 2, 2, 2, 2, 2, 2, 2, 2, 2, 2, 2, 2, 2, 2, 2, 2, 2, 2, 2, 2, 2, 2, 2, 2, 2, 2, 3 ),
 ( 0.000000000000000000, 1.000000000000000000 ),
 ( 0.000000000000000000, 0.002777777777777777884, 0.005555555555555555768, 0.008333333333333333218, 0.01111111111111111154, 0.01388888888888888812, 0.01666666666666666644, 0.01944444444444444475, 0.02222222222222222307, 0.02500000000000000139, 0.02777777777777777624, 0.03055555555555555455, 0.03333333333333333287, 0.03611111111111110772, 0.03888888888888888951, 0.04166666666666666435, 0.04444444444444444614, 0.04722222222222222099, 0.05000000000000000278, 0.05277777777777777762, 0.05555555555555555247, 0.05833333333333333426, 0.06111111111111110911, 0.06388888888888888395, 0.06666666666666666574, 0.06944444444444444753, 0.07222222222222221544, 0.07499999999999999722, 0.07777777777777777901, 0.08055555555555556080, 0.08333333333333332871, 0.08611111111111111049, 0.08888888888888889228, 0.09166666666666666019, 0.09444444444444444198, 0.09722222222222222376, 0.1000000000000000056, 0.1027777777777777735, 0.1055555555555555552, 0.1083333333333333370, 0.1111111111111111049, 0.1138888888888888867, 0.1166666666666666685, 0.1194444444444444503, 0.1222222222222222182, 0.1250000000000000000, 0.1277777777777777679, 0.1305555555555555636, 0.1333333333333333315, 0.1361111111111110994, 0.1388888888888888951, 0.1416666666666666630, 0.1444444444444444309, 0.1472222222222222265, 0.1499999999999999944, 0.1527777777777777901, 0.1555555555555555580, 0.1583333333333333259, 0.1611111111111111216, 0.1638888888888888895, 0.1666666666666666574, 0.1694444444444444531, 0.1722222222222222210, 0.1749999999999999889, 0.1777777777777777846, 0.1805555555555555525, 0.1833333333333333204, 0.1861111111111111160, 0.1888888888888888840, 0.1916666666666666796, 0.1944444444444444475, 0.1972222222222222154, 0.2000000000000000111, 0.2027777777777777790, 0.2055555555555555469, 0.2083333333333333426, 0.2111111111111111105, 0.2138888888888888784, 0.2166666666666666741, 0.2194444444444444420, 0.2222222222222222099, 0.2250000000000000056, 0.2277777777777777735, 0.2305555555555555691, 0.2333333333333333370, 0.2361111111111111049, 0.2388888888888889006, 0.2416666666666666685, 0.2444444444444444364, 0.2472222222222222321, 0.2500000000000000000, 0.2527777777777777679, 0.2555555555555555358, 0.2583333333333333592, 0.2611111111111111271, 0.2638888888888888951, 0.2666666666666666630, 0.2694444444444444309, 0.2722222222222221988, 0.2750000000000000222, 0.2777777777777777901, 0.2805555555555555580, 0.2833333333333333259, 0.2861111111111110938, 0.2888888888888888618, 0.2916666666666666852, 0.2944444444444444531, 0.2972222222222222210, 0.2999999999999999889, 0.3027777777777777568, 0.3055555555555555802, 0.3083333333333333481, 0.3111111111111111160, 0.3138888888888888840, 0.3166666666666666519, 0.3194444444444444198, 0.3222222222222222432, 0.3250000000000000111, 0.3277777777777777790, 0.3305555555555555469, 0.3333333333333333148, 0.3361111111111111382, 0.3388888888888889062, 0.3416666666666666741, 0.3444444444444444420, 0.3472222222222222099, 0.3499999999999999778, 0.3527777777777778012, 0.3555555555555555691, 0.3583333333333333370, 0.3611111111111111049, 0.3638888888888888729, 0.3666666666666666408, 0.3694444444444444642, 0.3722222222222222321, 0.3750000000000000000, 0.3777777777777777679, 0.3805555555555555358, 0.3833333333333333592, 0.3861111111111111271, 0.3888888888888888951, 0.3916666666666666630, 0.3944444444444444309, 0.3972222222222221988, 0.4000000000000000222, 0.4027777777777777901, 0.4055555555555555580, 0.4083333333333333259, 0.4111111111111110938, 0.4138888888888888618, 0.4166666666666666852, 0.4194444444444444531, 0.4222222222222222210, 0.4249999999999999889, 0.4277777777777777568, 0.4305555555555555802, 0.4333333333333333481, 0.4361111111111111160, 0.4388888888888888840, 0.4416666666666666519, 0.4444444444444444198, 0.4472222222222222432, 0.4500000000000000111, 0.4527777777777777790, 0.4555555555555555469, 0.4583333333333333148, 0.4611111111111111382, 0.4638888888888889062, 0.4666666666666666741, 0.4694444444444444420, 0.4722222222222222099, 0.4749999999999999778, 0.4777777777777778012, 0.4805555555555555691, 0.4833333333333333370, 0.4861111111111111049, 0.4888888888888888729, 0.4916666666666666408, 0.4944444444444444642, 0.4972222222222222321, 0.5000000000000000000, 0.5027777777777777679, 0.5055555555555555358, 0.5083333333333333037, 0.5111111111111110716, 0.5138888888888888395, 0.5166666666666667185, 0.5194444444444444864, 0.5222222222222222543, 0.5250000000000000222, 0.5277777777777777901, 0.5305555555555555580, 0.5333333333333333259, 0.5361111111111110938, 0.5388888888888888618, 0.5416666666666666297, 0.5444444444444443976, 0.5472222222222222765, 0.5500000000000000444, 0.5527777777777778123, 0.5555555555555555802, 0.5583333333333333481, 0.5611111111111111160, 0.5638888888888888840, 0.5666666666666666519, 0.5694444444444444198, 0.5722222222222221877, 0.5749999999999999556, 0.5777777777777777235, 0.5805555555555556024, 0.5833333333333333703, 0.5861111111111111382, 0.5888888888888889062, 0.5916666666666666741, 0.5944444444444444420, 0.5972222222222222099, 0.5999999999999999778, 0.6027777777777777457, 0.6055555555555555136, 0.6083333333333332815, 0.6111111111111111605, 0.6138888888888889284, 0.6166666666666666963, 0.6194444444444444642, 0.6222222222222222321, 0.6250000000000000000, 0.6277777777777777679, 0.6305555555555555358, 0.6333333333333333037, 0.6361111111111110716, 0.6388888888888888395, 0.6416666666666667185, 0.6444444444444444864, 0.6472222222222222543, 0.6500000000000000222, 0.6527777777777777901, 0.6555555555555555580, 0.6583333333333333259, 0.6611111111111110938, 0.6638888888888888618, 0.6666666666666666297, 0.6694444444444443976, 0.6722222222222222765, 0.6750000000000000444, 0.6777777777777778123, 0.6805555555555555802, 0.6833333333333333481, 0.6861111111111111160, 0.6888888888888888840, 0.6916666666666666519, 0.6944444444444444198, 0.6972222222222221877, 0.6999999999999999556, 0.7027777777777777235, 0.7055555555555556024, 0.7083333333333333703, 0.7111111111111111382, 0.7138888888888889062, 0.7166666666666666741, 0.7194444444444444420, 0.7222222222222222099, 0.7249999999999999778, 0.7277777777777777457, 0.7305555555555555136, 0.7333333333333332815, 0.7361111111111111605, 0.7388888888888889284, 0.7416666666666666963, 0.7444444444444444642, 0.7472222222222222321, 0.7500000000000000000, 0.7527777777777777679, 0.7555555555555555358, 0.7583333333333333037, 0.7611111111111110716, 0.7638888888888888395, 0.7666666666666667185, 0.7694444444444444864, 0.7722222222222222543, 0.7750000000000000222, 0.7777777777777777901, 0.7805555555555555580, 0.7833333333333333259, 0.7861111111111110938, 0.7888888888888888618, 0.7916666666666666297, 0.7944444444444443976, 0.7972222222222222765, 0.8000000000000000444, 0.8027777777777778123, 0.8055555555555555802, 0.8083333333333333481, 0.8111111111111111160, 0.8138888888888888840, 0.8166666666666666519, 0.8194444444444444198, 0.8222222222222221877, 0.8249999999999999556, 0.8277777777777777235, 0.8305555555555556024, 0.8333333333333333703, 0.8361111111111111382, 0.8388888888888889062, 0.8416666666666666741, 0.8444444444444444420, 0.8472222222222222099, 0.8499999999999999778, 0.8527777777777777457, 0.8555555555555555136, 0.8583333333333332815, 0.8611111111111111605, 0.8638888888888889284, 0.8666666666666666963, 0.8694444444444444642, 0.8722222222222222321, 0.8750000000000000000, 0.8777777777777777679, 0.8805555555555555358, 0.8833333333333333037, 0.8861111111111110716, 0.8888888888888888395, 0.8916666666666667185, 0.8944444444444444864, 0.8972222222222222543, 0.9000000000000000222, 0.9027777777777777901, 0.9055555555555555580, 0.9083333333333333259, 0.9111111111111110938, 0.9138888888888888618, 0.9166666666666666297, 0.9194444444444443976, 0.9222222222222222765, 0.9250000000000000444, 0.9277777777777778123, 0.9305555555555555802, 0.9333333333333333481, 0.9361111111111111160, 0.9388888888888888840, 0.9416666666666666519, 0.9444444444444444198, 0.9472222222222221877, 0.9499999999999999556, 0.9527777777777777235, 0.9555555555555556024, 0.9583333333333333703, 0.9611111111111111382, 0.9638888888888889062, 0.9666666666666666741, 0.9694444444444444420, 0.9722222222222222099, 0.9749999999999999778, 0.9777777777777777457, 0.9805555555555555136, 0.9833333333333332815, 0.9861111111111111605, 0.9888888888888889284, 0.9916666666666666963, 0.9944444444444444642, 0.9972222222222222321, 1.000000000000000000 ),
 .UNSPECIFIED. ) 
 GEOMETRIC_REPRESENTATION_ITEM ( )  RATIONAL_B_SPLINE_SURFACE ( (
 ( 1.000000000000000000, 0.8660254037844387076, 1.000000000000000000, 0.8660254037844387076, 1.000000000000000000, 0.8660254037844387076, 1.000000000000000000, 0.8660254037844387076, 1.000000000000000000, 0.8660254037844387076, 1.000000000000000000, 0.8660254037844387076, 1.000000000000000000, 0.8660254037844387076, 1.000000000000000000, 0.8660254037844387076, 1.000000000000000000, 0.8660254037844387076, 1.000000000000000000, 0.8660254037844387076, 1.000000000000000000, 0.8660254037844387076, 1.000000000000000000, 0.8660254037844387076, 1.000000000000000000, 0.8660254037844387076, 1.000000000000000000, 0.8660254037844387076, 1.000000000000000000, 0.8660254037844387076, 1.000000000000000000, 0.8660254037844387076, 1.000000000000000000, 0.8660254037844387076, 1.000000000000000000, 0.8660254037844387076, 1.000000000000000000, 0.8660254037844387076, 1.000000000000000000, 0.8660254037844387076, 1.000000000000000000, 0.8660254037844387076, 1.000000000000000000, 0.8660254037844387076, 1.000000000000000000, 0.8660254037844387076, 1.000000000000000000, 0.8660254037844387076, 1.000000000000000000, 0.8660254037844387076, 1.000000000000000000, 0.8660254037844387076, 1.000000000000000000, 0.8660254037844387076, 1.000000000000000000, 0.8660254037844387076, 1.000000000000000000, 0.8660254037844387076, 1.000000000000000000, 0.8660254037844387076, 1.000000000000000000, 0.8660254037844387076, 1.000000000000000000, 0.8660254037844387076, 1.000000000000000000, 0.8660254037844387076, 1.000000000000000000, 0.8660254037844387076, 1.000000000000000000, 0.8660254037844387076, 1.000000000000000000, 0.8660254037844387076, 1.000000000000000000, 0.8660254037844387076, 1.000000000000000000, 0.8660254037844387076, 1.000000000000000000, 0.8660254037844387076, 1.000000000000000000, 0.8660254037844387076, 1.000000000000000000, 0.8660254037844387076, 1.000000000000000000, 0.8660254037844387076, 1.000000000000000000, 0.8660254037844387076, 1.000000000000000000, 0.8660254037844387076, 1.000000000000000000, 0.8660254037844387076, 1.000000000000000000, 0.8660254037844387076, 1.000000000000000000, 0.8660254037844387076, 1.000000000000000000, 0.8660254037844387076, 1.000000000000000000, 0.8660254037844387076, 1.000000000000000000, 0.8660254037844387076, 1.000000000000000000, 0.8660254037844387076, 1.000000000000000000, 0.8660254037844387076, 1.000000000000000000, 0.8660254037844387076, 1.000000000000000000, 0.8660254037844387076, 1.000000000000000000, 0.8660254037844387076, 1.000000000000000000, 0.8660254037844387076, 1.000000000000000000, 0.8660254037844387076, 1.000000000000000000, 0.8660254037844387076, 1.000000000000000000, 0.8660254037844387076, 1.000000000000000000, 0.8660254037844387076, 1.000000000000000000, 0.8660254037844387076, 1.000000000000000000, 0.8660254037844387076, 1.000000000000000000, 0.8660254037844387076, 1.000000000000000000, 0.8660254037844387076, 1.000000000000000000, 0.8660254037844387076, 1.000000000000000000, 0.8660254037844387076, 1.000000000000000000, 0.8660254037844387076, 1.000000000000000000, 0.8660254037844387076, 1.000000000000000000, 0.8660254037844387076, 1.000000000000000000, 0.8660254037844387076, 1.000000000000000000, 0.8660254037844387076, 1.000000000000000000, 0.8660254037844387076, 1.000000000000000000, 0.8660254037844387076, 1.000000000000000000, 0.8660254037844387076, 1.000000000000000000, 0.8660254037844387076, 1.000000000000000000, 0.8660254037844387076, 1.000000000000000000, 0.8660254037844387076, 1.000000000000000000, 0.8660254037844387076, 1.000000000000000000, 0.8660254037844387076, 1.000000000000000000, 0.8660254037844387076, 1.000000000000000000, 0.8660254037844387076, 1.000000000000000000, 0.8660254037844387076, 1.000000000000000000, 0.8660254037844387076, 1.000000000000000000, 0.8660254037844387076, 1.000000000000000000, 0.8660254037844387076, 1.000000000000000000, 0.8660254037844387076, 1.000000000000000000, 0.8660254037844387076, 1.000000000000000000, 0.8660254037844387076, 1.000000000000000000, 0.8660254037844387076, 1.000000000000000000, 0.8660254037844387076, 1.000000000000000000, 0.8660254037844387076, 1.000000000000000000, 0.8660254037844387076, 1.000000000000000000, 0.8660254037844387076, 1.000000000000000000, 0.8660254037844387076, 1.000000000000000000, 0.8660254037844387076, 1.000000000000000000, 0.8660254037844387076, 1.000000000000000000, 0.8660254037844387076, 1.000000000000000000, 0.8660254037844387076, 1.000000000000000000, 0.8660254037844387076, 1.000000000000000000, 0.8660254037844387076, 1.000000000000000000, 0.8660254037844387076, 1.000000000000000000, 0.8660254037844387076, 1.000000000000000000, 0.8660254037844387076, 1.000000000000000000, 0.8660254037844387076, 1.000000000000000000, 0.8660254037844387076, 1.000000000000000000, 0.8660254037844387076, 1.000000000000000000, 0.8660254037844387076, 1.000000000000000000, 0.8660254037844387076, 1.000000000000000000, 0.8660254037844387076, 1.000000000000000000, 0.8660254037844387076, 1.000000000000000000, 0.8660254037844387076, 1.000000000000000000, 0.8660254037844387076, 1.000000000000000000, 0.8660254037844387076, 1.000000000000000000, 0.8660254037844387076, 1.000000000000000000, 0.8660254037844387076, 1.000000000000000000, 0.8660254037844387076, 1.000000000000000000, 0.8660254037844387076, 1.000000000000000000, 0.8660254037844387076, 1.000000000000000000, 0.8660254037844387076, 1.000000000000000000, 0.8660254037844387076, 1.000000000000000000, 0.8660254037844387076, 1.000000000000000000, 0.8660254037844387076, 1.000000000000000000, 0.8660254037844387076, 1.000000000000000000, 0.8660254037844387076, 1.000000000000000000, 0.8660254037844387076, 1.000000000000000000, 0.8660254037844387076, 1.000000000000000000, 0.8660254037844387076, 1.000000000000000000, 0.8660254037844387076, 1.000000000000000000, 0.8660254037844387076, 1.000000000000000000, 0.8660254037844387076, 1.000000000000000000, 0.8660254037844387076, 1.000000000000000000, 0.8660254037844387076, 1.000000000000000000, 0.8660254037844387076, 1.000000000000000000, 0.8660254037844387076, 1.000000000000000000, 0.8660254037844387076, 1.000000000000000000, 0.8660254037844387076, 1.000000000000000000, 0.8660254037844387076, 1.000000000000000000, 0.8660254037844387076, 1.000000000000000000, 0.8660254037844387076, 1.000000000000000000, 0.8660254037844387076, 1.000000000000000000, 0.8660254037844387076, 1.000000000000000000, 0.8660254037844387076, 1.000000000000000000, 0.8660254037844387076, 1.000000000000000000, 0.8660254037844387076, 1.000000000000000000, 0.8660254037844387076, 1.000000000000000000, 0.8660254037844387076, 1.000000000000000000, 0.8660254037844387076, 1.000000000000000000, 0.8660254037844387076, 1.000000000000000000, 0.8660254037844387076, 1.000000000000000000, 0.8660254037844387076, 1.000000000000000000, 0.8660254037844387076, 1.000000000000000000, 0.8660254037844387076, 1.000000000000000000, 0.8660254037844387076, 1.000000000000000000, 0.8660254037844387076, 1.000000000000000000, 0.8660254037844387076, 1.000000000000000000, 0.8660254037844387076, 1.000000000000000000, 0.8660254037844387076, 1.000000000000000000, 0.8660254037844387076, 1.000000000000000000, 0.8660254037844387076, 1.000000000000000000, 0.8660254037844387076, 1.000000000000000000, 0.8660254037844387076, 1.000000000000000000, 0.8660254037844387076, 1.000000000000000000, 0.8660254037844387076, 1.000000000000000000, 0.8660254037844387076, 1.000000000000000000, 0.8660254037844387076, 1.000000000000000000, 0.8660254037844387076, 1.000000000000000000, 0.8660254037844387076, 1.000000000000000000, 0.8660254037844387076, 1.000000000000000000, 0.8660254037844387076, 1.000000000000000000, 0.8660254037844387076, 1.000000000000000000, 0.8660254037844387076, 1.000000000000000000, 0.8660254037844387076, 1.000000000000000000, 0.8660254037844387076, 1.000000000000000000, 0.8660254037844387076, 1.000000000000000000, 0.8660254037844387076, 1.000000000000000000, 0.8660254037844387076, 1.000000000000000000, 0.8660254037844387076, 1.000000000000000000, 0.8660254037844387076, 1.000000000000000000, 0.8660254037844387076, 1.000000000000000000, 0.8660254037844387076, 1.000000000000000000, 0.8660254037844387076, 1.000000000000000000, 0.8660254037844387076, 1.000000000000000000, 0.8660254037844387076, 1.000000000000000000, 0.8660254037844387076, 1.000000000000000000, 0.8660254037844387076, 1.000000000000000000, 0.8660254037844387076, 1.000000000000000000, 0.8660254037844387076, 1.000000000000000000, 0.8660254037844387076, 1.000000000000000000, 0.8660254037844387076, 1.000000000000000000, 0.8660254037844387076, 1.000000000000000000, 0.8660254037844387076, 1.000000000000000000, 0.8660254037844387076, 1.000000000000000000, 0.8660254037844387076, 1.000000000000000000, 0.8660254037844387076, 1.000000000000000000, 0.8660254037844387076, 1.000000000000000000, 0.8660254037844387076, 1.000000000000000000, 0.8660254037844387076, 1.000000000000000000, 0.8660254037844387076, 1.000000000000000000, 0.8660254037844387076, 1.000000000000000000, 0.8660254037844387076, 1.000000000000000000, 0.8660254037844387076, 1.000000000000000000, 0.8660254037844387076, 1.000000000000000000, 0.8660254037844387076, 1.000000000000000000, 0.8660254037844387076, 1.000000000000000000, 0.8660254037844387076, 1.000000000000000000, 0.8660254037844387076, 1.000000000000000000, 0.8660254037844387076, 1.000000000000000000, 0.8660254037844387076, 1.000000000000000000, 0.8660254037844387076, 1.000000000000000000, 0.8660254037844387076, 1.000000000000000000, 0.8660254037844387076, 1.000000000000000000, 0.8660254037844387076, 1.000000000000000000, 0.8660254037844387076, 1.000000000000000000, 0.8660254037844387076, 1.000000000000000000, 0.8660254037844387076, 1.000000000000000000, 0.8660254037844387076, 1.000000000000000000, 0.8660254037844387076, 1.000000000000000000, 0.8660254037844387076, 1.000000000000000000, 0.8660254037844387076, 1.000000000000000000, 0.8660254037844387076, 1.000000000000000000, 0.8660254037844387076, 1.000000000000000000, 0.8660254037844387076, 1.000000000000000000, 0.8660254037844387076, 1.000000000000000000, 0.8660254037844387076, 1.000000000000000000, 0.8660254037844387076, 1.000000000000000000, 0.8660254037844387076, 1.000000000000000000, 0.8660254037844387076, 1.000000000000000000, 0.8660254037844387076, 1.000000000000000000, 0.8660254037844387076, 1.000000000000000000, 0.8660254037844387076, 1.000000000000000000, 0.8660254037844387076, 1.000000000000000000, 0.8660254037844387076, 1.000000000000000000, 0.8660254037844387076, 1.000000000000000000, 0.8660254037844387076, 1.000000000000000000, 0.8660254037844387076, 1.000000000000000000, 0.8660254037844387076, 1.000000000000000000, 0.8660254037844387076, 1.000000000000000000, 0.8660254037844387076, 1.000000000000000000, 0.8660254037844387076, 1.000000000000000000, 0.8660254037844387076, 1.000000000000000000, 0.8660254037844387076, 1.000000000000000000, 0.8660254037844387076, 1.000000000000000000, 0.8660254037844387076, 1.000000000000000000, 0.8660254037844387076, 1.000000000000000000, 0.8660254037844387076, 1.000000000000000000, 0.8660254037844387076, 1.000000000000000000, 0.8660254037844387076, 1.000000000000000000, 0.8660254037844387076, 1.000000000000000000, 0.8660254037844387076, 1.000000000000000000, 0.8660254037844387076, 1.000000000000000000, 0.8660254037844387076, 1.000000000000000000, 0.8660254037844387076, 1.000000000000000000, 0.8660254037844387076, 1.000000000000000000, 0.8660254037844387076, 1.000000000000000000, 0.8660254037844387076, 1.000000000000000000, 0.8660254037844387076, 1.000000000000000000, 0.8660254037844387076, 1.000000000000000000, 0.8660254037844387076, 1.000000000000000000, 0.8660254037844387076, 1.000000000000000000, 0.8660254037844387076, 1.000000000000000000, 0.8660254037844387076, 1.000000000000000000, 0.8660254037844387076, 1.000000000000000000, 0.8660254037844387076, 1.000000000000000000, 0.8660254037844387076, 1.000000000000000000, 0.8660254037844387076, 1.000000000000000000, 0.8660254037844387076, 1.000000000000000000, 0.8660254037844387076, 1.000000000000000000, 0.8660254037844387076, 1.000000000000000000, 0.8660254037844387076, 1.000000000000000000, 0.8660254037844387076, 1.000000000000000000, 0.8660254037844387076, 1.000000000000000000, 0.8660254037844387076, 1.000000000000000000, 0.8660254037844387076, 1.000000000000000000, 0.8660254037844387076, 1.000000000000000000, 0.8660254037844387076, 1.000000000000000000, 0.8660254037844387076, 1.000000000000000000, 0.8660254037844387076, 1.000000000000000000, 0.8660254037844387076, 1.000000000000000000, 0.8660254037844387076, 1.000000000000000000, 0.8660254037844387076, 1.000000000000000000, 0.8660254037844387076, 1.000000000000000000, 0.8660254037844387076, 1.000000000000000000, 0.8660254037844387076, 1.000000000000000000, 0.8660254037844387076, 1.000000000000000000, 0.8660254037844387076, 1.000000000000000000, 0.8660254037844387076, 1.000000000000000000, 0.8660254037844387076, 1.000000000000000000, 0.8660254037844387076, 1.000000000000000000, 0.8660254037844387076, 1.000000000000000000, 0.8660254037844387076, 1.000000000000000000, 0.8660254037844387076, 1.000000000000000000, 0.8660254037844387076, 1.000000000000000000, 0.8660254037844387076, 1.000000000000000000, 0.8660254037844387076, 1.000000000000000000, 0.8660254037844387076, 1.000000000000000000, 0.8660254037844387076, 1.000000000000000000, 0.8660254037844387076, 1.000000000000000000, 0.8660254037844387076, 1.000000000000000000, 0.8660254037844387076, 1.000000000000000000, 0.8660254037844387076, 1.000000000000000000, 0.8660254037844387076, 1.000000000000000000, 0.8660254037844387076, 1.000000000000000000, 0.8660254037844387076, 1.000000000000000000, 0.8660254037844387076, 1.000000000000000000, 0.8660254037844387076, 1.000000000000000000, 0.8660254037844387076, 1.000000000000000000, 0.8660254037844387076, 1.000000000000000000, 0.8660254037844387076, 1.000000000000000000, 0.8660254037844387076, 1.000000000000000000, 0.8660254037844387076, 1.000000000000000000, 0.8660254037844387076, 1.000000000000000000, 0.8660254037844387076, 1.000000000000000000, 0.8660254037844387076, 1.000000000000000000, 0.8660254037844387076, 1.000000000000000000, 0.8660254037844387076, 1.000000000000000000, 0.8660254037844387076, 1.000000000000000000, 0.8660254037844387076, 1.000000000000000000, 0.8660254037844387076, 1.000000000000000000, 0.8660254037844387076, 1.000000000000000000, 0.8660254037844387076, 1.000000000000000000, 0.8660254037844387076, 1.000000000000000000, 0.8660254037844387076, 1.000000000000000000, 0.8660254037844387076, 1.000000000000000000, 0.8660254037844387076, 1.000000000000000000, 0.8660254037844387076, 1.000000000000000000, 0.8660254037844387076, 1.000000000000000000, 0.8660254037844387076, 1.000000000000000000, 0.8660254037844387076, 1.000000000000000000, 0.8660254037844387076, 1.000000000000000000, 0.8660254037844387076, 1.000000000000000000, 0.8660254037844387076, 1.000000000000000000, 0.8660254037844387076, 1.000000000000000000, 0.8660254037844387076, 1.000000000000000000, 0.8660254037844387076, 1.000000000000000000, 0.8660254037844387076, 1.000000000000000000, 0.8660254037844387076, 1.000000000000000000, 0.8660254037844387076, 1.000000000000000000, 0.8660254037844387076, 1.000000000000000000, 0.8660254037844387076, 1.000000000000000000, 0.8660254037844387076, 1.000000000000000000, 0.8660254037844387076, 1.000000000000000000, 0.8660254037844387076, 1.000000000000000000, 0.8660254037844387076, 1.000000000000000000, 0.8660254037844387076, 1.000000000000000000, 0.8660254037844387076, 1.000000000000000000, 0.8660254037844387076, 1.000000000000000000, 0.8660254037844387076, 1.000000000000000000, 0.8660254037844387076, 1.000000000000000000, 0.8660254037844387076, 1.000000000000000000, 0.8660254037844387076, 1.000000000000000000, 0.8660254037844387076, 1.000000000000000000, 0.8660254037844387076, 1.000000000000000000, 0.8660254037844387076, 1.000000000000000000, 0.8660254037844387076, 1.000000000000000000, 0.8660254037844387076, 1.000000000000000000, 0.8660254037844387076, 1.000000000000000000, 0.8660254037844387076, 1.000000000000000000, 0.8660254037844387076, 1.000000000000000000, 0.8660254037844387076, 1.000000000000000000, 0.8660254037844387076, 1.000000000000000000),
 ( 1.000000000000000000, 0.8660254037844387076, 1.000000000000000000, 0.8660254037844387076, 1.000000000000000000, 0.8660254037844387076, 1.000000000000000000, 0.8660254037844387076, 1.000000000000000000, 0.8660254037844387076, 1.000000000000000000, 0.8660254037844387076, 1.000000000000000000, 0.8660254037844387076, 1.000000000000000000, 0.8660254037844387076, 1.000000000000000000, 0.8660254037844387076, 1.000000000000000000, 0.8660254037844387076, 1.000000000000000000, 0.8660254037844387076, 1.000000000000000000, 0.8660254037844387076, 1.000000000000000000, 0.8660254037844387076, 1.000000000000000000, 0.8660254037844387076, 1.000000000000000000, 0.8660254037844387076, 1.000000000000000000, 0.8660254037844387076, 1.000000000000000000, 0.8660254037844387076, 1.000000000000000000, 0.8660254037844387076, 1.000000000000000000, 0.8660254037844387076, 1.000000000000000000, 0.8660254037844387076, 1.000000000000000000, 0.8660254037844387076, 1.000000000000000000, 0.8660254037844387076, 1.000000000000000000, 0.8660254037844387076, 1.000000000000000000, 0.8660254037844387076, 1.000000000000000000, 0.8660254037844387076, 1.000000000000000000, 0.8660254037844387076, 1.000000000000000000, 0.8660254037844387076, 1.000000000000000000, 0.8660254037844387076, 1.000000000000000000, 0.8660254037844387076, 1.000000000000000000, 0.8660254037844387076, 1.000000000000000000, 0.8660254037844387076, 1.000000000000000000, 0.8660254037844387076, 1.000000000000000000, 0.8660254037844387076, 1.000000000000000000, 0.8660254037844387076, 1.000000000000000000, 0.8660254037844387076, 1.000000000000000000, 0.8660254037844387076, 1.000000000000000000, 0.8660254037844387076, 1.000000000000000000, 0.8660254037844387076, 1.000000000000000000, 0.8660254037844387076, 1.000000000000000000, 0.8660254037844387076, 1.000000000000000000, 0.8660254037844387076, 1.000000000000000000, 0.8660254037844387076, 1.000000000000000000, 0.8660254037844387076, 1.000000000000000000, 0.8660254037844387076, 1.000000000000000000, 0.8660254037844387076, 1.000000000000000000, 0.8660254037844387076, 1.000000000000000000, 0.8660254037844387076, 1.000000000000000000, 0.8660254037844387076, 1.000000000000000000, 0.8660254037844387076, 1.000000000000000000, 0.8660254037844387076, 1.000000000000000000, 0.8660254037844387076, 1.000000000000000000, 0.8660254037844387076, 1.000000000000000000, 0.8660254037844387076, 1.000000000000000000, 0.8660254037844387076, 1.000000000000000000, 0.8660254037844387076, 1.000000000000000000, 0.8660254037844387076, 1.000000000000000000, 0.8660254037844387076, 1.000000000000000000, 0.8660254037844387076, 1.000000000000000000, 0.8660254037844387076, 1.000000000000000000, 0.8660254037844387076, 1.000000000000000000, 0.8660254037844387076, 1.000000000000000000, 0.8660254037844387076, 1.000000000000000000, 0.8660254037844387076, 1.000000000000000000, 0.8660254037844387076, 1.000000000000000000, 0.8660254037844387076, 1.000000000000000000, 0.8660254037844387076, 1.000000000000000000, 0.8660254037844387076, 1.000000000000000000, 0.8660254037844387076, 1.000000000000000000, 0.8660254037844387076, 1.000000000000000000, 0.8660254037844387076, 1.000000000000000000, 0.8660254037844387076, 1.000000000000000000, 0.8660254037844387076, 1.000000000000000000, 0.8660254037844387076, 1.000000000000000000, 0.8660254037844387076, 1.000000000000000000, 0.8660254037844387076, 1.000000000000000000, 0.8660254037844387076, 1.000000000000000000, 0.8660254037844387076, 1.000000000000000000, 0.8660254037844387076, 1.000000000000000000, 0.8660254037844387076, 1.000000000000000000, 0.8660254037844387076, 1.000000000000000000, 0.8660254037844387076, 1.000000000000000000, 0.8660254037844387076, 1.000000000000000000, 0.8660254037844387076, 1.000000000000000000, 0.8660254037844387076, 1.000000000000000000, 0.8660254037844387076, 1.000000000000000000, 0.8660254037844387076, 1.000000000000000000, 0.8660254037844387076, 1.000000000000000000, 0.8660254037844387076, 1.000000000000000000, 0.8660254037844387076, 1.000000000000000000, 0.8660254037844387076, 1.000000000000000000, 0.8660254037844387076, 1.000000000000000000, 0.8660254037844387076, 1.000000000000000000, 0.8660254037844387076, 1.000000000000000000, 0.8660254037844387076, 1.000000000000000000, 0.8660254037844387076, 1.000000000000000000, 0.8660254037844387076, 1.000000000000000000, 0.8660254037844387076, 1.000000000000000000, 0.8660254037844387076, 1.000000000000000000, 0.8660254037844387076, 1.000000000000000000, 0.8660254037844387076, 1.000000000000000000, 0.8660254037844387076, 1.000000000000000000, 0.8660254037844387076, 1.000000000000000000, 0.8660254037844387076, 1.000000000000000000, 0.8660254037844387076, 1.000000000000000000, 0.8660254037844387076, 1.000000000000000000, 0.8660254037844387076, 1.000000000000000000, 0.8660254037844387076, 1.000000000000000000, 0.8660254037844387076, 1.000000000000000000, 0.8660254037844387076, 1.000000000000000000, 0.8660254037844387076, 1.000000000000000000, 0.8660254037844387076, 1.000000000000000000, 0.8660254037844387076, 1.000000000000000000, 0.8660254037844387076, 1.000000000000000000, 0.8660254037844387076, 1.000000000000000000, 0.8660254037844387076, 1.000000000000000000, 0.8660254037844387076, 1.000000000000000000, 0.8660254037844387076, 1.000000000000000000, 0.8660254037844387076, 1.000000000000000000, 0.8660254037844387076, 1.000000000000000000, 0.8660254037844387076, 1.000000000000000000, 0.8660254037844387076, 1.000000000000000000, 0.8660254037844387076, 1.000000000000000000, 0.8660254037844387076, 1.000000000000000000, 0.8660254037844387076, 1.000000000000000000, 0.8660254037844387076, 1.000000000000000000, 0.8660254037844387076, 1.000000000000000000, 0.8660254037844387076, 1.000000000000000000, 0.8660254037844387076, 1.000000000000000000, 0.8660254037844387076, 1.000000000000000000, 0.8660254037844387076, 1.000000000000000000, 0.8660254037844387076, 1.000000000000000000, 0.8660254037844387076, 1.000000000000000000, 0.8660254037844387076, 1.000000000000000000, 0.8660254037844387076, 1.000000000000000000, 0.8660254037844387076, 1.000000000000000000, 0.8660254037844387076, 1.000000000000000000, 0.8660254037844387076, 1.000000000000000000, 0.8660254037844387076, 1.000000000000000000, 0.8660254037844387076, 1.000000000000000000, 0.8660254037844387076, 1.000000000000000000, 0.8660254037844387076, 1.000000000000000000, 0.8660254037844387076, 1.000000000000000000, 0.8660254037844387076, 1.000000000000000000, 0.8660254037844387076, 1.000000000000000000, 0.8660254037844387076, 1.000000000000000000, 0.8660254037844387076, 1.000000000000000000, 0.8660254037844387076, 1.000000000000000000, 0.8660254037844387076, 1.000000000000000000, 0.8660254037844387076, 1.000000000000000000, 0.8660254037844387076, 1.000000000000000000, 0.8660254037844387076, 1.000000000000000000, 0.8660254037844387076, 1.000000000000000000, 0.8660254037844387076, 1.000000000000000000, 0.8660254037844387076, 1.000000000000000000, 0.8660254037844387076, 1.000000000000000000, 0.8660254037844387076, 1.000000000000000000, 0.8660254037844387076, 1.000000000000000000, 0.8660254037844387076, 1.000000000000000000, 0.8660254037844387076, 1.000000000000000000, 0.8660254037844387076, 1.000000000000000000, 0.8660254037844387076, 1.000000000000000000, 0.8660254037844387076, 1.000000000000000000, 0.8660254037844387076, 1.000000000000000000, 0.8660254037844387076, 1.000000000000000000, 0.8660254037844387076, 1.000000000000000000, 0.8660254037844387076, 1.000000000000000000, 0.8660254037844387076, 1.000000000000000000, 0.8660254037844387076, 1.000000000000000000, 0.8660254037844387076, 1.000000000000000000, 0.8660254037844387076, 1.000000000000000000, 0.8660254037844387076, 1.000000000000000000, 0.8660254037844387076, 1.000000000000000000, 0.8660254037844387076, 1.000000000000000000, 0.8660254037844387076, 1.000000000000000000, 0.8660254037844387076, 1.000000000000000000, 0.8660254037844387076, 1.000000000000000000, 0.8660254037844387076, 1.000000000000000000, 0.8660254037844387076, 1.000000000000000000, 0.8660254037844387076, 1.000000000000000000, 0.8660254037844387076, 1.000000000000000000, 0.8660254037844387076, 1.000000000000000000, 0.8660254037844387076, 1.000000000000000000, 0.8660254037844387076, 1.000000000000000000, 0.8660254037844387076, 1.000000000000000000, 0.8660254037844387076, 1.000000000000000000, 0.8660254037844387076, 1.000000000000000000, 0.8660254037844387076, 1.000000000000000000, 0.8660254037844387076, 1.000000000000000000, 0.8660254037844387076, 1.000000000000000000, 0.8660254037844387076, 1.000000000000000000, 0.8660254037844387076, 1.000000000000000000, 0.8660254037844387076, 1.000000000000000000, 0.8660254037844387076, 1.000000000000000000, 0.8660254037844387076, 1.000000000000000000, 0.8660254037844387076, 1.000000000000000000, 0.8660254037844387076, 1.000000000000000000, 0.8660254037844387076, 1.000000000000000000, 0.8660254037844387076, 1.000000000000000000, 0.8660254037844387076, 1.000000000000000000, 0.8660254037844387076, 1.000000000000000000, 0.8660254037844387076, 1.000000000000000000, 0.8660254037844387076, 1.000000000000000000, 0.8660254037844387076, 1.000000000000000000, 0.8660254037844387076, 1.000000000000000000, 0.8660254037844387076, 1.000000000000000000, 0.8660254037844387076, 1.000000000000000000, 0.8660254037844387076, 1.000000000000000000, 0.8660254037844387076, 1.000000000000000000, 0.8660254037844387076, 1.000000000000000000, 0.8660254037844387076, 1.000000000000000000, 0.8660254037844387076, 1.000000000000000000, 0.8660254037844387076, 1.000000000000000000, 0.8660254037844387076, 1.000000000000000000, 0.8660254037844387076, 1.000000000000000000, 0.8660254037844387076, 1.000000000000000000, 0.8660254037844387076, 1.000000000000000000, 0.8660254037844387076, 1.000000000000000000, 0.8660254037844387076, 1.000000000000000000, 0.8660254037844387076, 1.000000000000000000, 0.8660254037844387076, 1.000000000000000000, 0.8660254037844387076, 1.000000000000000000, 0.8660254037844387076, 1.000000000000000000, 0.8660254037844387076, 1.000000000000000000, 0.8660254037844387076, 1.000000000000000000, 0.8660254037844387076, 1.000000000000000000, 0.8660254037844387076, 1.000000000000000000, 0.8660254037844387076, 1.000000000000000000, 0.8660254037844387076, 1.000000000000000000, 0.8660254037844387076, 1.000000000000000000, 0.8660254037844387076, 1.000000000000000000, 0.8660254037844387076, 1.000000000000000000, 0.8660254037844387076, 1.000000000000000000, 0.8660254037844387076, 1.000000000000000000, 0.8660254037844387076, 1.000000000000000000, 0.8660254037844387076, 1.000000000000000000, 0.8660254037844387076, 1.000000000000000000, 0.8660254037844387076, 1.000000000000000000, 0.8660254037844387076, 1.000000000000000000, 0.8660254037844387076, 1.000000000000000000, 0.8660254037844387076, 1.000000000000000000, 0.8660254037844387076, 1.000000000000000000, 0.8660254037844387076, 1.000000000000000000, 0.8660254037844387076, 1.000000000000000000, 0.8660254037844387076, 1.000000000000000000, 0.8660254037844387076, 1.000000000000000000, 0.8660254037844387076, 1.000000000000000000, 0.8660254037844387076, 1.000000000000000000, 0.8660254037844387076, 1.000000000000000000, 0.8660254037844387076, 1.000000000000000000, 0.8660254037844387076, 1.000000000000000000, 0.8660254037844387076, 1.000000000000000000, 0.8660254037844387076, 1.000000000000000000, 0.8660254037844387076, 1.000000000000000000, 0.8660254037844387076, 1.000000000000000000, 0.8660254037844387076, 1.000000000000000000, 0.8660254037844387076, 1.000000000000000000, 0.8660254037844387076, 1.000000000000000000, 0.8660254037844387076, 1.000000000000000000, 0.8660254037844387076, 1.000000000000000000, 0.8660254037844387076, 1.000000000000000000, 0.8660254037844387076, 1.000000000000000000, 0.8660254037844387076, 1.000000000000000000, 0.8660254037844387076, 1.000000000000000000, 0.8660254037844387076, 1.000000000000000000, 0.8660254037844387076, 1.000000000000000000, 0.8660254037844387076, 1.000000000000000000, 0.8660254037844387076, 1.000000000000000000, 0.8660254037844387076, 1.000000000000000000, 0.8660254037844387076, 1.000000000000000000, 0.8660254037844387076, 1.000000000000000000, 0.8660254037844387076, 1.000000000000000000, 0.8660254037844387076, 1.000000000000000000, 0.8660254037844387076, 1.000000000000000000, 0.8660254037844387076, 1.000000000000000000, 0.8660254037844387076, 1.000000000000000000, 0.8660254037844387076, 1.000000000000000000, 0.8660254037844387076, 1.000000000000000000, 0.8660254037844387076, 1.000000000000000000, 0.8660254037844387076, 1.000000000000000000, 0.8660254037844387076, 1.000000000000000000, 0.8660254037844387076, 1.000000000000000000, 0.8660254037844387076, 1.000000000000000000, 0.8660254037844387076, 1.000000000000000000, 0.8660254037844387076, 1.000000000000000000, 0.8660254037844387076, 1.000000000000000000, 0.8660254037844387076, 1.000000000000000000, 0.8660254037844387076, 1.000000000000000000, 0.8660254037844387076, 1.000000000000000000, 0.8660254037844387076, 1.000000000000000000, 0.8660254037844387076, 1.000000000000000000, 0.8660254037844387076, 1.000000000000000000, 0.8660254037844387076, 1.000000000000000000, 0.8660254037844387076, 1.000000000000000000, 0.8660254037844387076, 1.000000000000000000, 0.8660254037844387076, 1.000000000000000000, 0.8660254037844387076, 1.000000000000000000, 0.8660254037844387076, 1.000000000000000000, 0.8660254037844387076, 1.000000000000000000, 0.8660254037844387076, 1.000000000000000000, 0.8660254037844387076, 1.000000000000000000, 0.8660254037844387076, 1.000000000000000000, 0.8660254037844387076, 1.000000000000000000, 0.8660254037844387076, 1.000000000000000000, 0.8660254037844387076, 1.000000000000000000, 0.8660254037844387076, 1.000000000000000000, 0.8660254037844387076, 1.000000000000000000, 0.8660254037844387076, 1.000000000000000000, 0.8660254037844387076, 1.000000000000000000, 0.8660254037844387076, 1.000000000000000000, 0.8660254037844387076, 1.000000000000000000, 0.8660254037844387076, 1.000000000000000000, 0.8660254037844387076, 1.000000000000000000, 0.8660254037844387076, 1.000000000000000000, 0.8660254037844387076, 1.000000000000000000, 0.8660254037844387076, 1.000000000000000000, 0.8660254037844387076, 1.000000000000000000, 0.8660254037844387076, 1.000000000000000000, 0.8660254037844387076, 1.000000000000000000, 0.8660254037844387076, 1.000000000000000000, 0.8660254037844387076, 1.000000000000000000, 0.8660254037844387076, 1.000000000000000000, 0.8660254037844387076, 1.000000000000000000, 0.8660254037844387076, 1.000000000000000000, 0.8660254037844387076, 1.000000000000000000, 0.8660254037844387076, 1.000000000000000000, 0.8660254037844387076, 1.000000000000000000, 0.8660254037844387076, 1.000000000000000000, 0.8660254037844387076, 1.000000000000000000, 0.8660254037844387076, 1.000000000000000000, 0.8660254037844387076, 1.000000000000000000, 0.8660254037844387076, 1.000000000000000000, 0.8660254037844387076, 1.000000000000000000, 0.8660254037844387076, 1.000000000000000000, 0.8660254037844387076, 1.000000000000000000, 0.8660254037844387076, 1.000000000000000000, 0.8660254037844387076, 1.000000000000000000, 0.8660254037844387076, 1.000000000000000000, 0.8660254037844387076, 1.000000000000000000, 0.8660254037844387076, 1.000000000000000000, 0.8660254037844387076, 1.000000000000000000, 0.8660254037844387076, 1.000000000000000000, 0.8660254037844387076, 1.000000000000000000, 0.8660254037844387076, 1.000000000000000000, 0.8660254037844387076, 1.000000000000000000, 0.8660254037844387076, 1.000000000000000000, 0.8660254037844387076, 1.000000000000000000, 0.8660254037844387076, 1.000000000000000000, 0.8660254037844387076, 1.000000000000000000, 0.8660254037844387076, 1.000000000000000000, 0.8660254037844387076, 1.000000000000000000, 0.8660254037844387076, 1.000000000000000000, 0.8660254037844387076, 1.000000000000000000, 0.8660254037844387076, 1.000000000000000000, 0.8660254037844387076, 1.000000000000000000, 0.8660254037844387076, 1.000000000000000000, 0.8660254037844387076, 1.000000000000000000, 0.8660254037844387076, 1.000000000000000000, 0.8660254037844387076, 1.000000000000000000, 0.8660254037844387076, 1.000000000000000000, 0.8660254037844387076, 1.000000000000000000) ) ) 
 REPRESENTATION_ITEM ( '' )  SURFACE ( )  );
#68239 = CARTESIAN_POINT ( 'NONE',  ( 27.68437500061451573, -4.541064518000419881, 2.621784821874995952 ) ) ;
#68240 = ORIENTED_EDGE ( 'NONE', *, *, #64237, .F. ) ;
#68241 = CARTESIAN_POINT ( 'NONE',  ( 14.87812500061451537, 4.541064518000418104, 2.621784821874999949 ) ) ;
#68242 = CARTESIAN_POINT ( 'NONE',  ( 8.053125000614516082, 4.541064518000418104, -2.621784821874998173 ) ) ;
#68243 = CARTESIAN_POINT ( 'NONE',  ( 17.82187500061451502, 5.824947211148865298E-16, -4.756430356249998326 ) ) ;
#68244 = CARTESIAN_POINT ( 'NONE',  ( 4.209375000614516971, 0.000000000000000000, 5.243569643749999010 ) ) ;
#68245 = CARTESIAN_POINT ( 'NONE',  ( 17.10000000122903430, -2.886751345948129988, 4.999999999999997335 ) ) ;
#68246 = CARTESIAN_POINT ( 'NONE',  ( 21.60000000000000142, -4.330127018922190985, -2.500000000000001332 ) ) ;
#68247 = CARTESIAN_POINT ( 'NONE',  ( 29.73750000000000071, -2.886751345948125991, -5.000000000000000000 ) ) ;
#68248 = CARTESIAN_POINT ( 'NONE',  ( 3.534375000614518036, 6.421520780324663323E-16, -5.243569643749999010 ) ) ;
#68249 = CARTESIAN_POINT ( 'NONE',  ( 12.00937500061451857, -4.541064518000417216, -2.621784821875001281 ) ) ;
#68250 = CARTESIAN_POINT ( 'NONE',  ( 22.73437500061451644, -4.541064518000419881, 2.621784821874995952 ) ) ;
#68251 = CARTESIAN_POINT ( 'NONE',  ( -3.999999999999999112, 15.12500000122903465, -32.30940107675850470 ) ) ;
#68252 = VERTEX_POINT ( 'NONE', #27051 ) ;
#68253 = EDGE_CURVE ( 'NONE', #69015, #38031, #55484, .T. ) ;
#68254 = CARTESIAN_POINT ( 'NONE',  ( 3.234375000614516438, 4.541064518000418104, 2.621784821874999949 ) ) ;
#68255 = CARTESIAN_POINT ( 'NONE',  ( 7.434375000614519280, -4.541064518000419881, 2.621784821874995952 ) ) ;
#68256 = CARTESIAN_POINT ( 'NONE',  ( 18.56250000000000000, 2.886751345948129099, -4.999999999999998224 ) ) ;
#68257 = CARTESIAN_POINT ( 'NONE',  ( 16.64062500061451289, 6.054752690667223547, 3.707466751127219781E-16 ) ) ;
#68258 = CARTESIAN_POINT ( 'NONE',  ( -3.999999999999999556, 20.33749999999999858, 27.69059892324149175 ) ) ;
#68259 = DIRECTION ( 'NONE',  ( -1.000000000000000000, -0.000000000000000000, -0.000000000000000000 ) ) ;
#68260 = CARTESIAN_POINT ( 'NONE',  ( 19.77187500061451786, 2.746126346562645981, -4.756430356249997438 ) ) ;
#68261 = CARTESIAN_POINT ( 'NONE',  ( 9.628125000614517148, -4.541064518000419881, 2.621784821874995952 ) ) ;
#68262 = CARTESIAN_POINT ( 'NONE',  ( 25.54687500061451644, -3.027376345333610441, -5.243569643749999898 ) ) ;
#68263 = CARTESIAN_POINT ( 'NONE',  ( 28.36875000122903145, -5.773502691896255534, -1.060575238724906372E-15 ) ) ;
#68264 = CARTESIAN_POINT ( 'NONE',  ( 25.39687500061451431, -3.027376345333614438, 5.243569643749998122 ) ) ;
#68265 = CARTESIAN_POINT ( 'NONE',  ( 7.387500000000001066, 5.773502691896255534, 3.535250795749688894E-16 ) ) ;
#68266 = CARTESIAN_POINT ( 'NONE',  ( -3.999999999999997335, 14.30000000122903359, 32.30940107675850470 ) ) ;
#68267 = CARTESIAN_POINT ( 'NONE',  ( 8.625000001229034652, -5.773502691896255534, -1.060575238724906372E-15 ) ) ;
#68268 = CARTESIAN_POINT ( 'NONE',  ( 20.07187500061451857, -6.054752690667223547, -1.112240025338166033E-15 ) ) ;
#68269 = CARTESIAN_POINT ( 'NONE',  ( 12.19687500061451679, 6.054752690667223547, 3.707466751127219781E-16 ) ) ;
#68270 = CARTESIAN_POINT ( 'NONE',  ( 2.000000000000000444, 13.86874999877096748, 26.53589838486224650 ) ) ;
#68271 = VERTEX_POINT ( 'NONE', #9321 ) ;
#68272 = CARTESIAN_POINT ( 'NONE',  ( 14.99062500061451786, -3.027376345333614438, 5.243569643749998122 ) ) ;
#68273 = CARTESIAN_POINT ( 'NONE',  ( 26.25000000122903288, -2.886751345948125991, -5.000000000000000000 ) ) ;
#68274 = CARTESIAN_POINT ( 'NONE',  ( 11.63437500061451857, 6.421520780324663323E-16, -5.243569643749999010 ) ) ;
#68275 = CARTESIAN_POINT ( 'NONE',  ( 4.000000000000000000, 12.65000000122903323, 32.30940107675849760 ) ) ;
#68276 = CARTESIAN_POINT ( 'NONE',  ( 16.86562500061451786, -6.054752690667223547, -1.112240025338166033E-15 ) ) ;
#68277 = CARTESIAN_POINT ( 'NONE',  ( 26.32500000122903216, 2.886751345948129099, -4.999999999999997335 ) ) ;
#68278 = CARTESIAN_POINT ( 'NONE',  ( 26.85937500061451644, -4.541064518000417216, -2.621784821875001281 ) ) ;
#68279 = CARTESIAN_POINT ( 'NONE',  ( -2.121784821874996840, 9.978125000614518569, 33.67503911421598417 ) ) ;
#68280 = EDGE_CURVE ( 'NONE', #27910, #70559, #41901, .T. ) ;
#68281 = CARTESIAN_POINT ( 'NONE',  ( 10.91250000122903252, -4.330127018922190985, -2.500000000000001332 ) ) ;
#68282 = CARTESIAN_POINT ( 'NONE',  ( 7.546875000614515550, -2.746126346562641984, -4.756430356249999214 ) ) ;
#68283 = CARTESIAN_POINT ( 'NONE',  ( -4.243569643749999898, 17.12187500061451573, -32.45002607614398471 ) ) ;
#68284 = CARTESIAN_POINT ( 'NONE',  ( 18.53437500061451715, 4.541064518000418104, 2.621784821874999949 ) ) ;
#68285 = CARTESIAN_POINT ( 'NONE',  ( 19.98750000122903359, 6.123233995736764310E-16, -4.999999999999998224 ) ) ;
#68286 = ADVANCED_FACE ( 'NONE', ( #31854 ), #18790, .T. ) ;
#68287 = CARTESIAN_POINT ( 'NONE',  ( 15.38437500061451679, 4.541064518000418104, 2.621784821874999949 ) ) ;
#68288 = CARTESIAN_POINT ( 'NONE',  ( -4.243569643749999898, 10.85937500061451821, 30.00000000000000000 ) ) ;
#68289 = CARTESIAN_POINT ( 'NONE',  ( 21.93750000122903288, 4.330127018922191873, 2.499999999999999556 ) ) ;
#68290 = CARTESIAN_POINT ( 'NONE',  ( 14.35312500061451679, 4.541064518000418104, -2.621784821874998173 ) ) ;
#68291 = CARTESIAN_POINT ( 'NONE',  ( 28.90312500061451217, 0.000000000000000000, 5.243569643749999010 ) ) ;
#68292 = VERTEX_POINT ( 'NONE', #20516 ) ;
#68293 = VERTEX_POINT ( 'NONE', #2815 ) ;
#68294 = CARTESIAN_POINT ( 'NONE',  ( 18.45000000000000284, -4.330127018922190985, -2.500000000000001332 ) ) ;
#68295 = CARTESIAN_POINT ( 'NONE',  ( 1.071796769724491227, 14.39240381056766438, 26.00000000000000000 ) ) ;
#68296 = CARTESIAN_POINT ( 'NONE',  ( 0.6891293861215573857, 4.954145703890282526, 33.94256940425900382 ) ) ;
#68297 = CARTESIAN_POINT ( 'NONE',  ( 14.66250000122903252, 4.330127018922192761, -2.499999999999997780 ) ) ;
#68298 = CARTESIAN_POINT ( 'NONE',  ( 20.76562500061451644, 3.027376345333611329, 5.243569643749999010 ) ) ;
#68299 = CARTESIAN_POINT ( 'NONE',  ( 23.76562500061451644, 3.027376345333613106, -5.243569643749998122 ) ) ;
#68300 = CARTESIAN_POINT ( 'NONE',  ( 3.890625000614517326, -3.027376345333610441, -5.243569643749999898 ) ) ;
#68301 =( BOUNDED_CURVE ( )  B_SPLINE_CURVE ( 3, ( #15727, #14631, #37905, #37171 ),
 .UNSPECIFIED., .F., .F. ) 
 B_SPLINE_CURVE_WITH_KNOTS ( ( 4, 4 ),
 ( 4.024033675728571069, 4.052330423520261959 ),
 .UNSPECIFIED. ) 
 CURVE ( )  GEOMETRIC_REPRESENTATION_ITEM ( )  RATIONAL_B_SPLINE_CURVE ( ( 1.000000000000000000, 0.9999332756184333704, 0.9999332756184333704, 1.000000000000000000 ) ) 
 REPRESENTATION_ITEM ( '' )  );
#68302 = CARTESIAN_POINT ( 'NONE',  ( 11.55000000000000071, 0.000000000000000000, 4.999999999999998224 ) ) ;
#68303 = CARTESIAN_POINT ( 'NONE',  ( 5.812500001229035540, 0.000000000000000000, 4.999999999999998224 ) ) ;
#68304 = CARTESIAN_POINT ( 'NONE',  ( 8.371875000614515727, -5.492252693125287522, -1.008910452111647106E-15 ) ) ;
#68305 = CARTESIAN_POINT ( 'NONE',  ( 6.300000001229033586, -2.886751345948130876, 4.999999999999996447 ) ) ;
#68306 = CARTESIAN_POINT ( 'NONE',  ( 8.484601909799253346E-16, 10.32500000122903572, -25.38119784648299770 ) ) ;
#68307 = CARTESIAN_POINT ( 'NONE',  ( -2.121784821874999949, 15.73437500061451644, -33.67503911421598417 ) ) ;
#68308 = CARTESIAN_POINT ( 'NONE',  ( 5.662500001229035185, 4.330127018922192761, -2.499999999999997780 ) ) ;
#68309 = CARTESIAN_POINT ( 'NONE',  ( 8.662499999999999645, 2.886751345948129099, -4.999999999999998224 ) ) ;
#68310 = CARTESIAN_POINT ( 'NONE',  ( 3.412500001229032964, 4.330127018922192761, -2.499999999999997780 ) ) ;
#68311 = CARTESIAN_POINT ( 'NONE',  ( 11.70937500061451608, 4.541064518000418104, -2.621784821874998173 ) ) ;
#68312 = DIRECTION ( 'NONE',  ( -1.000000000000000000, -0.000000000000000000, -0.000000000000000000 ) ) ;
#68313 = CARTESIAN_POINT ( 'NONE',  ( 2.896875000614518747, -3.027376345333614438, 5.243569643749998122 ) ) ;
#68314 = CARTESIAN_POINT ( 'NONE',  ( 4.000000000000000000, 18.95000000122903216, 32.30940107675849760 ) ) ;
#68315 = CARTESIAN_POINT ( 'NONE',  ( 1.071796769724490339, 19.52990381179669654, 26.00000000000000355 ) ) ;
#68316 = CARTESIAN_POINT ( 'NONE',  ( 7.884375000614517681, -4.541064518000419881, 2.621784821874995952 ) ) ;
#68317 = CARTESIAN_POINT ( 'NONE',  ( 14.33437500061451786, 6.421520780324663323E-16, -5.243569643749999010 ) ) ;
#68318 = CARTESIAN_POINT ( 'NONE',  ( -5.810221930991193690E-16, 14.15000000122903145, -34.00000000000000000 ) ) ;
#68319 = CARTESIAN_POINT ( 'NONE',  ( 5.812500000000001776, -5.773502691896255534, -1.060575238724906372E-15 ) ) ;
#68320 = CARTESIAN_POINT ( 'NONE',  ( -4.243569643749998122, 16.69062500061459531, 32.45002607614398471 ) ) ;
#68321 = CARTESIAN_POINT ( 'NONE',  ( 20.59687500061451360, -3.027376345333610441, -5.243569643749999898 ) ) ;
#68322 = FACE_OUTER_BOUND ( 'NONE', #22895, .T. ) ;
#68323 = CARTESIAN_POINT ( 'NONE',  ( 26.88750000122903216, 4.330127018922191873, 2.499999999999999556 ) ) ;
#68324 = CARTESIAN_POINT ( 'NONE',  ( 18.72187500061451360, 5.824947211148865298E-16, -4.756430356249998326 ) ) ;
#68325 = CARTESIAN_POINT ( 'NONE',  ( 22.64062500061451644, -3.027376345333614438, 5.243569643749998122 ) ) ;
#68326 = CARTESIAN_POINT ( 'NONE',  ( 16.30312500061451786, 0.000000000000000000, 5.243569643749999010 ) ) ;
#68327 = CARTESIAN_POINT ( 'NONE',  ( 26.22187500061451360, -4.119189519843968306, 2.378215178124996054 ) ) ;
#68328 = CARTESIAN_POINT ( 'NONE',  ( 12.83437500061451786, -4.541064518000419881, 2.621784821874995952 ) ) ;
#68329 = CARTESIAN_POINT ( 'NONE',  ( 28.04999999999999716, 4.330127018922192761, -2.499999999999997780 ) ) ;
#68330 = CARTESIAN_POINT ( 'NONE',  ( 23.92500000122903359, -5.773502691896255534, -1.060575238724906372E-15 ) ) ;
#68331 = CYLINDRICAL_SURFACE ( 'NONE', #40241, 4.000000000000000000 ) ;
#68332 = CARTESIAN_POINT ( 'NONE',  ( 10.80937500061451928, 4.541064518000418104, -2.621784821874998173 ) ) ;
#68333 = CARTESIAN_POINT ( 'NONE',  ( 29.78437500061451715, 4.541064518000418104, 2.621784821874999949 ) ) ;
#68334 = CARTESIAN_POINT ( 'NONE',  ( 3.084375000614519191, 6.421520780324663323E-16, -5.243569643749999010 ) ) ;
#68335 = CARTESIAN_POINT ( 'NONE',  ( -1.071796769724491005, 11.92009619066136850, 26.00000000000000355 ) ) ;
#68336 = CARTESIAN_POINT ( 'NONE',  ( 23.40937500061451715, 4.541064518000418104, -2.621784821874998173 ) ) ;
#68337 = CARTESIAN_POINT ( 'NONE',  ( 14.40937500061451715, 4.541064518000418104, -2.621784821874998173 ) ) ;
#68338 = CARTESIAN_POINT ( 'NONE',  ( 3.756430356249998770, 17.66562499938548214, 32.16877607737302469 ) ) ;
#68339 = CARTESIAN_POINT ( 'NONE',  ( 25.08749999999999858, -2.886751345948129988, 4.999999999999997335 ) ) ;
#68340 = CARTESIAN_POINT ( 'NONE',  ( -3.756430356250001434, 20.10312499938548214, 32.16877607737301048 ) ) ;
#68341 = CARTESIAN_POINT ( 'NONE',  ( 26.70937500061451431, 0.000000000000000000, 4.756430356249998326 ) ) ;
#68342 = CARTESIAN_POINT ( 'NONE',  ( 18.02812500061451573, 4.541064518000418104, 2.621784821874999949 ) ) ;
#68343 = CARTESIAN_POINT ( 'NONE',  ( 6.825000000000001066, 6.123233995736764310E-16, -4.999999999999998224 ) ) ;
#68344 = DIRECTION ( 'NONE',  ( 0.1736464922939214561, 0.000000000000000000, 0.9848080501874549864 ) ) ;
#68345 = CARTESIAN_POINT ( 'NONE',  ( 18.14999999999999858, 4.330127018922192761, -2.499999999999997780 ) ) ;
#68346 = CARTESIAN_POINT ( 'NONE',  ( 4.243569643749999898, 12.79062500061451679, 32.45002607614398471 ) ) ;
#68347 = DIRECTION ( 'NONE',  ( -1.000000000000000000, -0.000000000000000000, -0.000000000000000000 ) ) ;
#68348 = CARTESIAN_POINT ( 'NONE',  ( 27.49687500061451217, 6.054752690667223547, 3.707466751127219781E-16 ) ) ;
#68349 = EDGE_LOOP ( 'NONE', ( #32182, #25112, #1320, #21397 ) ) ;
#68350 = CARTESIAN_POINT ( 'NONE',  ( 21.77812500061451928, -4.541064518000419881, 2.621784821874995952 ) ) ;
#68351 = CARTESIAN_POINT ( 'NONE',  ( 20.29687500061451644, 6.054752690667223547, 3.707466751127219781E-16 ) ) ;
#68352 = CARTESIAN_POINT ( 'NONE',  ( 3.337499999999999911, 5.773502691896255534, 3.535250795749688894E-16 ) ) ;
#68353 = CARTESIAN_POINT ( 'NONE',  ( 6.290625000614517681, 6.054752690667223547, 3.707466751127219781E-16 ) ) ;
#68354 = CARTESIAN_POINT ( 'NONE',  ( 24.14062500061451289, -3.027376345333610441, -5.243569643749999898 ) ) ;
#68355 = CARTESIAN_POINT ( 'NONE',  ( 11.74687500061451573, 6.054752690667223547, 3.707466751127219781E-16 ) ) ;
#68356 = CARTESIAN_POINT ( 'NONE',  ( 17.22187500061451715, 3.027376345333611329, 5.243569643749999010 ) ) ;
#68357 = CARTESIAN_POINT ( 'NONE',  ( -3.000416591977282496E-16, 17.89062500061451644, 25.09994784771203058 ) ) ;
#68358 = CARTESIAN_POINT ( 'NONE',  ( 19.20000000122903572, 5.773502691896255534, 3.535250795749688894E-16 ) ) ;
#68359 = CARTESIAN_POINT ( 'NONE',  ( 15.38437500061451679, 4.119189519843966529, 2.378215178124999607 ) ) ;
#68360 = CARTESIAN_POINT ( 'NONE',  ( 9.403125000614517504, 4.541064518000418104, -2.621784821874998173 ) ) ;
#68361 = CARTESIAN_POINT ( 'NONE',  ( 5.409375000614516260, 4.541064518000418104, -2.621784821874998173 ) ) ;
#68362 = CARTESIAN_POINT ( 'NONE',  ( 4.021875000614516082, 3.027376345333613106, -5.243569643749998122 ) ) ;
#68363 = VERTEX_POINT ( 'NONE', #3189 ) ;
#68364 = CARTESIAN_POINT ( 'NONE',  ( 24.87187500061451573, 3.027376345333611329, 5.243569643749999010 ) ) ;
#68365 = CARTESIAN_POINT ( 'NONE',  ( 17.01562500061451644, 3.027376345333613106, -5.243569643749998122 ) ) ;
#68366 = CARTESIAN_POINT ( 'NONE',  ( 26.40000000122902790, 5.773502691896255534, 3.535250795749688894E-16 ) ) ;
#68367 = EDGE_CURVE ( 'NONE', #41205, #59156, #52158, .T. ) ;
#68368 = CARTESIAN_POINT ( 'NONE',  ( 27.44062500061451715, 6.054752690667223547, 3.707466751127219781E-16 ) ) ;
#68369 = CARTESIAN_POINT ( 'NONE',  ( 22.73437500061451644, -4.541064518000419881, 2.621784821874995952 ) ) ;
#68370 = CARTESIAN_POINT ( 'NONE',  ( 16.90312500061451573, -4.541064518000417216, -2.621784821875001281 ) ) ;
#68371 = CARTESIAN_POINT ( 'NONE',  ( 2.121784821874999061, 18.80937500061451928, 26.32496088578401583 ) ) ;
#68372 = CARTESIAN_POINT ( 'NONE',  ( 23.09062500061451573, -3.027376345333614438, 5.243569643749998122 ) ) ;
#68373 = CARTESIAN_POINT ( 'NONE',  ( 2.700000001229035718, -2.886751345948129988, 4.999999999999997335 ) ) ;
#68374 = VERTEX_POINT ( 'NONE', #59309 ) ;
#68375 = CARTESIAN_POINT ( 'NONE',  ( 26.77499999999999858, 4.330127018922191873, 2.499999999999999556 ) ) ;
#68376 = CARTESIAN_POINT ( 'NONE',  ( 1.999999999999998668, 12.20000000000000107, -33.46410161513775705 ) ) ;
#68377 = CARTESIAN_POINT ( 'NONE',  ( 3.756430356250000102, 18.60312499938548214, 30.00000000000000000 ) ) ;
#68378 = CARTESIAN_POINT ( 'NONE',  ( 3.496875000614518836, -3.027376345333610441, -5.243569643749999898 ) ) ;
#68379 = CARTESIAN_POINT ( 'NONE',  ( 9.103125000614515017, 0.000000000000000000, 5.243569643749999010 ) ) ;
#68380 = CARTESIAN_POINT ( 'NONE',  ( 21.93750000122903288, 4.330127018922191873, 2.499999999999999556 ) ) ;
#68381 = CARTESIAN_POINT ( 'NONE',  ( 27.36562500061451786, 3.027376345333613106, -5.243569643749998122 ) ) ;
#68382 = CARTESIAN_POINT ( 'NONE',  ( 27.63749999999999929, 5.773502691896255534, 3.535250795749688894E-16 ) ) ;
#68383 = CARTESIAN_POINT ( 'NONE',  ( 3.999999999999998668, 18.12500000122903288, -32.30940107675850470 ) ) ;
#68384 = DIRECTION ( 'NONE',  ( 0.1736464922939166267, 0.000000000000000000, 0.9848080501874559856 ) ) ;
#68385 = CARTESIAN_POINT ( 'NONE',  ( 9.778125000614517504, 6.421520780324663323E-16, -5.243569643749999010 ) ) ;
#68386 = ORIENTED_EDGE ( 'NONE', *, *, #31507, .T. ) ;
#68387 = CARTESIAN_POINT ( 'NONE',  ( 8.728125000614518569, -4.541064518000419881, 2.621784821874995952 ) ) ;
#68388 = CARTESIAN_POINT ( 'NONE',  ( 5.053125000614517859, 0.000000000000000000, 5.243569643749999010 ) ) ;
#68389 = CARTESIAN_POINT ( 'NONE',  ( 17.52187500061451431, 2.746126346562645981, -4.756430356249997438 ) ) ;
#68390 = CARTESIAN_POINT ( 'NONE',  ( 13.95000000122903394, -2.886751345948063374, 5.000000000000112799 ) ) ;
#68391 = CARTESIAN_POINT ( 'NONE',  ( 15.97499999999999964, 4.330127018922191873, 2.499999999999999556 ) ) ;
#68392 = CARTESIAN_POINT ( 'NONE',  ( 16.50937500061451502, -4.541064518000417216, -2.621784821875001281 ) ) ;
#68393 = CARTESIAN_POINT ( 'NONE',  ( 10.27500000122903323, 2.886751345948126879, 4.999999999999999112 ) ) ;
#68394 = CARTESIAN_POINT ( 'NONE',  ( 19.47187500061451360, 3.027376345333611329, 5.243569643749999010 ) ) ;
#68395 = CARTESIAN_POINT ( 'NONE',  ( 17.51249999999999929, -5.773502691896255534, -1.060575238724906372E-15 ) ) ;
#68396 = CARTESIAN_POINT ( 'NONE',  ( 20.52187500061451786, -6.054752690667223547, -1.112240025338166033E-15 ) ) ;
#68397 = CARTESIAN_POINT ( 'NONE',  ( -4.243569643749997233, 13.99062500061451786, -27.54997392385601174 ) ) ;
#68398 = CYLINDRICAL_SURFACE ( 'NONE', #24162, 4.999999999999998224 ) ;
#68399 = CARTESIAN_POINT ( 'NONE',  ( 26.55937500061451573, 2.746126346562643317, 4.756430356249998326 ) ) ;
#68400 = CARTESIAN_POINT ( 'NONE',  ( 4.000000000000000000, 13.38124999877096677, 27.69059892324149885 ) ) ;
#68401 = CARTESIAN_POINT ( 'NONE',  ( 26.12812500061451360, 4.541064518000418104, 2.621784821874999949 ) ) ;
#68402 = FACE_OUTER_BOUND ( 'NONE', #66802, .T. ) ;
#68403 = CARTESIAN_POINT ( 'NONE',  ( 27.87187500061451573, 3.027376345333613106, -5.243569643749998122 ) ) ;
#68404 = CARTESIAN_POINT ( 'NONE',  ( 23.21250000000000213, 2.886751345948126879, 4.999999999999999112 ) ) ;
#68405 = CARTESIAN_POINT ( 'NONE',  ( 5.953125000614519102, 0.000000000000000000, 5.243569643749999010 ) ) ;
#68406 = CARTESIAN_POINT ( 'NONE',  ( 26.03437500061451360, 5.492252693125287522, 3.363034840372157021E-16 ) ) ;
#68407 = CARTESIAN_POINT ( 'NONE',  ( 18.49687500061452283, 6.054752690667223547, 3.707466751127219781E-16 ) ) ;
#68408 = CARTESIAN_POINT ( 'NONE',  ( 10.69687500061451679, 4.119189519843966529, -2.378215178124998275 ) ) ;
#68409 = CARTESIAN_POINT ( 'NONE',  ( 5.278125000614516615, 6.421520780324663323E-16, -5.243569643749999010 ) ) ;
#68410 = CARTESIAN_POINT ( 'NONE',  ( 11.63437500061451857, 6.421520780324663323E-16, -5.243569643749999010 ) ) ;
#68411 = ORIENTED_EDGE ( 'NONE', *, *, #53665, .T. ) ;
#68412 = CARTESIAN_POINT ( 'NONE',  ( 19.62187500061451573, -6.054752690667223547, -1.112240025338166033E-15 ) ) ;
#68413 = DIRECTION ( 'NONE',  ( -1.000000000000000000, -0.000000000000000000, -0.000000000000000000 ) ) ;
#68414 = CARTESIAN_POINT ( 'NONE',  ( 28.68749999999999645, -2.886751345948129988, 4.999999999999997335 ) ) ;
#68415 = CARTESIAN_POINT ( 'NONE',  ( 3.787500000000002753, 5.773502691896255534, 3.535250795749688894E-16 ) ) ;
#68416 = DIRECTION ( 'NONE',  ( 0.000000000000000000, 0.000000000000000000, 1.000000000000000000 ) ) ;
#68417 = CARTESIAN_POINT ( 'NONE',  ( 10.87500000000000000, 6.123233995736764310E-16, -4.999999999999998224 ) ) ;
#68418 = VERTEX_POINT ( 'NONE', #24972 ) ;
#68419 = CARTESIAN_POINT ( 'NONE',  ( 10.87500000000000000, 6.123233995736764310E-16, -4.999999999999998224 ) ) ;
#68420 = CARTESIAN_POINT ( 'NONE',  ( 11.29687500061451644, 0.000000000000000000, 4.756430356249998326 ) ) ;
#68421 = CARTESIAN_POINT ( 'NONE',  ( 24.66562500061451502, 3.027376345333613106, -5.243569643749998122 ) ) ;
#68422 = CARTESIAN_POINT ( 'NONE',  ( 15.29999999999999893, -4.330127018922190985, -2.500000000000001332 ) ) ;
#68423 = CARTESIAN_POINT ( 'NONE',  ( 10.53750000122903252, 6.123233995736764310E-16, -4.999999999999998224 ) ) ;
#68424 = CARTESIAN_POINT ( 'NONE',  ( 10.11562500061451608, -6.054752690667223547, -1.112240025338166033E-15 ) ) ;
#68425 = CARTESIAN_POINT ( 'NONE',  ( 25.12499999999999645, -4.330127018922194537, 2.499999999999995559 ) ) ;
#68426 = CARTESIAN_POINT ( 'NONE',  ( 20.12812500061451715, 6.421520780324663323E-16, -5.243569643749999010 ) ) ;
#68427 = CARTESIAN_POINT ( 'NONE',  ( 18.67500000122903359, 2.886751345948095793, -5.000000000000055067 ) ) ;
#68428 = CARTESIAN_POINT ( 'NONE',  ( 27.93750000122903288, -4.330127018922194537, 2.499999999999995559 ) ) ;
#68429 = CARTESIAN_POINT ( 'NONE',  ( -3.756430356250000990, 16.50312499938548427, 32.16877607737301048 ) ) ;
#68430 = CARTESIAN_POINT ( 'NONE',  ( 6.637500000000001066, -2.886751345948129988, 4.999999999999997335 ) ) ;
#68431 = ORIENTED_EDGE ( 'NONE', *, *, #24642, .F. ) ;
#68432 = CARTESIAN_POINT ( 'NONE',  ( 22.64062500061451644, -3.027376345333614438, 5.243569643749998122 ) ) ;
#68433 = CARTESIAN_POINT ( 'NONE',  ( 28.52812500061451573, -4.541064518000419881, 2.621784821874995952 ) ) ;
#68434 = DIRECTION ( 'NONE',  ( 0.000000000000000000, 0.000000000000000000, 1.000000000000000000 ) ) ;
#68435 = CARTESIAN_POINT ( 'NONE',  ( 18.23437500061451999, -4.541064518000419881, 2.621784821874995952 ) ) ;
#68436 = EDGE_CURVE ( 'NONE', #24236, #20715, #47517, .T. ) ;
#68437 = CARTESIAN_POINT ( 'NONE',  ( 13.45312500061451466, 4.541064518000418104, -2.621784821874998173 ) ) ;
#68438 = CARTESIAN_POINT ( 'NONE',  ( 28.91250000122903074, -4.330127018922190985, -2.500000000000001332 ) ) ;
#68439 = CARTESIAN_POINT ( 'NONE',  ( 22.73437500061451644, -4.119189519843968306, 2.378215178124996054 ) ) ;
#68440 = CARTESIAN_POINT ( 'NONE',  ( 16.19062500061451715, 6.054752690667223547, 3.707466751127219781E-16 ) ) ;
#68441 = CYLINDRICAL_SURFACE ( 'NONE', #6743, 4.999999999999998224 ) ;
#68442 = CARTESIAN_POINT ( 'NONE',  ( 3.750000001229034652, -2.886751345948125991, -5.000000000000000000 ) ) ;
#68443 =( BOUNDED_CURVE ( )  B_SPLINE_CURVE ( 2, ( #59666, #65953, #65212, #15332, #26803, #19774, #37874, #48972, #31970 ),
 .UNSPECIFIED., .F., .F. ) 
 B_SPLINE_CURVE_WITH_KNOTS ( ( 3, 2, 2, 2, 3 ),
 ( 0.6630434782608696231, 0.6666666666666666297, 0.6739130434782608647, 0.6811594202898550998, 0.6847826086956522174 ),
 .UNSPECIFIED. ) 
 CURVE ( )  GEOMETRIC_REPRESENTATION_ITEM ( )  RATIONAL_B_SPLINE_CURVE ( ( 0.9330127018922192983, 0.9330127018922202975, 1.000000000000000000, 0.8660254037844387076, 1.000000000000000000, 0.8660254037844387076, 1.000000000000000000, 0.9330127018922182991, 0.9330127018922192983 ) ) 
 REPRESENTATION_ITEM ( '' )  );
#68444 = CARTESIAN_POINT ( 'NONE',  ( 13.88437500061451679, 6.421520780324663323E-16, -5.243569643749999010 ) ) ;
#68445 = CARTESIAN_POINT ( 'NONE',  ( 12.94687500061451857, -3.027376345333610441, -5.243569643749999898 ) ) ;
#68446 = CARTESIAN_POINT ( 'NONE',  ( 19.32187500061451857, 3.027376345333613106, -5.243569643749998122 ) ) ;
#68447 = ORIENTED_EDGE ( 'NONE', *, *, #49669, .T. ) ;
#68448 = CARTESIAN_POINT ( 'NONE',  ( -5.790145606462770544, 8.153486631126844131, 31.58542748218363982 ) ) ;
#68449 = CARTESIAN_POINT ( 'NONE',  ( 24.66562500061451502, 3.027376345333613106, -5.243569643749998122 ) ) ;
#68450 = CARTESIAN_POINT ( 'NONE',  ( 17.78437500061451715, -4.541064518000419881, 2.621784821874995952 ) ) ;
#68451 = CARTESIAN_POINT ( 'NONE',  ( 25.22812500061451502, 4.541064518000418104, 2.621784821874999949 ) ) ;
#68452 = CARTESIAN_POINT ( 'NONE',  ( 1.626862140677534273E-15, 12.01250000000000284, -26.00000000000000355 ) ) ;
#68453 = CARTESIAN_POINT ( 'NONE',  ( -1.999999999999997113, 17.82499999999999929, 33.46410161513775705 ) ) ;
#68454 = CARTESIAN_POINT ( 'NONE',  ( 28.49062500061451431, -3.027376345333614438, 5.243569643749998122 ) ) ;
#68455 = CARTESIAN_POINT ( 'NONE',  ( 10.01250000122903394, -4.330127018922190985, -2.500000000000001332 ) ) ;
#68456 = CARTESIAN_POINT ( 'NONE',  ( 5.962500001229033231, -4.330127018922190985, -2.500000000000001332 ) ) ;
#68457 = CARTESIAN_POINT ( 'NONE',  ( 28.76250000122903216, 0.000000000000000000, 4.999999999999998224 ) ) ;
#68458 = CARTESIAN_POINT ( 'NONE',  ( 27.82500000122903572, 2.886751345948126879, 4.999999999999999112 ) ) ;
#68459 = CARTESIAN_POINT ( 'NONE',  ( -3.999999999999999556, 18.93124999877096570, 27.69059892324149175 ) ) ;
#68460 = CARTESIAN_POINT ( 'NONE',  ( 16.18125000122903145, -4.330127018922194537, 2.499999999999995559 ) ) ;
#68461 = CARTESIAN_POINT ( 'NONE',  ( 8.671875000614518214, 3.027376345333611329, 5.243569643749999010 ) ) ;
#68462 = LINE ( 'NONE', #24468, #56173 ) ;
#68463 = CARTESIAN_POINT ( 'NONE',  ( 17.87812500061451715, 6.421520780324663323E-16, -5.243569643749999010 ) ) ;
#68464 = CARTESIAN_POINT ( 'NONE',  ( 11.82187500061451679, 3.027376345333611329, 5.243569643749999010 ) ) ;
#68465 = CARTESIAN_POINT ( 'NONE',  ( 3.703125000614516882, 0.000000000000000000, 5.243569643749999010 ) ) ;
#68466 = CARTESIAN_POINT ( 'NONE',  ( 19.47187500061451360, 3.027376345333611329, 5.243569643749999010 ) ) ;
#68467 = CARTESIAN_POINT ( 'NONE',  ( 6.384375000614516793, 4.541064518000418104, 2.621784821874999949 ) ) ;
#68468 = CARTESIAN_POINT ( 'NONE',  ( 4.000000000000000000, 12.89374999877096606, 30.00000000000000000 ) ) ;
#68469 = DIRECTION ( 'NONE',  ( 0.000000000000000000, 0.000000000000000000, -1.000000000000000000 ) ) ;
#68470 = CARTESIAN_POINT ( 'NONE',  ( 7.078125000614516438, 6.421520780324663323E-16, -5.243569643749999010 ) ) ;
#68471 = CARTESIAN_POINT ( 'NONE',  ( 20.95312500061451999, -4.541064518000417216, -2.621784821875001281 ) ) ;
#68472 = VERTEX_POINT ( 'NONE', #70046 ) ;
#68473 = CARTESIAN_POINT ( 'NONE',  ( 5.662500001229035185, 4.330127018922192761, -2.499999999999997780 ) ) ;
#68474 = CARTESIAN_POINT ( 'NONE',  ( 14.61562500061451608, -6.054752690667223547, -1.112240025338166033E-15 ) ) ;
#68475 = CARTESIAN_POINT ( 'NONE',  ( 13.30312500061451786, -4.541064518000417216, -2.621784821875001281 ) ) ;
#68476 = CARTESIAN_POINT ( 'NONE',  ( 24.27187500061452141, 2.746126346562645981, -4.756430356249997438 ) ) ;
#68477 = CARTESIAN_POINT ( 'NONE',  ( 13.61250000000000071, 2.886751345948129099, -4.999999999999998224 ) ) ;
#68478 = CARTESIAN_POINT ( 'NONE',  ( 9.675000001229035362, 2.886751345948129099, -4.999999999999998224 ) ) ;
#68479 = CARTESIAN_POINT ( 'NONE',  ( 5.953125000614519102, 0.000000000000000000, 5.243569643749999010 ) ) ;
#68480 = CARTESIAN_POINT ( 'NONE',  ( 18.71250000122903145, 4.330127018922192761, -2.499999999999997780 ) ) ;
#68481 = CARTESIAN_POINT ( 'NONE',  ( 23.66250000000000142, 2.886751345948126879, 4.999999999999999112 ) ) ;
#68482 = CARTESIAN_POINT ( 'NONE',  ( 9.001249775931846008E-16, 10.97187500061451715, -25.09994784771203058 ) ) ;
#68483 = DIRECTION ( 'NONE',  ( 0.000000000000000000, 0.000000000000000000, -1.000000000000000000 ) ) ;
#68484 = CARTESIAN_POINT ( 'NONE',  ( 3.937500001229034208, 4.330127018922191873, 2.499999999999999556 ) ) ;
#68485 =( BOUNDED_CURVE ( )  B_SPLINE_CURVE ( 2, ( #72875, #51064, #45531, #27816, #10451, #17068, #56950 ),
 .UNSPECIFIED., .F., .F. ) 
 B_SPLINE_CURVE_WITH_KNOTS ( ( 3, 2, 2, 3 ),
 ( 0.5100000000000000089, 0.5133333333333333082, 0.5166666666666667185, 0.5200000000000000178 ),
 .UNSPECIFIED. ) 
 CURVE ( )  GEOMETRIC_REPRESENTATION_ITEM ( )  RATIONAL_B_SPLINE_CURVE ( ( 1.000000000000000000, 0.8660254037844387076, 1.000000000000000000, 0.8660254037844387076, 1.000000000000000000, 0.8660254037844387076, 1.000000000000000000 ) ) 
 REPRESENTATION_ITEM ( '' )  );
#68486 = CARTESIAN_POINT ( 'NONE',  ( -1.243387493232115393E-14, 14.86250000000000071, 26.00000000000000000 ) ) ;
#68487 = CARTESIAN_POINT ( 'NONE',  ( -2.000000000000000000, 13.17500000000000071, 26.53589838486224650 ) ) ;
#68488 = CARTESIAN_POINT ( 'NONE',  ( 17.85937500061451999, -4.541064518000417216, -2.621784821875001281 ) ) ;
#68489 = CARTESIAN_POINT ( 'NONE',  ( -5.810221930991193690E-16, 13.70000000122903394, 26.00000000000000355 ) ) ;
#68490 = EDGE_CURVE ( 'NONE', #5287, #13883, #1793, .T. ) ;
#68491 = CARTESIAN_POINT ( 'NONE',  ( 12.92812500061451786, 6.421520780324663323E-16, -5.243569643749999010 ) ) ;
#68492 = CARTESIAN_POINT ( 'NONE',  ( 10.33125000122903359, -4.330127018922194537, 2.499999999999995559 ) ) ;
#68493 = CARTESIAN_POINT ( 'NONE',  ( 22.61250000122903003, -4.330127018922190985, -2.500000000000001332 ) ) ;
#68494 = CARTESIAN_POINT ( 'NONE',  ( 29.82187500061451502, 3.027376345333611329, 5.243569643749999010 ) ) ;
#68495 = CARTESIAN_POINT ( 'NONE',  ( 26.85937500061451644, -4.541064518000417216, -2.621784821875001281 ) ) ;
#68496 = CARTESIAN_POINT ( 'NONE',  ( 17.82187500061451502, 5.824947211148865298E-16, -4.756430356249998326 ) ) ;
#68497 = CARTESIAN_POINT ( 'NONE',  ( 12.74062500061451786, -3.027376345333614438, 5.243569643749998122 ) ) ;
#68498 = CARTESIAN_POINT ( 'NONE',  ( 9.871875000614517504, 3.027376345333613106, -5.243569643749998122 ) ) ;
#68499 = ORIENTED_EDGE ( 'NONE', *, *, #57822, .F. ) ;
#68500 = CARTESIAN_POINT ( 'NONE',  ( 29.46562500061451573, -6.054752690667223547, -1.112240025338166033E-15 ) ) ;
#68501 = CARTESIAN_POINT ( 'NONE',  ( 20.87812500061451715, -4.541064518000419881, 2.621784821874995952 ) ) ;
#68502 = FACE_OUTER_BOUND ( 'NONE', #46337, .T. ) ;
#68503 = EDGE_CURVE ( 'NONE', #41603, #44765, #59683, .T. ) ;
#68504 = CARTESIAN_POINT ( 'NONE',  ( 1.071796769724491893, 15.29509619066137027, -26.00000000000000355 ) ) ;
#68505 = CARTESIAN_POINT ( 'NONE',  ( 10.23750000000000071, -2.886751345948129988, 4.999999999999997335 ) ) ;
#68506 = CARTESIAN_POINT ( 'NONE',  ( 22.53750000122903430, -4.330127018922194537, 2.499999999999995559 ) ) ;
#68507 = CARTESIAN_POINT ( 'NONE',  ( 16.64062500061451289, 6.054752690667223547, 3.707466751127219781E-16 ) ) ;
#68508 = CARTESIAN_POINT ( 'NONE',  ( 11.18437500061451573, 5.492252693125287522, 3.363034840372157021E-16 ) ) ;
#68509 = ORIENTED_EDGE ( 'NONE', *, *, #39611, .T. ) ;
#68510 = CARTESIAN_POINT ( 'NONE',  ( 18.56250000000000000, 2.886751345948129099, -4.999999999999998224 ) ) ;
#68511 = EDGE_CURVE ( 'NONE', #55166, #19228, #7332, .T. ) ;
#68512 = CARTESIAN_POINT ( 'NONE',  ( 21.03750000000000142, -2.886751345948129988, 4.999999999999997335 ) ) ;
#68513 = CARTESIAN_POINT ( 'NONE',  ( 19.43437500061451928, 4.541064518000418104, 2.621784821874999949 ) ) ;
#68514 = CARTESIAN_POINT ( 'NONE',  ( 25.67812500061451431, 4.541064518000418104, 2.621784821874999949 ) ) ;
#68515 =( BOUNDED_CURVE ( )  B_SPLINE_CURVE ( 2, ( #9589, #37657, #2951, #42843, #8856, #25479, #71279 ),
 .UNSPECIFIED., .F., .F. ) 
 B_SPLINE_CURVE_WITH_KNOTS ( ( 3, 2, 2, 3 ),
 ( 0.6083333333333332815, 0.6111111111111111605, 0.6138888888888889284, 0.6166666666666666963 ),
 .UNSPECIFIED. ) 
 CURVE ( )  GEOMETRIC_REPRESENTATION_ITEM ( )  RATIONAL_B_SPLINE_CURVE ( ( 1.000000000000000000, 0.8660254037844387076, 1.000000000000000000, 0.8660254037844387076, 1.000000000000000000, 0.8660254037844387076, 1.000000000000000000 ) ) 
 REPRESENTATION_ITEM ( '' )  );
#68516 = VERTEX_POINT ( 'NONE', #42707 ) ;
#68517 = CARTESIAN_POINT ( 'NONE',  ( 8.812500001229034652, 4.330127018922192761, -2.499999999999997780 ) ) ;
#68518 = CARTESIAN_POINT ( 'NONE',  ( 9.253125000614517148, -4.541064518000417216, -2.621784821875001281 ) ) ;
#68519 = CARTESIAN_POINT ( 'NONE',  ( 2.393811435568372112E-14, 19.08124999877097139, 34.00000000000000000 ) ) ;
#68520 = CARTESIAN_POINT ( 'NONE',  ( 15.82499999999999929, 6.123233995736764310E-16, -4.999999999999998224 ) ) ;
#68521 = CARTESIAN_POINT ( 'NONE',  ( 4.243569643749999010, 18.71562500061451217, 27.54997392385601174 ) ) ;
#68522 = CARTESIAN_POINT ( 'NONE',  ( 27.96562500061451928, 3.027376345333611329, 5.243569643749999010 ) ) ;
#68523 = CARTESIAN_POINT ( 'NONE',  ( 10.27499999999999858, -4.330127018922194537, 2.499999999999995559 ) ) ;
#68524 = CARTESIAN_POINT ( 'NONE',  ( -1.878215178124999163, 15.04062499938548392, 26.74683588394047007 ) ) ;
#68525 = CARTESIAN_POINT ( 'NONE',  ( 25.65937500061451715, 4.541064518000418104, -2.621784821874998173 ) ) ;
#68526 = VERTEX_POINT ( 'NONE', #36432 ) ;
#68527 = CARTESIAN_POINT ( 'NONE',  ( 24.85312500061451502, 0.000000000000000000, 5.243569643749999010 ) ) ;
#68528 = CARTESIAN_POINT ( 'NONE',  ( 24.60937500061451644, -4.541064518000417216, -2.621784821875001281 ) ) ;
#68529 = CARTESIAN_POINT ( 'NONE',  ( -2.121784821874996840, 18.07812500061459104, -26.32496088578401583 ) ) ;
#68530 = CARTESIAN_POINT ( 'NONE',  ( 11.92500000000000071, 4.330127018922191873, 2.499999999999999556 ) ) ;
#68531 = CARTESIAN_POINT ( 'NONE',  ( 8.915625000614515017, 3.027376345333613106, -5.243569643749998122 ) ) ;
#68532 = CARTESIAN_POINT ( 'NONE',  ( 28.43437500061451573, 4.119189519843966529, 2.378215178124999607 ) ) ;
#68533 = CARTESIAN_POINT ( 'NONE',  ( 28.41562500061451502, 3.027376345333611329, 5.243569643749999010 ) ) ;
#68534 = CARTESIAN_POINT ( 'NONE',  ( 27.47812500061451502, 4.541064518000418104, 2.621784821874999949 ) ) ;
#68535 = CARTESIAN_POINT ( 'NONE',  ( 28.80937500061451217, 2.746126346562643317, 4.756430356249998326 ) ) ;
#68536 = CARTESIAN_POINT ( 'NONE',  ( 12.79687500061451821, -2.746126346562646425, 4.756430356249996549 ) ) ;
#68537 = CARTESIAN_POINT ( 'NONE',  ( 20.10937500061451289, -4.541064518000417216, -2.621784821875001281 ) ) ;
#68538 = CARTESIAN_POINT ( 'NONE',  ( -2.121784821874996840, 12.73437500061451821, 33.67503911421598417 ) ) ;
#68539 = CARTESIAN_POINT ( 'NONE',  ( 19.80937500061451573, 4.541064518000418104, -2.621784821874998173 ) ) ;
#68540 = CARTESIAN_POINT ( 'NONE',  ( 27.68437500061451573, -4.541064518000419881, 2.621784821874995952 ) ) ;
#68541 = CARTESIAN_POINT ( 'NONE',  ( 2.121784821874999061, 16.10937500061451644, 26.32496088578401583 ) ) ;
#68542 = CARTESIAN_POINT ( 'NONE',  ( 8.465625000614515727, 3.027376345333613106, -5.243569643749998122 ) ) ;
#68543 = CARTESIAN_POINT ( 'NONE',  ( 2.000000000000001332, 10.36250000122903359, -26.53589838486224650 ) ) ;
#68544 = CARTESIAN_POINT ( 'NONE',  ( 5.484375000614518214, 4.541064518000418104, 2.621784821874999949 ) ) ;
#68545 = CARTESIAN_POINT ( 'NONE',  ( 11.79375000122903039, -2.886751345948181946, -4.999999999999904077 ) ) ;
#68546 =( BOUNDED_CURVE ( )  B_SPLINE_CURVE ( 2, ( #19736, #48196, #32665, #37473, #65175, #43391, #15295 ),
 .UNSPECIFIED., .F., .F. ) 
 B_SPLINE_CURVE_WITH_KNOTS ( ( 3, 2, 2, 3 ),
 ( 0.3599999999999999867, 0.3633333333333333415, 0.3666666666666666408, 0.3699999999999999956 ),
 .UNSPECIFIED. ) 
 CURVE ( )  GEOMETRIC_REPRESENTATION_ITEM ( )  RATIONAL_B_SPLINE_CURVE ( ( 1.000000000000000000, 0.8660254037844387076, 1.000000000000000000, 0.8660254037844387076, 1.000000000000000000, 0.8660254037844387076, 1.000000000000000000 ) ) 
 REPRESENTATION_ITEM ( '' )  );
#68547 = CARTESIAN_POINT ( 'NONE',  ( 4.828125000614518214, 6.421520780324663323E-16, -5.243569643749999010 ) ) ;
#68548 = CARTESIAN_POINT ( 'NONE',  ( 9.871875000614517504, 3.027376345333613106, -5.243569643749998122 ) ) ;
#68549 = SURFACE_STYLE_FILL_AREA ( #34549 ) ;
#68550 = CARTESIAN_POINT ( 'NONE',  ( 18.00000000122903288, -2.886751345948129988, 4.999999999999997335 ) ) ;
#68551 = CARTESIAN_POINT ( 'NONE',  ( 5.709375000614517859, -4.541064518000417216, -2.621784821875001281 ) ) ;
#68552 = CARTESIAN_POINT ( 'NONE',  ( 7.115625000614516082, 3.027376345333613106, -5.243569643749998122 ) ) ;
#68553 = CARTESIAN_POINT ( 'NONE',  ( 4.196151849995945149, -2.718880220196457476, -4.196151849995952254 ) ) ;
#68554 = CARTESIAN_POINT ( 'NONE',  ( 24.05625000122903145, 4.330127018922192761, -2.499999999999997780 ) ) ;
#68555 = CARTESIAN_POINT ( 'NONE',  ( 16.84687500061451715, -3.027376345333614438, 5.243569643749998122 ) ) ;
#68556 = ORIENTED_EDGE ( 'NONE', *, *, #32955, .F. ) ;
#68557 = CARTESIAN_POINT ( 'NONE',  ( 25.04062500061451502, -3.027376345333610441, -5.243569643749999898 ) ) ;
#68558 = CARTESIAN_POINT ( 'NONE',  ( 9.215625000614515727, -6.054752690667223547, -1.112240025338166033E-15 ) ) ;
#68559 = EDGE_CURVE ( 'NONE', #46076, #41970, #59362, .T. ) ;
#68560 = CARTESIAN_POINT ( 'NONE',  ( 27.68437500061451573, -4.541064518000419881, 2.621784821874995952 ) ) ;
#68561 = CARTESIAN_POINT ( 'NONE',  ( 9.703125000614514661, -4.541064518000417216, -2.621784821875001281 ) ) ;
#68562 = CARTESIAN_POINT ( 'NONE',  ( -4.243569643749999898, 10.85937500061451821, -30.00000000000000000 ) ) ;
#68563 = CARTESIAN_POINT ( 'NONE',  ( 12.56250000122903465, 0.000000000000000000, 4.999999999999998224 ) ) ;
#68564 = CARTESIAN_POINT ( 'NONE',  ( 26.54062500061451146, 6.054752690667223547, 3.707466751127219781E-16 ) ) ;
#68565 = CARTESIAN_POINT ( 'NONE',  ( 2.121784821874999061, 13.35312500061451679, -33.67503911421598417 ) ) ;
#68566 = CARTESIAN_POINT ( 'NONE',  ( 12.75000000122903643, -2.886751345948125991, -5.000000000000000000 ) ) ;
#68567 = CARTESIAN_POINT ( 'NONE',  ( 10.95000000000000107, 4.330127018922192761, -2.499999999999997780 ) ) ;
#68568 = CARTESIAN_POINT ( 'NONE',  ( 21.47812500061451502, 6.421520780324663323E-16, -5.243569643749999010 ) ) ;
#68569 = CARTESIAN_POINT ( 'NONE',  ( 5.259375000614518569, -4.541064518000417216, -2.621784821875001281 ) ) ;
#68570 = CARTESIAN_POINT ( 'NONE',  ( 20.47500000000000142, 4.330127018922191873, 2.499999999999999556 ) ) ;
#68571 = CARTESIAN_POINT ( 'NONE',  ( 7.837500001229035007, 6.123233995736764310E-16, -4.999999999999998224 ) ) ;
#68572 = CARTESIAN_POINT ( 'NONE',  ( 16.42500000122903359, 2.886751345948129099, -4.999999999999998224 ) ) ;
#68573 = CARTESIAN_POINT ( 'NONE',  ( 12.70312500061451821, 0.000000000000000000, 5.243569643749999010 ) ) ;
#68574 = CARTESIAN_POINT ( 'NONE',  ( 15.92812500061451608, -4.541064518000419881, 2.621784821874995952 ) ) ;
#68575 = CARTESIAN_POINT ( 'NONE',  ( 25.95000000122903216, 5.773502691896255534, 3.535250795749688894E-16 ) ) ;
#68576 = CARTESIAN_POINT ( 'NONE',  ( 21.22500000000000142, 6.123233995736764310E-16, -4.999999999999998224 ) ) ;
#68577 = CARTESIAN_POINT ( 'NONE',  ( 24.30937500061451573, 4.541064518000418104, -2.621784821874998173 ) ) ;
#68578 = CARTESIAN_POINT ( 'NONE',  ( 1.071796769724491227, 13.94240381056766509, 26.00000000000000000 ) ) ;
#68579 = CARTESIAN_POINT ( 'NONE',  ( 11.10000000122903252, 5.773502691896255534, 3.535250795749688894E-16 ) ) ;
#68580 = CARTESIAN_POINT ( 'NONE',  ( 8.521875000614516082, 3.027376345333613106, -5.243569643749998122 ) ) ;
#68581 = CARTESIAN_POINT ( 'NONE',  ( 26.55937500061451573, 4.541064518000418104, -2.621784821874998173 ) ) ;
#68582 = CARTESIAN_POINT ( 'NONE',  ( 3.421875000614516882, -6.054752690667223547, -1.112240025338166033E-15 ) ) ;
#68583 = CARTESIAN_POINT ( 'NONE',  ( 23.72812500061451502, 6.421520780324663323E-16, -5.243569643749999010 ) ) ;
#68584 = CARTESIAN_POINT ( 'NONE',  ( 26.67187500061451644, 3.027376345333611329, 5.243569643749999010 ) ) ;
#68585 = CARTESIAN_POINT ( 'NONE',  ( -7.967954043666661671E-16, 18.04062499938548214, 34.33755215474603517 ) ) ;
#68586 = CARTESIAN_POINT ( 'NONE',  ( 7.396875000614519635, -3.027376345333614438, 5.243569643749998122 ) ) ;
#68587 = CARTESIAN_POINT ( 'NONE',  ( 18.81562500061452070, 3.027376345333613106, -5.243569643749998122 ) ) ;
#68588 = DIRECTION ( 'NONE',  ( 0.000000000000000000, 1.000000000000000000, 0.000000000000000000 ) ) ;
#68589 = CARTESIAN_POINT ( 'NONE',  ( 28.15312500061451573, -4.541064518000417216, -2.621784821875001281 ) ) ;
#68590 = CARTESIAN_POINT ( 'NONE',  ( 4.846875000614519813, -3.027376345333610441, -5.243569643749999898 ) ) ;
#68591 = AXIS2_PLACEMENT_3D ( 'NONE', #68684, #1092, #23600 ) ;
#68592 = CARTESIAN_POINT ( 'NONE',  ( 11.13750000000000107, -2.886751345948130876, 4.999999999999996447 ) ) ;
#68593 = CARTESIAN_POINT ( 'NONE',  ( 17.77499999999999858, 4.330127018922191873, 2.499999999999999556 ) ) ;
#68594 = ORIENTED_EDGE ( 'NONE', *, *, #15556, .T. ) ;
#68595 = CARTESIAN_POINT ( 'NONE',  ( 24.71250000000000213, -5.773502691896255534, -1.060575238724906372E-15 ) ) ;
#68596 = EDGE_CURVE ( 'NONE', #37144, #41179, #39116, .T. ) ;
#68597 = EDGE_CURVE ( 'NONE', #39309, #26767, #39208, .T. ) ;
#68598 = CARTESIAN_POINT ( 'NONE',  ( 27.04687500061451644, 6.054752690667223547, 3.707466751127219781E-16 ) ) ;
#68599 = ORIENTED_EDGE ( 'NONE', *, *, #10213, .F. ) ;
#68600 = CARTESIAN_POINT ( 'NONE',  ( 14.95312500061451644, 0.000000000000000000, 5.243569643749999010 ) ) ;
#68601 = CARTESIAN_POINT ( 'NONE',  ( 6.965625000614518392, -6.054752690667223547, -1.112240025338166033E-15 ) ) ;
#68602 = CARTESIAN_POINT ( 'NONE',  ( 19.47187500061451360, -4.119189519843968306, 2.378215178124996054 ) ) ;
#68603 = CARTESIAN_POINT ( 'NONE',  ( 5.521875000614517859, 3.027376345333611329, 5.243569643749999010 ) ) ;
#68604 = CARTESIAN_POINT ( 'NONE',  ( 14.40000000122903323, -2.886751345948129988, 4.999999999999997335 ) ) ;
#68605 = CARTESIAN_POINT ( 'NONE',  ( 22.16250000000000142, 2.886751345948129099, -4.999999999999998224 ) ) ;
#68606 = CARTESIAN_POINT ( 'NONE',  ( 29.28749999999999787, -2.886751345948125991, -5.000000000000000000 ) ) ;
#68607 = CARTESIAN_POINT ( 'NONE',  ( 4.921875000614518214, 3.027376345333613106, -5.243569643749998122 ) ) ;
#68608 = CARTESIAN_POINT ( 'NONE',  ( 8.334375000614516082, -4.541064518000419881, 2.621784821874995952 ) ) ;
#68609 = CARTESIAN_POINT ( 'NONE',  ( 20.85937500061451644, 0.000000000000000000, 5.243569643749999010 ) ) ;
#68610 = CYLINDRICAL_SURFACE ( 'NONE', #71382, 4.999999999999998224 ) ;
#68611 = ORIENTED_EDGE ( 'NONE', *, *, #44097, .F. ) ;
#68612 = CARTESIAN_POINT ( 'NONE',  ( 5.109375000614518214, 0.000000000000000000, 5.243569643749999010 ) ) ;
#68613 = CARTESIAN_POINT ( 'NONE',  ( 5.250000000000000888, 0.000000000000000000, 4.999999999999998224 ) ) ;
#68614 = CARTESIAN_POINT ( 'NONE',  ( 6.159375000614517148, -4.541064518000417216, -2.621784821875001281 ) ) ;
#68615 = CARTESIAN_POINT ( 'NONE',  ( 19.50000000000000000, 4.330127018922192761, -2.499999999999997780 ) ) ;
#68616 = CARTESIAN_POINT ( 'NONE',  ( 15.55312500061451608, -4.541064518000417216, -2.621784821875001281 ) ) ;
#68617 = CARTESIAN_POINT ( 'NONE',  ( 4.000000000000000000, 18.80000000000000071, 30.00000000000000000 ) ) ;
#68619 = CARTESIAN_POINT ( 'NONE',  ( -1.071796769724490561, 19.90759618943233278, 26.00000000000000000 ) ) ;
#68618 = VECTOR ( 'NONE', #53453, 1000.000000000000000 ) ;
#68620 = CARTESIAN_POINT ( 'NONE',  ( 20.33437500061451786, 4.119189519843966529, 2.378215178124999607 ) ) ;
#68621 = CARTESIAN_POINT ( 'NONE',  ( 10.49062500061451431, -3.027376345333614438, 5.243569643749998122 ) ) ;
#68622 = CARTESIAN_POINT ( 'NONE',  ( 27.34687500061451360, -3.027376345333610441, -5.243569643749999898 ) ) ;
#68623 = CARTESIAN_POINT ( 'NONE',  ( 12.33750000122903145, 6.123233995736764310E-16, -4.999999999999998224 ) ) ;
#68624 = CARTESIAN_POINT ( 'NONE',  ( 25.92187500061451999, -6.054752690667223547, -1.112240025338166033E-15 ) ) ;
#68625 = CARTESIAN_POINT ( 'NONE',  ( 7.762500000000001954, 2.886751345948129099, -4.999999999999998224 ) ) ;
#68626 = CARTESIAN_POINT ( 'NONE',  ( -2.828200636599751609E-16, 13.25000000122903288, 25.38119784648299770 ) ) ;
#68627 = CARTESIAN_POINT ( 'NONE',  ( 15.14062500061451644, -3.027376345333610441, -5.243569643749999898 ) ) ;
#68628 = CARTESIAN_POINT ( 'NONE',  ( 7.537500001229033408, 4.330127018922191873, 2.499999999999999556 ) ) ;
#68629 = CARTESIAN_POINT ( 'NONE',  ( 18.30937500061451928, -4.541064518000417216, -2.621784821875001281 ) ) ;
#68630 = CARTESIAN_POINT ( 'NONE',  ( 11.89687500061451608, -3.027376345333614438, 5.243569643749998122 ) ) ;
#68631 = CARTESIAN_POINT ( 'NONE',  ( 45.00000000000000000, 0.000000000000000000, 0.000000000000000000 ) ) ;
#68632 = VERTEX_POINT ( 'NONE', #61514 ) ;
#68633 = CARTESIAN_POINT ( 'NONE',  ( 11.65312500061451573, 4.541064518000418104, -2.621784821874998173 ) ) ;
#68634 = CARTESIAN_POINT ( 'NONE',  ( 26.58750000122903145, -4.330127018922194537, 2.499999999999995559 ) ) ;
#68635 = CARTESIAN_POINT ( 'NONE',  ( 12.38437500061451857, -4.541064518000419881, 2.621784821874995952 ) ) ;
#68636 = CARTESIAN_POINT ( 'NONE',  ( 4.169580978743460342, 2.759455464706926708, 4.458747374224691029 ) ) ;
#68637 = CARTESIAN_POINT ( 'NONE',  ( 13.94062500061451892, 6.054752690667223547, 3.707466751127219781E-16 ) ) ;
#68638 = DIRECTION ( 'NONE',  ( -1.000000000000000000, -0.000000000000000000, -0.000000000000000000 ) ) ;
#68639 = CARTESIAN_POINT ( 'NONE',  ( 23.22187500061451715, -6.054752690667223547, -1.112240025338166033E-15 ) ) ;
#68640 = CARTESIAN_POINT ( 'NONE',  ( 2.867942972713479755, -4.095717654485441450, 3.274159358307527690 ) ) ;
#68641 = CARTESIAN_POINT ( 'NONE',  ( 12.75000000122903643, -2.886751345948125991, -5.000000000000000000 ) ) ;
#68642 = CYLINDRICAL_SURFACE ( 'NONE', #57514, 4.999999999999998224 ) ;
#68643 = CARTESIAN_POINT ( 'NONE',  ( 3.193447721043152665, 3.847322660365763536, 3.562742055761627835 ) ) ;
#68644 = CARTESIAN_POINT ( 'NONE',  ( 4.243569643749999010, 16.97187500061451715, -32.45002607614398471 ) ) ;
#68645 = CARTESIAN_POINT ( 'NONE',  ( 17.93437500061451928, 6.421520780324663323E-16, -5.243569643749999010 ) ) ;
#68646 = CARTESIAN_POINT ( 'NONE',  ( 19.12500000122903288, 2.886751345948129099, -4.999999999999998224 ) ) ;
#68647 = CARTESIAN_POINT ( 'NONE',  ( 14.29687500061451821, -3.027376345333610441, -5.243569643749999898 ) ) ;
#68648 = CARTESIAN_POINT ( 'NONE',  ( -2.121784821874996840, 10.03437500061451892, 33.67503911421598417 ) ) ;
#68649 = CARTESIAN_POINT ( 'NONE',  ( 20.32500000122903572, -5.773502691896255534, -1.060575238724906372E-15 ) ) ;
#68650 = CARTESIAN_POINT ( 'NONE',  ( 15.17812500061451608, 6.421520780324663323E-16, -5.243569643749999010 ) ) ;
#68651 = FACE_OUTER_BOUND ( 'NONE', #19362, .T. ) ;
#68652 = ORIENTED_EDGE ( 'NONE', *, *, #63249, .T. ) ;
#68653 = ORIENTED_EDGE ( 'NONE', *, *, #61021, .T. ) ;
#68654 = CARTESIAN_POINT ( 'NONE',  ( 17.84999999999999787, 0.000000000000000000, 4.999999999999998224 ) ) ;
#68655 = CARTESIAN_POINT ( 'NONE',  ( 4.115625000614516082, 3.027376345333611329, 5.243569643749999010 ) ) ;
#68656 = EDGE_CURVE ( 'NONE', #45391, #6802, #66711, .T. ) ;
#68657 = CARTESIAN_POINT ( 'NONE',  ( 15.33750000122903323, -4.330127018922194537, 2.499999999999995559 ) ) ;
#68658 = CARTESIAN_POINT ( 'NONE',  ( 26.44687500061451502, -3.027376345333610441, -5.243569643749999898 ) ) ;
#68659 = CARTESIAN_POINT ( 'NONE',  ( 20.27812500061451573, 4.541064518000418104, 2.621784821874999949 ) ) ;
#68660 = CARTESIAN_POINT ( 'NONE',  ( 23.39062500061451289, 6.054752690667223547, 3.707466751127219781E-16 ) ) ;
#68661 = CARTESIAN_POINT ( 'NONE',  ( 3.778125000614519280, -4.541064518000419881, 2.621784821874995952 ) ) ;
#68662 = B_SPLINE_CURVE_WITH_KNOTS ( 'NONE', 1,
 ( #8006, #33989 ),
 .UNSPECIFIED., .F., .F.,
 ( 2, 2 ),
 ( 0.000000000000000000, 1.000000000000000000 ),
 .UNSPECIFIED. ) ;
#68663 = CARTESIAN_POINT ( 'NONE',  ( 28.12499999999999645, 4.330127018922191873, 2.499999999999999556 ) ) ;
#68664 = CARTESIAN_POINT ( 'NONE',  ( 4.724999999999999645, 4.330127018922191873, 2.499999999999999556 ) ) ;
#68665 = CARTESIAN_POINT ( 'NONE',  ( 8.559375000614515727, 4.119189519843966529, -2.378215178124998275 ) ) ;
#68666 = CARTESIAN_POINT ( 'NONE',  ( 6.337500001229033231, -4.330127018922194537, 2.499999999999995559 ) ) ;
#68667 = CARTESIAN_POINT ( 'NONE',  ( 28.80000000000000071, -4.330127018922190985, -2.500000000000001332 ) ) ;
#68668 = CARTESIAN_POINT ( 'NONE',  ( -4.243569643749999898, 17.12187500061451573, -32.45002607614398471 ) ) ;
#68669 = CARTESIAN_POINT ( 'NONE',  ( 5.025000001229035895, -5.773502691896255534, -1.060575238724906372E-15 ) ) ;
#68670 = CARTESIAN_POINT ( 'NONE',  ( 4.762499999999999289, 2.886751345948126879, 4.999999999999999112 ) ) ;
#68671 =( BOUNDED_CURVE ( )  B_SPLINE_CURVE ( 2, ( #28417, #5528, #11063, #33589, #56842, #16236, #11792 ),
 .UNSPECIFIED., .F., .F. ) 
 B_SPLINE_CURVE_WITH_KNOTS ( ( 3, 2, 2, 3 ),
 ( 0.7900000000000001465, 0.7933333333333334458, 0.7966666666666666341, 0.8000000000000000444 ),
 .UNSPECIFIED. ) 
 CURVE ( )  GEOMETRIC_REPRESENTATION_ITEM ( )  RATIONAL_B_SPLINE_CURVE ( ( 0.9999999999999955591, 0.8660254037844431485, 1.000000000000000000, 0.8660254037844387076, 1.000000000000000000, 0.8660254037844387076, 1.000000000000000000 ) ) 
 REPRESENTATION_ITEM ( '' )  );
#68672 = CARTESIAN_POINT ( 'NONE',  ( 3.225000001229033408, -5.773502691896255534, -1.060575238724906372E-15 ) ) ;
#68673 = CARTESIAN_POINT ( 'NONE',  ( 9.946875000614516793, 6.054752690667223547, 3.707466751127219781E-16 ) ) ;
#68674 = AXIS2_PLACEMENT_3D ( 'NONE', #21209, #44131, #50402 ) ;
#68675 = CARTESIAN_POINT ( 'NONE',  ( 4.000000000000000000, 16.70000000122903216, -27.69059892324149885 ) ) ;
#68676 = CYLINDRICAL_SURFACE ( 'NONE', #38967, 4.999999999999998224 ) ;
#68677 = CARTESIAN_POINT ( 'NONE',  ( 5.512500001229033941, -4.330127018922190985, -2.500000000000001332 ) ) ;
#68678 = CYLINDRICAL_SURFACE ( 'NONE', #47749, 4.999999999999998224 ) ;
#68679 = CARTESIAN_POINT ( 'NONE',  ( 6.646875000614518747, -3.027376345333610441, -5.243569643749999898 ) ) ;
#68680 = CARTESIAN_POINT ( 'NONE',  ( 13.20937500061451786, 0.000000000000000000, 5.243569643749999010 ) ) ;
#68681 = CARTESIAN_POINT ( 'NONE',  ( 7.012500000000001066, 2.886751345948126879, 4.999999999999999112 ) ) ;
#68682 = CARTESIAN_POINT ( 'NONE',  ( 4.243569643749999898, 17.32812500061459104, 30.00000000000000000 ) ) ;
#68683 = CARTESIAN_POINT ( 'NONE',  ( 21.23437500061451644, 4.541064518000418104, 2.621784821874999949 ) ) ;
#68684 = CARTESIAN_POINT ( 'NONE',  ( 0.000000000000000000, 20.00000000000000000, -30.00000000000000000 ) ) ;
#68685 = ADVANCED_FACE ( 'NONE', ( #72612 ), #72246, .T. ) ;
#68686 = CARTESIAN_POINT ( 'NONE',  ( 27.67500000122903359, 2.886751345948129099, -4.999999999999998224 ) ) ;
#68687 = CARTESIAN_POINT ( 'NONE',  ( 18.83437500061451786, 5.492252693125287522, 3.363034840372157021E-16 ) ) ;
#68688 = CARTESIAN_POINT ( 'NONE',  ( 21.66562500061451502, 3.027376345333611329, 5.243569643749999010 ) ) ;
#68689 = CARTESIAN_POINT ( 'NONE',  ( 13.41562500061451502, 3.027376345333613106, -5.243569643749998122 ) ) ;
#68690 = CARTESIAN_POINT ( 'NONE',  ( 25.80937500061451217, -5.492252693125287522, -1.008910452111647106E-15 ) ) ;
#68691 = CARTESIAN_POINT ( 'NONE',  ( 11.07187500061451679, -6.054752690667223547, -1.112240025338166033E-15 ) ) ;
#68692 = CARTESIAN_POINT ( 'NONE',  ( 29.06250000000000000, 2.886751345948126879, 4.999999999999999112 ) ) ;
#68693 = CARTESIAN_POINT ( 'NONE',  ( 22.12500000122903288, -5.773502691896255534, -1.060575238724906372E-15 ) ) ;
#68694 = CYLINDRICAL_SURFACE ( 'NONE', #62654, 4.000000000000000000 ) ;
#68695 = CARTESIAN_POINT ( 'NONE',  ( 11.63437500061451857, 6.421520780324663323E-16, -5.243569643749999010 ) ) ;
#68696 = CARTESIAN_POINT ( 'NONE',  ( 28.13437500061451502, -4.541064518000419881, 2.621784821874995952 ) ) ;
#68697 = LINE ( 'NONE', #40255, #57215 ) ;
#68698 = CARTESIAN_POINT ( 'NONE',  ( 27.80625000122903145, 0.000000000000000000, 4.999999999999998224 ) ) ;
#68699 = CARTESIAN_POINT ( 'NONE',  ( 21.87187500061451573, -6.054752690667223547, -1.112240025338166033E-15 ) ) ;
#68700 = CARTESIAN_POINT ( 'NONE',  ( 14.70937500061451786, -4.541064518000417216, -2.621784821875001281 ) ) ;
#68701 = CARTESIAN_POINT ( 'NONE',  ( -3.756430356249999214, 17.89062499938548356, 27.83122392262697531 ) ) ;
#68702 = CARTESIAN_POINT ( 'NONE',  ( 25.83749999999999858, 5.773502691896255534, 3.535250795749688894E-16 ) ) ;
#68703 = CARTESIAN_POINT ( 'NONE',  ( -4.000000000000000000, 13.62500000000000000, 30.00000000000000000 ) ) ;
#68704 = CARTESIAN_POINT ( 'NONE',  ( 26.48437500061451644, 5.824947211148865298E-16, -4.756430356249998326 ) ) ;
#68705 = CARTESIAN_POINT ( 'NONE',  ( 18.40312500061451573, 4.541064518000418104, -2.621784821874998173 ) ) ;
#68706 = CARTESIAN_POINT ( 'NONE',  ( 6.787500000000001421, -2.886751345948125991, -5.000000000000000000 ) ) ;
#68707 = CARTESIAN_POINT ( 'NONE',  ( -0.7368881354385758975, 9.803648613939515144, 25.82089971438751519 ) ) ;
#68708 = CARTESIAN_POINT ( 'NONE',  ( 14.24999999999999822, 0.000000000000000000, 4.999999999999998224 ) ) ;
#68709 = CARTESIAN_POINT ( 'NONE',  ( 4.243569643749999898, 10.57812500061451821, 30.00000000000000000 ) ) ;
#68710 = DIRECTION ( 'NONE',  ( -1.000000000000000000, -0.000000000000000000, -0.000000000000000000 ) ) ;
#68711 = CARTESIAN_POINT ( 'NONE',  ( 25.50937500061451502, -4.541064518000417216, -2.621784821875001281 ) ) ;
#68712 = ORIENTED_EDGE ( 'NONE', *, *, #8736, .T. ) ;
#68713 = CARTESIAN_POINT ( 'NONE',  ( 23.16562500061451502, -6.054752690667223547, -1.112240025338166033E-15 ) ) ;
#68714 = CARTESIAN_POINT ( 'NONE',  ( 20.59687500061451360, -3.027376345333610441, -5.243569643749999898 ) ) ;
#68715 = CARTESIAN_POINT ( 'NONE',  ( 3.787500000000002753, 5.773502691896255534, 3.535250795749688894E-16 ) ) ;
#68716 = CARTESIAN_POINT ( 'NONE',  ( 7.903125000614515727, -4.541064518000417216, -2.621784821875001281 ) ) ;
#68717 = CARTESIAN_POINT ( 'NONE',  ( 21.06562500061451715, 3.027376345333613106, -5.243569643749998122 ) ) ;
#68718 = CARTESIAN_POINT ( 'NONE',  ( 13.20937500061451786, 0.000000000000000000, 5.243569643749999010 ) ) ;
#68719 = CARTESIAN_POINT ( 'NONE',  ( 16.35937500061451644, 0.000000000000000000, 5.243569643749999010 ) ) ;
#68720 = CARTESIAN_POINT ( 'NONE',  ( -4.243569643749997233, 18.49062500061451431, 32.45002607614398471 ) ) ;
#68721 = CARTESIAN_POINT ( 'NONE',  ( 19.53750000122903430, 6.123233995736764310E-16, -4.999999999999998224 ) ) ;
#68722 = CARTESIAN_POINT ( 'NONE',  ( 14.63437500061451679, -4.119189519843968306, 2.378215178124996054 ) ) ;
#68723 = CARTESIAN_POINT ( 'NONE',  ( 10.26562500061451644, 3.027376345333612662, -5.243569643749998122 ) ) ;
#68724 = CARTESIAN_POINT ( 'NONE',  ( 4.471875000614518925, 3.027376345333613106, -5.243569643749998122 ) ) ;
#68725 = CARTESIAN_POINT ( 'NONE',  ( 5.409375000614516260, 4.541064518000418104, -2.621784821874998173 ) ) ;
#68726 = CARTESIAN_POINT ( 'NONE',  ( 26.33437500061451431, -4.541064518000419881, 2.621784821874995952 ) ) ;
#68727 = CARTESIAN_POINT ( 'NONE',  ( 16.97812500061451502, 6.421520780324663323E-16, -5.243569643749999010 ) ) ;
#68728 = CARTESIAN_POINT ( 'NONE',  ( 26.25000000122903288, -2.886751345948125991, -5.000000000000000000 ) ) ;
#68729 =( BOUNDED_CURVE ( )  B_SPLINE_CURVE ( 2, ( #4897, #38512, #54769, #49237, #72126, #3808, #66215 ),
 .UNSPECIFIED., .F., .F. ) 
 B_SPLINE_CURVE_WITH_KNOTS ( ( 3, 2, 2, 3 ),
 ( 0.07000000000000000666, 0.07333333333333333370, 0.07666666666666664687, 0.07999999999999998779 ),
 .UNSPECIFIED. ) 
 CURVE ( )  GEOMETRIC_REPRESENTATION_ITEM ( )  RATIONAL_B_SPLINE_CURVE ( ( 1.000000000000000000, 0.8660254037844387076, 1.000000000000000000, 0.8660254037844387076, 1.000000000000000000, 0.8660254037844392627, 0.9999999999999994449 ) ) 
 REPRESENTATION_ITEM ( '' )  );
#68730 = CARTESIAN_POINT ( 'NONE',  ( 26.12812500061451360, 4.541064518000418104, 2.621784821874999949 ) ) ;
#68731 = AXIS2_PLACEMENT_3D ( 'NONE', #4998, #27169, #44892 ) ;
#68732 = CARTESIAN_POINT ( 'NONE',  ( 22.92187500061451644, 3.027376345333613106, -5.243569643749998122 ) ) ;
#68733 = CARTESIAN_POINT ( 'NONE',  ( 17.50312500061451715, 4.541064518000418104, -2.621784821874998173 ) ) ;
#68734 = CARTESIAN_POINT ( 'NONE',  ( 4.243569643749999010, 16.97187500061451360, 27.54997392385601174 ) ) ;
#68735 = CARTESIAN_POINT ( 'NONE',  ( 21.29062500061451502, -3.027376345333614438, 5.243569643749998122 ) ) ;
#68736 = CARTESIAN_POINT ( 'NONE',  ( 22.01249999999999574, -5.773502691896255534, -1.060575238724906372E-15 ) ) ;
#68737 = ORIENTED_EDGE ( 'NONE', *, *, #47742, .F. ) ;
#68738 = CARTESIAN_POINT ( 'NONE',  ( 26.47499999999999787, -4.330127018922194537, 2.499999999999995559 ) ) ;
#68739 = CARTESIAN_POINT ( 'NONE',  ( -3.999999999999999112, 12.34999999999999964, -30.00000000000000000 ) ) ;
#68740 = CARTESIAN_POINT ( 'NONE',  ( -7.967954043666661671E-16, 20.29062499938548214, 34.33755215474603517 ) ) ;
#68741 = CARTESIAN_POINT ( 'NONE',  ( 29.46562500061451573, -6.054752690667223547, -1.112240025338166033E-15 ) ) ;
#68742 = CARTESIAN_POINT ( 'NONE',  ( 10.75312500061451715, 4.541064518000418104, -2.621784821874998173 ) ) ;
#68743 = CARTESIAN_POINT ( 'NONE',  ( 21.97500000122903074, 2.886751345948126879, 4.999999999999999112 ) ) ;
#68744 = CARTESIAN_POINT ( 'NONE',  ( 26.84062500061451573, -3.027376345333610441, -5.243569643749999898 ) ) ;
#68745 = CARTESIAN_POINT ( 'NONE',  ( 27.11249999999999716, 2.886751345948129099, -4.999999999999998224 ) ) ;
#68746 = CARTESIAN_POINT ( 'NONE',  ( -3.999999999999999112, 15.61250000122903359, -30.00000000000000000 ) ) ;
#68747 = CARTESIAN_POINT ( 'NONE',  ( 29.65312500061451573, 4.541064518000418104, -2.621784821874998173 ) ) ;
#68748 = CARTESIAN_POINT ( 'NONE',  ( 11.57812500061451644, 6.421520780324663323E-16, -5.243569643749999010 ) ) ;
#68749 = ORIENTED_EDGE ( 'NONE', *, *, #30772, .F. ) ;
#68750 = CARTESIAN_POINT ( 'NONE',  ( 26.65312500061451573, 0.000000000000000000, 5.243569643749999010 ) ) ;
#68751 = CARTESIAN_POINT ( 'NONE',  ( 7.903125000614515727, -4.541064518000417216, -2.621784821875001281 ) ) ;
#68752 = CARTESIAN_POINT ( 'NONE',  ( 4.828125000614518214, 6.421520780324663323E-16, -5.243569643749999010 ) ) ;
#68753 = CARTESIAN_POINT ( 'NONE',  ( 16.35937500061451644, 0.000000000000000000, 4.756430356249998326 ) ) ;
#68754 = CARTESIAN_POINT ( 'NONE',  ( 13.04999999999999893, -4.330127018922190985, -2.500000000000001332 ) ) ;
#68755 = CARTESIAN_POINT ( 'NONE',  ( 16.53750000000000142, -2.886751345948129988, 4.999999999999997335 ) ) ;
#68756 = CARTESIAN_POINT ( 'NONE',  ( 15.04687500061451644, -3.027376345333614438, 5.243569643749998122 ) ) ;
#68757 = CARTESIAN_POINT ( 'NONE',  ( 10.76250000122903572, 0.000000000000000000, 4.999999999999998224 ) ) ;
#68758 = EDGE_CURVE ( 'NONE', #18233, #48333, #23561, .T. ) ;
#68759 = CARTESIAN_POINT ( 'NONE',  ( 17.52187500061451431, 3.027376345333613106, -5.243569643749998122 ) ) ;
#68760 = CARTESIAN_POINT ( 'NONE',  ( 17.36249999999999716, 2.886751345948126879, 4.999999999999999112 ) ) ;
#68761 = CARTESIAN_POINT ( 'NONE',  ( 21.98437500061451644, 6.421520780324663323E-16, -5.243569643749999010 ) ) ;
#68762 = CARTESIAN_POINT ( 'NONE',  ( -2.121784821874996840, 13.12812500061451715, -26.32496088578401583 ) ) ;
#68763 = LINE ( 'NONE', #1531, #56039 ) ;
#68764 = CARTESIAN_POINT ( 'NONE',  ( 23.55937500061451573, -5.492252693125287522, -1.008910452111647106E-15 ) ) ;
#68765 = CARTESIAN_POINT ( 'NONE',  ( -2.672702088255949472E-15, 13.45624999877096784, 26.00000000000000000 ) ) ;
#68766 = CARTESIAN_POINT ( 'NONE',  ( 24.59062500061451573, -3.027376345333610441, -5.243569643749999898 ) ) ;
#68767 = EDGE_CURVE ( 'NONE', #16738, #57497, #8890, .T. ) ;
#68768 = CARTESIAN_POINT ( 'NONE',  ( 29.29687500061451644, 6.054752690667223547, 3.707466751127219781E-16 ) ) ;
#68769 = CARTESIAN_POINT ( 'NONE',  ( 24.29999999999999716, -4.330127018922190985, -2.500000000000001332 ) ) ;
#68770 = ADVANCED_FACE ( 'NONE', ( #27184 ), #54212, .T. ) ;
#68771 = CARTESIAN_POINT ( 'NONE',  ( 5.803125000614517859, 4.541064518000418104, -2.621784821874998173 ) ) ;
#68772 = CARTESIAN_POINT ( 'NONE',  ( 25.35937500061451644, -5.492252693125287522, -1.008910452111647106E-15 ) ) ;
#68773 = CARTESIAN_POINT ( 'NONE',  ( 18.60937500061451644, 0.000000000000000000, 5.243569643749999010 ) ) ;
#68774 = CARTESIAN_POINT ( 'NONE',  ( 11.44687500061451679, -4.119189519843965641, -2.378215178125001383 ) ) ;
#68775 = CARTESIAN_POINT ( 'NONE',  ( 3.478125000614517237, 6.421520780324663323E-16, -5.243569643749999010 ) ) ;
#68776 = CARTESIAN_POINT ( 'NONE',  ( 7.771875000614516971, 3.027376345333611329, 5.243569643749999010 ) ) ;
#68777 = VERTEX_POINT ( 'NONE', #36814 ) ;
#68778 = CARTESIAN_POINT ( 'NONE',  ( 19.69687500061451857, -3.027376345333610441, -5.243569643749999898 ) ) ;
#68779 = DIRECTION ( 'NONE',  ( -1.000000000000000000, -0.000000000000000000, -0.000000000000000000 ) ) ;
#68780 = CARTESIAN_POINT ( 'NONE',  ( 25.57499999999999929, -4.330127018922194537, 2.499999999999995559 ) ) ;
#68781 = CARTESIAN_POINT ( 'NONE',  ( 28.99687500061451573, -3.027376345333614438, 5.243569643749998122 ) ) ;
#68782 = CARTESIAN_POINT ( 'NONE',  ( 3.999999999999999112, 10.32500000000000107, -30.00000000000000000 ) ) ;
#68783 = CARTESIAN_POINT ( 'NONE',  ( 12.43125000122903145, 4.330127018922191873, 2.499999999999999556 ) ) ;
#68784 = ORIENTED_EDGE ( 'NONE', *, *, #30682, .T. ) ;
#68785 = CARTESIAN_POINT ( 'NONE',  ( 11.40000000000000036, 4.330127018922192761, -2.499999999999997780 ) ) ;
#68786 = CARTESIAN_POINT ( 'NONE',  ( 11.44687500061451679, -4.119189519843965641, -2.378215178125001383 ) ) ;
#68787 = CARTESIAN_POINT ( 'NONE',  ( 24.77812500061451217, 4.541064518000418104, 2.621784821874999949 ) ) ;
#68788 = CARTESIAN_POINT ( 'NONE',  ( 13.31250000000000178, 2.886751345948126879, 4.999999999999999112 ) ) ;
#68789 = EDGE_CURVE ( 'NONE', #26491, #69693, #21184, .T. ) ;
#68790 = CARTESIAN_POINT ( 'NONE',  ( 9.900000001229033231, -2.886751345948129988, 4.999999999999997335 ) ) ;
#68791 = CARTESIAN_POINT ( 'NONE',  ( 9.965625000614517504, 3.027376345333611329, 5.243569643749999010 ) ) ;
#68792 = CARTESIAN_POINT ( 'NONE',  ( 22.42500000000000071, -4.330127018922194537, 2.499999999999995559 ) ) ;
#68793 = CARTESIAN_POINT ( 'NONE',  ( 21.59062500061451928, 6.054752690667223547, 3.707466751127219781E-16 ) ) ;
#68794 = CARTESIAN_POINT ( 'NONE',  ( 15.93750000122903110, 6.123233995736764310E-16, -4.999999999999998224 ) ) ;
#68795 = CARTESIAN_POINT ( 'NONE',  ( 26.28750000122903430, 6.123233995736764310E-16, -4.999999999999998224 ) ) ;
#68796 = CARTESIAN_POINT ( 'NONE',  ( 1.878215178124997609, 17.51562499938548356, 33.25316411605952993 ) ) ;
#68797 = CARTESIAN_POINT ( 'NONE',  ( 8.175000000000002487, 6.123233995736764310E-16, -4.999999999999998224 ) ) ;
#68798 = ORIENTED_EDGE ( 'NONE', *, *, #24642, .T. ) ;
#68799 = CARTESIAN_POINT ( 'NONE',  ( 22.56562500061451715, 3.027376345333611329, 5.243569643749999010 ) ) ;
#68800 = CARTESIAN_POINT ( 'NONE',  ( 29.65312500061451573, 4.541064518000418104, -2.621784821874998173 ) ) ;
#68801 = CARTESIAN_POINT ( 'NONE',  ( 27.60937500061451644, 0.000000000000000000, 5.243569643749999010 ) ) ;
#68802 = CARTESIAN_POINT ( 'NONE',  ( 19.58437500061451786, -4.541064518000419881, 2.621784821874995952 ) ) ;
#68803 = CARTESIAN_POINT ( 'NONE',  ( 13.22812500061451502, -4.541064518000419881, 2.621784821874995952 ) ) ;
#68804 = CARTESIAN_POINT ( 'NONE',  ( 2.121784821875001281, 10.05312500061459247, -26.32496088578401938 ) ) ;
#68805 = CARTESIAN_POINT ( 'NONE',  ( 26.62500000122903288, -5.773502691896255534, -1.060575238724906372E-15 ) ) ;
#68806 = CARTESIAN_POINT ( 'NONE',  ( 21.98437500061451644, 5.824947211148865298E-16, -4.756430356249998326 ) ) ;
#68807 = CARTESIAN_POINT ( 'NONE',  ( 15.59062500061451573, -3.027376345333610441, -5.243569643749999898 ) ) ;
#68808 = CARTESIAN_POINT ( 'NONE',  ( 13.42499999999999893, -4.330127018922194537, 2.499999999999995559 ) ) ;
#68809 = CARTESIAN_POINT ( 'NONE',  ( 2.700000001229035718, -2.886751345948129988, 4.999999999999997335 ) ) ;
#68810 = CARTESIAN_POINT ( 'NONE',  ( 11.70937500061451608, 4.541064518000418104, -2.621784821874998173 ) ) ;
#68811 = CARTESIAN_POINT ( 'NONE',  ( 11.63437500061451857, 6.421520780324663323E-16, -5.243569643749999010 ) ) ;
#68812 = CARTESIAN_POINT ( 'NONE',  ( 20.63437500061451857, 6.421520780324663323E-16, -5.243569643749999010 ) ) ;
#68813 = ORIENTED_EDGE ( 'NONE', *, *, #62426, .F. ) ;
#68814 = DIRECTION ( 'NONE',  ( -1.000000000000000000, -0.000000000000000000, -0.000000000000000000 ) ) ;
#68815 = CARTESIAN_POINT ( 'NONE',  ( 23.87812500061451715, 4.541064518000418104, 2.621784821874999949 ) ) ;
#68816 = CARTESIAN_POINT ( 'NONE',  ( 19.58437500061451786, -4.541064518000419881, 2.621784821874995952 ) ) ;
#68817 = CARTESIAN_POINT ( 'NONE',  ( 24.44062500061451715, -3.027376345333614438, 5.243569643749998122 ) ) ;
#68818 = CARTESIAN_POINT ( 'NONE',  ( 1.071796769724489895, 12.21740381056766900, -34.00000000000000000 ) ) ;
#68819 = CARTESIAN_POINT ( 'NONE',  ( -1.999999999999997113, 14.22500000000000142, 33.46410161513775705 ) ) ;
#68820 = CARTESIAN_POINT ( 'NONE',  ( 28.67812500061451431, 6.421520780324663323E-16, -5.243569643749999010 ) ) ;
#68821 = CARTESIAN_POINT ( 'NONE',  ( 9.300000001229035362, 5.773502691896255534, 3.535250795749688894E-16 ) ) ;
#68822 = CARTESIAN_POINT ( 'NONE',  ( 3.637500001229036162, -4.330127018922194537, 2.499999999999995559 ) ) ;
#68823 = CARTESIAN_POINT ( 'NONE',  ( 28.87500000122902932, -5.773502691896255534, -1.060575238724906372E-15 ) ) ;
#68824 = CARTESIAN_POINT ( 'NONE',  ( 26.21250000122903501, -4.330127018922190985, -2.500000000000001332 ) ) ;
#68825 = CARTESIAN_POINT ( 'NONE',  ( -1.878215178124999163, 12.90312499938548463, 26.74683588394047007 ) ) ;
#68826 = CARTESIAN_POINT ( 'NONE',  ( 16.40625000122903643, 4.330127018922192761, -2.499999999999997780 ) ) ;
#68827 = CARTESIAN_POINT ( 'NONE',  ( 8.409375000614518925, -4.541064518000417216, -2.621784821875001281 ) ) ;
#68828 = CARTESIAN_POINT ( 'NONE',  ( 9.299999999999998934, 0.000000000000000000, 4.999999999999998224 ) ) ;
#68829 = CARTESIAN_POINT ( 'NONE',  ( 17.27812500061451217, -4.541064518000419881, 2.621784821874995952 ) ) ;
#68830 = CARTESIAN_POINT ( 'NONE',  ( 11.78437500061451892, 4.541064518000418104, 2.621784821874999949 ) ) ;
#68831 = CARTESIAN_POINT ( 'NONE',  ( 3.478125000614517237, 6.421520780324663323E-16, -5.243569643749999010 ) ) ;
#68832 = CARTESIAN_POINT ( 'NONE',  ( 19.20937500061451786, -4.541064518000417216, -2.621784821875001281 ) ) ;
#68833 = CARTESIAN_POINT ( 'NONE',  ( 7.246875000614518392, 6.054752690667223547, 3.707466751127219781E-16 ) ) ;
#68834 = CARTESIAN_POINT ( 'NONE',  ( 3.628125000614518036, 4.541064518000418104, 2.621784821874999949 ) ) ;
#68835 = CARTESIAN_POINT ( 'NONE',  ( 8.765625000614518214, -6.054752690667223547, -1.112240025338166033E-15 ) ) ;
#68836 = CARTESIAN_POINT ( 'NONE',  ( 18.02812500061451573, 4.541064518000418104, 2.621784821874999949 ) ) ;
#68837 = ORIENTED_EDGE ( 'NONE', *, *, #39594, .F. ) ;
#68838 = CARTESIAN_POINT ( 'NONE',  ( 6.637500001229035718, 4.330127018922191873, 2.499999999999999556 ) ) ;
#68839 = CARTESIAN_POINT ( 'NONE',  ( 15.40312500061451573, 0.000000000000000000, 5.243569643749999010 ) ) ;
#68840 = CARTESIAN_POINT ( 'NONE',  ( 12.32812500061451821, -4.541064518000419881, 2.621784821874995952 ) ) ;
#68841 = CARTESIAN_POINT ( 'NONE',  ( 23.18437500061451573, -4.119189519843968306, 2.378215178124996054 ) ) ;
#68842 = CARTESIAN_POINT ( 'NONE',  ( 13.42499999999999893, -4.330127018922194537, 2.499999999999995559 ) ) ;
#68843 = CARTESIAN_POINT ( 'NONE',  ( 6.450000001229034829, -2.886751345948125991, -5.000000000000000000 ) ) ;
#68844 = CARTESIAN_POINT ( 'NONE',  ( 4.528125000614516615, 4.541064518000418104, 2.621784821874999949 ) ) ;
#68845 = CARTESIAN_POINT ( 'NONE',  ( 18.93750000122903288, -4.330127018922194537, 2.499999999999995559 ) ) ;
#68846 = CARTESIAN_POINT ( 'NONE',  ( 25.76249999999999929, 2.886751345948129099, -4.999999999999998224 ) ) ;
#68847 = CARTESIAN_POINT ( 'NONE',  ( -4.243569643749997233, 10.44687500061451857, -27.54997392385601174 ) ) ;
#68848 = CARTESIAN_POINT ( 'NONE',  ( 8.625000000000000000, 6.123233995736764310E-16, -4.999999999999998224 ) ) ;
#68849 = EDGE_CURVE ( 'NONE', #69178, #52021, #59806, .T. ) ;
#68850 = CARTESIAN_POINT ( 'NONE',  ( 12.95625000122903359, 0.000000000000000000, 4.999999999999998224 ) ) ;
#68851 = CARTESIAN_POINT ( 'NONE',  ( -3.137519842735245283E-14, 11.56250000000000178, -26.00000000000000711 ) ) ;
#68852 = CARTESIAN_POINT ( 'NONE',  ( 30.00000000000000000, 0.000000000000000000, 4.999999999999998224 ) ) ;
#68853 = CARTESIAN_POINT ( 'NONE',  ( 17.63437500061451502, 4.541064518000418104, 2.621784821874999949 ) ) ;
#68854 = CARTESIAN_POINT ( 'NONE',  ( 15.37500000000000000, 6.123233995736764310E-16, -4.999999999999998224 ) ) ;
#68855 = CARTESIAN_POINT ( 'NONE',  ( 14.50312500061451537, 0.000000000000000000, 5.243569643749999010 ) ) ;
#68856 = CARTESIAN_POINT ( 'NONE',  ( 8.681250001229031454, 6.123233995736764310E-16, -4.999999999999998224 ) ) ;
#68857 = CARTESIAN_POINT ( 'NONE',  ( 2.000000000000000444, 16.62500000000000000, 26.53589838486224650 ) ) ;
#68858 = CARTESIAN_POINT ( 'NONE',  ( 26.48437500061451644, 6.421520780324663323E-16, -5.243569643749999010 ) ) ;
#68859 = CARTESIAN_POINT ( 'NONE',  ( 19.09687500061451360, -4.119189519843965641, -2.378215178125001383 ) ) ;
#68860 = CARTESIAN_POINT ( 'NONE',  ( 11.84062500061451750, -3.027376345333614438, 5.243569643749998122 ) ) ;
#68861 = CARTESIAN_POINT ( 'NONE',  ( 16.43437500061451573, -4.541064518000419881, 2.621784821874995952 ) ) ;
#68862 = VERTEX_POINT ( 'NONE', #25507 ) ;
#68863 = CARTESIAN_POINT ( 'NONE',  ( 27.06562500061451004, 3.027376345333611329, 5.243569643749999010 ) ) ;
#68864 = CARTESIAN_POINT ( 'NONE',  ( 20.24062500061451431, 6.054752690667223547, 3.707466751127219781E-16 ) ) ;
#68865 = CARTESIAN_POINT ( 'NONE',  ( 3.089506346739232967, 3.931278485869285522, -3.469880700456108968 ) ) ;
#68866 = DIRECTION ( 'NONE',  ( -1.000000000000000000, -0.000000000000000000, -0.000000000000000000 ) ) ;
#68867 = CARTESIAN_POINT ( 'NONE',  ( 9.487500000000000711, -2.886751345948125991, -5.000000000000000000 ) ) ;
#68868 = CARTESIAN_POINT ( 'NONE',  ( 19.98750000122903359, 6.123233995736764310E-16, -4.999999999999998224 ) ) ;
#68869 = LINE ( 'NONE', #47418, #71432 ) ;
#68870 = CARTESIAN_POINT ( 'NONE',  ( 11.07187500061451679, 5.824947211148865298E-16, -4.756430356249998326 ) ) ;
#68871 = ORIENTED_EDGE ( 'NONE', *, *, #68849, .F. ) ;
#68872 = CARTESIAN_POINT ( 'NONE',  ( 17.13749999999999929, -2.886751345948125991, -5.000000000000000000 ) ) ;
#68873 = CARTESIAN_POINT ( 'NONE',  ( 20.96250000000000213, 2.886751345948126879, 4.999999999999999112 ) ) ;
#68874 = CARTESIAN_POINT ( 'NONE',  ( 19.73437500061451644, 6.421520780324663323E-16, -5.243569643749999010 ) ) ;
#68875 = CARTESIAN_POINT ( 'NONE',  ( 24.44062500061451715, -3.027376345333614438, 5.243569643749998122 ) ) ;
#68876 = EDGE_LOOP ( 'NONE', ( #18921, #61882, #18868, #66690 ) ) ;
#68877 = CARTESIAN_POINT ( 'NONE',  ( 27.86250000122903359, 0.000000000000000000, 4.999999999999998224 ) ) ;
#68878 = CARTESIAN_POINT ( 'NONE',  ( 8.128125000614515372, 4.541064518000418104, 2.621784821874999949 ) ) ;
#68879 = CARTESIAN_POINT ( 'NONE',  ( -4.000000000000000888, 19.00624999877096499, 32.30940107675850470 ) ) ;
#68880 = CARTESIAN_POINT ( 'NONE',  ( 15.03749999999999964, 5.773502691896255534, 3.535250795749688894E-16 ) ) ;
#68881 = CARTESIAN_POINT ( 'NONE',  ( 2.121784821874999061, 18.30312500061451431, 26.32496088578401583 ) ) ;
#68882 = CARTESIAN_POINT ( 'NONE',  ( 29.76562500061451644, 3.027376345333611329, 5.243569643749999010 ) ) ;
#68883 = CARTESIAN_POINT ( 'NONE',  ( 9.525000000000002132, 6.123233995736764310E-16, -4.999999999999998224 ) ) ;
#68884 = CARTESIAN_POINT ( 'NONE',  ( -3.756430356249999214, 17.77812499938548285, 27.83122392262697531 ) ) ;
#68885 = CARTESIAN_POINT ( 'NONE',  ( 27.00937500061451857, 4.541064518000418104, -2.621784821874998173 ) ) ;
#68886 = ORIENTED_EDGE ( 'NONE', *, *, #8189, .F. ) ;
#68887 = CARTESIAN_POINT ( 'NONE',  ( 21.89062500061451289, -3.027376345333610441, -5.243569643749999898 ) ) ;
#68888 = CARTESIAN_POINT ( 'NONE',  ( 23.78437500061451360, 6.421520780324663323E-16, -5.243569643749999010 ) ) ;
#68889 = CARTESIAN_POINT ( 'NONE',  ( -4.243569643749999898, 16.16562500061459673, -32.45002607614398471 ) ) ;
#68890 = CARTESIAN_POINT ( 'NONE',  ( 10.35000000000000142, -4.330127018922190985, -2.500000000000001332 ) ) ;
#68891 = CARTESIAN_POINT ( 'NONE',  ( 5.315625000614516260, 3.027376345333613106, -5.243569643749998122 ) ) ;
#68892 = CARTESIAN_POINT ( 'NONE',  ( 29.33437500061451431, 4.119189519843966529, 2.378215178124999607 ) ) ;
#68893 = CARTESIAN_POINT ( 'NONE',  ( 23.05312500061451431, 0.000000000000000000, 5.243569643749999010 ) ) ;
#68894 = CARTESIAN_POINT ( 'NONE',  ( 28.69687500061451502, 4.119189519843966529, -2.378215178124998275 ) ) ;
#68895 = CARTESIAN_POINT ( 'NONE',  ( 13.17187500061451999, 2.746126346562643317, 4.756430356249998326 ) ) ;
#68896 = CARTESIAN_POINT ( 'NONE',  ( 17.97187500061451715, 3.027376345333613106, -5.243569643749998122 ) ) ;
#68897 = CARTESIAN_POINT ( 'NONE',  ( 9.001249775931846008E-16, 13.22187500061451715, 34.90005215228797653 ) ) ;
#68898 = CARTESIAN_POINT ( 'NONE',  ( 18.12187500061451573, 3.027376345333611329, 5.243569643749999010 ) ) ;
#68899 = CARTESIAN_POINT ( 'NONE',  ( 26.33437500061451431, -4.541064518000419881, 2.621784821874995952 ) ) ;
#68900 = CARTESIAN_POINT ( 'NONE',  ( -4.243569643749999898, 15.80937500061451573, 30.00000000000000000 ) ) ;
#68901 = CARTESIAN_POINT ( 'NONE',  ( 7.528125000614515727, 6.421520780324663323E-16, -5.243569643749999010 ) ) ;
#68902 = DIRECTION ( 'NONE',  ( -1.000000000000000000, -0.000000000000000000, -0.000000000000000000 ) ) ;
#68903 = CARTESIAN_POINT ( 'NONE',  ( 3.796875000614517326, -3.027376345333614438, 5.243569643749998122 ) ) ;
#68904 = DIRECTION ( 'NONE',  ( -1.000000000000000000, -0.000000000000000000, -0.000000000000000000 ) ) ;
#68905 = CARTESIAN_POINT ( 'NONE',  ( 4.528125000614516615, 4.541064518000418104, 2.621784821874999949 ) ) ;
#68906 = CARTESIAN_POINT ( 'NONE',  ( 9.271875000614516082, -6.054752690667223547, -1.112240025338166033E-15 ) ) ;
#68907 = CARTESIAN_POINT ( 'NONE',  ( 17.21250000122903145, -4.330127018922190985, -2.500000000000001332 ) ) ;
#68908 = CARTESIAN_POINT ( 'NONE',  ( 5.146875000614517859, -3.027376345333614438, 5.243569643749998122 ) ) ;
#68909 = CARTESIAN_POINT ( 'NONE',  ( 6.403125000614517504, 0.000000000000000000, 5.243569643749999010 ) ) ;
#68910 = CARTESIAN_POINT ( 'NONE',  ( -3.999999999999999556, 13.53124999877096535, 27.69059892324149175 ) ) ;
#68911 = CARTESIAN_POINT ( 'NONE',  ( 22.89375000122903359, -2.886751345948129988, 4.999999999999997335 ) ) ;
#68912 = CARTESIAN_POINT ( 'NONE',  ( 17.29687500061451999, -3.027376345333614438, 5.243569643749998122 ) ) ;
#68913 = FACE_OUTER_BOUND ( 'NONE', #29084, .T. ) ;
#68914 = ORIENTED_EDGE ( 'NONE', *, *, #42571, .F. ) ;
#68915 = CARTESIAN_POINT ( 'NONE',  ( 25.34062500061451217, -3.027376345333614438, 5.243569643749998122 ) ) ;
#68916 = CARTESIAN_POINT ( 'NONE',  ( 8.878125000614515372, 6.421520780324663323E-16, -5.243569643749999010 ) ) ;
#68917 = CARTESIAN_POINT ( 'NONE',  ( 27.38437500061451857, 6.421520780324663323E-16, -5.243569643749999010 ) ) ;
#68918 = CARTESIAN_POINT ( 'NONE',  ( 10.26562500061451644, 3.027376345333613106, -5.243569643749998122 ) ) ;
#68919 = CARTESIAN_POINT ( 'NONE',  ( 4.413397852867026572, -2.350023558854721362, -4.663726614112597701 ) ) ;
#68920 = CARTESIAN_POINT ( 'NONE',  ( 9.450000001229033941, -2.886751345948129988, 4.999999999999997335 ) ) ;
#68921 = EDGE_CURVE ( 'NONE', #33991, #48298, #59475, .T. ) ;
#68922 = CARTESIAN_POINT ( 'NONE',  ( 25.00312500061451715, -4.541064518000417216, -2.621784821875001281 ) ) ;
#68923 = CARTESIAN_POINT ( 'NONE',  ( -3.000416591977282496E-16, 13.84062500061451928, -34.90005215228797653 ) ) ;
#68924 = CARTESIAN_POINT ( 'NONE',  ( 12.26250000122903394, -4.330127018922190985, -2.500000000000001332 ) ) ;
#68925 = CARTESIAN_POINT ( 'NONE',  ( 23.24062500061451786, -3.027376345333610441, -5.243569643749999898 ) ) ;
#68926 = CARTESIAN_POINT ( 'NONE',  ( 11.43750000000000000, 5.773502691896255534, 3.535250795749688894E-16 ) ) ;
#68927 = CARTESIAN_POINT ( 'NONE',  ( 19.49062500061451431, -3.027376345333614438, 5.243569643749998122 ) ) ;
#68928 = CARTESIAN_POINT ( 'NONE',  ( 5.446875000614519458, 6.054752690667223547, 3.707466751127219781E-16 ) ) ;
#68929 = CARTESIAN_POINT ( 'NONE',  ( 19.42499999999999716, 6.123233995736764310E-16, -4.999999999999998224 ) ) ;
#68930 = CARTESIAN_POINT ( 'NONE',  ( 6.637500001229035718, 4.330127018922191873, 2.499999999999999556 ) ) ;
#68931 = CARTESIAN_POINT ( 'NONE',  ( 17.02500000122903145, 2.886751345948126879, 4.999999999999999112 ) ) ;
#68932 =( BOUNDED_CURVE ( )  B_SPLINE_CURVE ( 2, ( #67344, #38529, #44811, #16705, #11178, #33702, #44076 ),
 .UNSPECIFIED., .F., .F. ) 
 B_SPLINE_CURVE_WITH_KNOTS ( ( 3, 2, 2, 3 ),
 ( 0.3900000000000000133, 0.3933333333333333126, 0.3966666666666667229, 0.4000000000000000777 ),
 .UNSPECIFIED. ) 
 CURVE ( )  GEOMETRIC_REPRESENTATION_ITEM ( )  RATIONAL_B_SPLINE_CURVE ( ( 1.000000000000000000, 0.8660254037844387076, 1.000000000000000000, 0.8660254037844387076, 1.000000000000000000, 0.8660254037844364872, 1.000000000000002220 ) ) 
 REPRESENTATION_ITEM ( '' )  );
#68933 = CARTESIAN_POINT ( 'NONE',  ( 11.76562500061451644, 3.027376345333611329, 5.243569643749999010 ) ) ;
#68934 = CARTESIAN_POINT ( 'NONE',  ( 14.76562500061451821, 3.027376345333613106, -5.243569643749998122 ) ) ;
#68935 = CARTESIAN_POINT ( 'NONE',  ( 26.70000000122903572, -2.886751345948125991, -5.000000000000000000 ) ) ;
#68936 = CARTESIAN_POINT ( 'NONE',  ( 21.52499999999999858, -4.330127018922194537, 2.499999999999995559 ) ) ;
#68937 = CARTESIAN_POINT ( 'NONE',  ( 22.77187500061451786, -6.054752690667223547, -1.112240025338166033E-15 ) ) ;
#68938 = CYLINDRICAL_SURFACE ( 'NONE', #25304, 4.999999999999998224 ) ;
#68939 = EDGE_CURVE ( 'NONE', #17423, #51420, #36589, .T. ) ;
#68940 = CARTESIAN_POINT ( 'NONE',  ( 11.21250000122903501, 0.000000000000000000, 4.999999999999998224 ) ) ;
#68941 = CARTESIAN_POINT ( 'NONE',  ( 9.871875000614517504, 3.027376345333613106, -5.243569643749998122 ) ) ;
#68942 = CARTESIAN_POINT ( 'NONE',  ( 24.64687500061451431, -3.027376345333610441, -5.243569643749999898 ) ) ;
#68943 =( BOUNDED_CURVE ( )  B_SPLINE_CURVE ( 2, ( #20563, #43121, #65645, #15394, #22038, #67487, #33479 ),
 .UNSPECIFIED., .F., .F. ) 
 B_SPLINE_CURVE_WITH_KNOTS ( ( 3, 2, 2, 3 ),
 ( 0.7083333333333334814, 0.7111111111111112493, 0.7138888888888890172, 0.7166666666666667851 ),
 .UNSPECIFIED. ) 
 CURVE ( )  GEOMETRIC_REPRESENTATION_ITEM ( )  RATIONAL_B_SPLINE_CURVE ( ( 0.9999999999999946709, 0.8660254037844440367, 1.000000000000000000, 0.8660254037844387076, 1.000000000000000000, 0.8660254037844333785, 1.000000000000005329 ) ) 
 REPRESENTATION_ITEM ( '' )  );
#68944 = CARTESIAN_POINT ( 'NONE',  ( 21.17812500061451431, 4.541064518000418104, 2.621784821874999949 ) ) ;
#68945 = CARTESIAN_POINT ( 'NONE',  ( 27.45937500061451786, 4.541064518000418104, -2.621784821874998173 ) ) ;
#68946 = CARTESIAN_POINT ( 'NONE',  ( -3.756430356249999214, 18.34062499938548640, 27.83122392262697176 ) ) ;
#68947 = CARTESIAN_POINT ( 'NONE',  ( 7.800000000000001599, 4.330127018922192761, -2.499999999999997780 ) ) ;
#68948 = CARTESIAN_POINT ( 'NONE',  ( 8.784375000614518925, -4.541064518000419881, 2.621784821874995952 ) ) ;
#68949 = CARTESIAN_POINT ( 'NONE',  ( 20.01562500061451644, -6.054752690667223547, -1.112240025338166033E-15 ) ) ;
#68950 = ORIENTED_EDGE ( 'NONE', *, *, #22648, .F. ) ;
#68951 = CARTESIAN_POINT ( 'NONE',  ( 30.00000000000000000, 0.000000000000000000, 4.999999999999998224 ) ) ;
#68952 = CARTESIAN_POINT ( 'NONE',  ( 27.70312500061451289, -4.541064518000417216, -2.621784821875001281 ) ) ;
#68953 = CARTESIAN_POINT ( 'NONE',  ( 3.834375000614519635, -4.541064518000419881, 2.621784821874995952 ) ) ;
#68954 = CARTESIAN_POINT ( 'NONE',  ( 22.76250000122903216, 4.330127018922192761, -2.499999999999997780 ) ) ;
#68955 = EDGE_CURVE ( 'NONE', #5357, #69237, #28745, .T. ) ;
#68956 = CARTESIAN_POINT ( 'NONE',  ( 3.586992791275801729, 3.483314903268937446, -3.919380039434936513 ) ) ;
#68957 = CARTESIAN_POINT ( 'NONE',  ( 17.32499999999999929, 4.330127018922191873, 2.499999999999999556 ) ) ;
#68958 = CARTESIAN_POINT ( 'NONE',  ( 20.42812500061451431, -4.541064518000419881, 2.621784821874995952 ) ) ;
#68959 = VERTEX_POINT ( 'NONE', #9253 ) ;
#68960 = CARTESIAN_POINT ( 'NONE',  ( 24.26249999999999929, -5.773502691896255534, -1.060575238724906372E-15 ) ) ;
#68961 = CARTESIAN_POINT ( 'NONE',  ( 26.14687500061451431, 6.054752690667223547, 3.707466751127219781E-16 ) ) ;
#68962 = ORIENTED_EDGE ( 'NONE', *, *, #21957, .T. ) ;
#68963 = CARTESIAN_POINT ( 'NONE',  ( 15.74062500061451608, 6.054752690667223547, 3.707466751127219781E-16 ) ) ;
#68964 = CARTESIAN_POINT ( 'NONE',  ( 5.428125000614517859, 4.541064518000418104, 2.621784821874999949 ) ) ;
#68965 = CARTESIAN_POINT ( 'NONE',  ( 19.69687500061451502, 4.119189519843966529, -2.378215178124998275 ) ) ;
#68966 = CARTESIAN_POINT ( 'NONE',  ( 2.859375000614519546, 0.000000000000000000, 5.243569643749999010 ) ) ;
#68967 =( BOUNDED_CURVE ( )  B_SPLINE_CURVE ( 2, ( #4960, #56295, #50394, #22659, #55206, #62548, #72191 ),
 .UNSPECIFIED., .F., .F. ) 
 B_SPLINE_CURVE_WITH_KNOTS ( ( 3, 2, 2, 3 ),
 ( 0.000000000000000000, 0.003333333333333326608, 0.006666666666666653217, 0.009999999999999979391 ),
 .UNSPECIFIED. ) 
 CURVE ( )  GEOMETRIC_REPRESENTATION_ITEM ( )  RATIONAL_B_SPLINE_CURVE ( ( 1.000000000000000000, 0.8660254037844387076, 1.000000000000000000, 0.8660254037844387076, 1.000000000000000000, 0.8660254037844395958, 0.9999999999999991118 ) ) 
 REPRESENTATION_ITEM ( '' )  );
#68968 = CARTESIAN_POINT ( 'NONE',  ( 15.67500000122903181, 2.886751345948126879, 4.999999999999999112 ) ) ;
#68969 = CARTESIAN_POINT ( 'NONE',  ( 23.02499999999999858, 6.123233995736764310E-16, -4.999999999999998224 ) ) ;
#68970 = CARTESIAN_POINT ( 'NONE',  ( 29.25000000000000000, -4.330127018922190985, -2.500000000000001332 ) ) ;
#68971 = CARTESIAN_POINT ( 'NONE',  ( 5.784375000614517148, 6.421520780324663323E-16, -5.243569643749999010 ) ) ;
#68972 = CARTESIAN_POINT ( 'NONE',  ( 9.384375000614518569, 6.421520780324663323E-16, -5.243569643749999010 ) ) ;
#68973 = CARTESIAN_POINT ( 'NONE',  ( 19.28437500061451360, 6.421520780324663323E-16, -5.243569643749999010 ) ) ;
#68974 = CARTESIAN_POINT ( 'NONE',  ( 9.975000001229034297, -5.773502691896255534, -1.060575238724906372E-15 ) ) ;
#68975 = ORIENTED_EDGE ( 'NONE', *, *, #19271, .F. ) ;
#68976 = CARTESIAN_POINT ( 'NONE',  ( 28.75312500061451715, 4.541064518000418104, -2.621784821874998173 ) ) ;
#68977 = CARTESIAN_POINT ( 'NONE',  ( 4.050000000000001599, -4.330127018922190985, -2.500000000000001332 ) ) ;
#68978 = CARTESIAN_POINT ( 'NONE',  ( 4.171875000614517326, 3.027376345333611329, 5.243569643749999010 ) ) ;
#68979 = CARTESIAN_POINT ( 'NONE',  ( 19.20000000000000284, 0.000000000000000000, 4.999999999999998224 ) ) ;
#68980 = CARTESIAN_POINT ( 'NONE',  ( 16.15312500061451573, 4.541064518000418104, -2.621784821874998173 ) ) ;
#68981 = CARTESIAN_POINT ( 'NONE',  ( -0.7391741542267653564, 20.47364048460824648, 34.19203975659616646 ) ) ;
#68982 = CARTESIAN_POINT ( 'NONE',  ( 45.00000000000000000, -5.218601775200048642, 7.332543590861146932 ) ) ;
#68983 = CARTESIAN_POINT ( 'NONE',  ( 20.74687500061451573, 5.492252693125287522, 3.363034840372157021E-16 ) ) ;
#68984 = CARTESIAN_POINT ( 'NONE',  ( 7.415625000614516793, -6.054752690667223547, -1.112240025338166033E-15 ) ) ;
#68985 = CARTESIAN_POINT ( 'NONE',  ( 26.40937500061451715, -4.541064518000417216, -2.621784821875001281 ) ) ;
#68986 = CARTESIAN_POINT ( 'NONE',  ( 2.121784821874999061, 19.25937500061451857, 26.32496088578401583 ) ) ;
#68987 = CARTESIAN_POINT ( 'NONE',  ( 26.40937500061451715, -4.541064518000417216, -2.621784821875001281 ) ) ;
#68988 = CARTESIAN_POINT ( 'NONE',  ( 7.724999999999999645, 6.123233995736764310E-16, -4.999999999999998224 ) ) ;
#68989 = CARTESIAN_POINT ( 'NONE',  ( 3.999999999999999112, 13.13750000122903394, 30.00000000000000000 ) ) ;
#68990 = CARTESIAN_POINT ( 'NONE',  ( 14.50312500061451537, 0.000000000000000000, 5.243569643749999010 ) ) ;
#68991 = CARTESIAN_POINT ( 'NONE',  ( 6.862500001229034474, -4.330127018922190985, -2.500000000000001332 ) ) ;
#68992 = CARTESIAN_POINT ( 'NONE',  ( 17.93437500061451928, 6.421520780324663323E-16, -5.243569643749999010 ) ) ;
#68993 = CARTESIAN_POINT ( 'NONE',  ( 12.27187500061451786, 3.027376345333611329, 5.243569643749999010 ) ) ;
#68994 = CARTESIAN_POINT ( 'NONE',  ( -3.861264241427935673, 3.177798304702605492, -31.07837686909879693 ) ) ;
#68995 = ORIENTED_EDGE ( 'NONE', *, *, #68656, .F. ) ;
#68996 = CARTESIAN_POINT ( 'NONE',  ( 12.66562500061451502, 3.027376345333611329, 5.243569643749999010 ) ) ;
#68997 = CARTESIAN_POINT ( 'NONE',  ( 23.77500000122903145, 2.886751345948126879, 4.999999999999999112 ) ) ;
#68998 = CARTESIAN_POINT ( 'NONE',  ( 13.99687500061451928, 6.054752690667223547, 3.707466751127219781E-16 ) ) ;
#68999 = CARTESIAN_POINT ( 'NONE',  ( 1.071796769724476572, 12.59509619066136921, 34.00000000000000000 ) ) ;
#69000 = CARTESIAN_POINT ( 'NONE',  ( 15.51562500061451644, -6.054752690667223547, -1.112240025338166033E-15 ) ) ;
#69001 = DIRECTION ( 'NONE',  ( 1.000000000000000000, 0.000000000000000000, 0.000000000000000000 ) ) ;
#69002 = CARTESIAN_POINT ( 'NONE',  ( 24.53437500061451715, -4.541064518000419881, 2.621784821874995952 ) ) ;
#69003 = DIRECTION ( 'NONE',  ( -1.000000000000000000, -0.000000000000000000, -0.000000000000000000 ) ) ;
#69004 = CARTESIAN_POINT ( 'NONE',  ( 11.13750000122903216, 4.330127018922191873, 2.499999999999999556 ) ) ;
#69005 = CARTESIAN_POINT ( 'NONE',  ( 30.00000000000000000, 0.000000000000000000, 0.000000000000000000 ) ) ;
#69006 = CARTESIAN_POINT ( 'NONE',  ( 8.849999999999999645, 0.000000000000000000, 4.999999999999998224 ) ) ;
#69007 = CARTESIAN_POINT ( 'NONE',  ( 9.001249775931846008E-16, 17.27187500061451786, -25.09994784771203058 ) ) ;
#69008 = CARTESIAN_POINT ( 'NONE',  ( 17.10937500061451999, 4.541064518000418104, -2.621784821874998173 ) ) ;
#69009 = CARTESIAN_POINT ( 'NONE',  ( 18.22500000122903430, 2.886751345948129099, -4.999999999999998224 ) ) ;
#69010 = AXIS2_PLACEMENT_3D ( 'NONE', #53428, #37160, #48621 ) ;
#69011 = CARTESIAN_POINT ( 'NONE',  ( 15.64687500061451608, -3.027376345333610441, -5.243569643749999898 ) ) ;
#69012 = FACE_OUTER_BOUND ( 'NONE', #42711, .T. ) ;
#69013 = CARTESIAN_POINT ( 'NONE',  ( 19.20000000122903572, 5.773502691896255534, 3.535250795749688894E-16 ) ) ;
#69014 = CARTESIAN_POINT ( 'NONE',  ( 14.05312500061451431, 0.000000000000000000, 5.243569643749999010 ) ) ;
#69015 = VERTEX_POINT ( 'NONE', #58743 ) ;
#69016 = ORIENTED_EDGE ( 'NONE', *, *, #11404, .F. ) ;
#69017 = CARTESIAN_POINT ( 'NONE',  ( 18.93750000000000000, -2.886751345948125991, -5.000000000000000000 ) ) ;
#69018 = CARTESIAN_POINT ( 'NONE',  ( 1.999999999999997335, 15.51874999877096784, 33.46410161513775705 ) ) ;
#69019 = CARTESIAN_POINT ( 'NONE',  ( 1.841668243974589059, 4.655663185590169562, 26.43913409586652818 ) ) ;
#69020 = CARTESIAN_POINT ( 'NONE',  ( 14.02500000122903323, -5.773502691896255534, -1.060575238724906372E-15 ) ) ;
#69021 = CARTESIAN_POINT ( 'NONE',  ( 27.79687500061451999, -3.027376345333610441, -5.243569643749999898 ) ) ;
#69022 = CARTESIAN_POINT ( 'NONE',  ( 20.54062500061451502, -3.027376345333610441, -5.243569643749999898 ) ) ;
#69023 = ADVANCED_FACE ( 'NONE', ( #8154 ), #19952, .T. ) ;
#69024 = CARTESIAN_POINT ( 'NONE',  ( 23.35312500061451857, 4.541064518000418104, -2.621784821874998173 ) ) ;
#69025 = CARTESIAN_POINT ( 'NONE',  ( 4.228125000614517681, -4.541064518000419881, 2.621784821874995952 ) ) ;
#69026 = CARTESIAN_POINT ( 'NONE',  ( 26.66250000000000142, 2.886751345948129099, -4.999999999999998224 ) ) ;
#69027 = CARTESIAN_POINT ( 'NONE',  ( 4.687500000000000000, 5.773502691896255534, 3.535250795749688401E-16 ) ) ;
#69028 = CARTESIAN_POINT ( 'NONE',  ( 8.071875000614518569, 2.746126346562645981, -4.756430356249997438 ) ) ;
#69029 = CARTESIAN_POINT ( 'NONE',  ( 6.262500001229034829, 0.000000000000000000, 4.999999999999998224 ) ) ;
#69030 = CARTESIAN_POINT ( 'NONE',  ( -3.999999999999997335, 9.800000001229033586, -27.69059892324149175 ) ) ;
#69031 = CARTESIAN_POINT ( 'NONE',  ( -2.121784821874999949, 17.08437500061451786, -33.67503911421598417 ) ) ;
#69032 = CARTESIAN_POINT ( 'NONE',  ( 6.262500001229034829, 0.000000000000000000, 4.999999999999998224 ) ) ;
#69033 = CARTESIAN_POINT ( 'NONE',  ( 6.750000000000002665, -4.330127018922190985, -2.500000000000001332 ) ) ;
#69034 = CARTESIAN_POINT ( 'NONE',  ( 4.762500001229033941, 4.330127018922192761, -2.499999999999997780 ) ) ;
#69035 = CARTESIAN_POINT ( 'NONE',  ( 10.99687500061451750, -3.027376345333614438, 5.243569643749998122 ) ) ;
#69036 = CARTESIAN_POINT ( 'NONE',  ( 28.26562500061451289, 3.027376345333613106, -5.243569643749998122 ) ) ;
#69037 = CARTESIAN_POINT ( 'NONE',  ( 45.00000000000000000, 0.000000000000000000, 0.000000000000000000 ) ) ;
#69038 = CARTESIAN_POINT ( 'NONE',  ( 5.587500001229033231, 6.123233995736764310E-16, -4.999999999999998224 ) ) ;
#69039 = CARTESIAN_POINT ( 'NONE',  ( 2.000000000000001332, 19.36250000122903359, 33.46410161513774995 ) ) ;
#69040 = CARTESIAN_POINT ( 'NONE',  ( 7.846875000614518036, -3.027376345333614438, 5.243569643749998122 ) ) ;
#69041 = CARTESIAN_POINT ( 'NONE',  ( 10.17187500061451999, -6.054752690667223547, -1.112240025338166033E-15 ) ) ;
#69042 = CARTESIAN_POINT ( 'NONE',  ( 5.662500000000000533, 2.886751345948126879, 4.999999999999999112 ) ) ;
#69043 = CARTESIAN_POINT ( 'NONE',  ( -4.243569643749998122, 14.89062500061459637, 32.45002607614398471 ) ) ;
#69044 = CARTESIAN_POINT ( 'NONE',  ( 1.071796769724491893, 17.88259618943233065, 33.99999999999999289 ) ) ;
#69045 = CARTESIAN_POINT ( 'NONE',  ( 6.825000000000001066, 6.123233995736764310E-16, -4.999999999999998224 ) ) ;
#69046 = CARTESIAN_POINT ( 'NONE',  ( 27.45000000122903572, -2.886751345948129988, 4.999999999999997335 ) ) ;
#69047 = VECTOR ( 'NONE', #50872, 1000.000000000000000 ) ;
#69048 = CARTESIAN_POINT ( 'NONE',  ( 16.54687500061451644, 4.119189519843966529, -2.378215178124998275 ) ) ;
#69049 = CARTESIAN_POINT ( 'NONE',  ( 23.20312500061451644, -4.541064518000417216, -2.621784821875001281 ) ) ;
#69050 = CARTESIAN_POINT ( 'NONE',  ( 14.20312500061451644, -4.541064518000417216, -2.621784821875001281 ) ) ;
#69051 = CARTESIAN_POINT ( 'NONE',  ( 26.07187500061451146, 4.119189519843966529, 2.378215178124999607 ) ) ;
#69052 = CARTESIAN_POINT ( 'NONE',  ( 10.24687500061451750, -3.027376345333610441, -5.243569643749999898 ) ) ;
#69053 = CARTESIAN_POINT ( 'NONE',  ( 29.13749999999999929, -2.886751345948129988, 4.999999999999997335 ) ) ;
#69054 = CARTESIAN_POINT ( 'NONE',  ( 23.36250000122903359, 0.000000000000000000, 4.999999999999998224 ) ) ;
#69055 = CARTESIAN_POINT ( 'NONE',  ( 11.32500000122903216, -5.773502691896255534, -1.060575238724906372E-15 ) ) ;
#69056 = VECTOR ( 'NONE', #8335, 1000.000000000000000 ) ;
#69057 = CARTESIAN_POINT ( 'NONE',  ( 12.94687500061451857, -3.027376345333610441, -5.243569643749999898 ) ) ;
#69058 = CARTESIAN_POINT ( 'NONE',  ( 25.80937500061451928, 0.000000000000000000, 5.243569643749999010 ) ) ;
#69059 = CARTESIAN_POINT ( 'NONE',  ( 3.946875000614517681, -3.027376345333610441, -5.243569643749999898 ) ) ;
#69060 = EDGE_CURVE ( 'NONE', #66931, #40447, #72269, .T. ) ;
#69061 = CARTESIAN_POINT ( 'NONE',  ( 1.999999999999998668, 13.66250000122903607, -33.46410161513775705 ) ) ;
#69062 = CARTESIAN_POINT ( 'NONE',  ( 22.43437500061451573, 6.421520780324663323E-16, -5.243569643749999010 ) ) ;
#69063 = CARTESIAN_POINT ( 'NONE',  ( 12.38437500061451857, -4.541064518000419881, 2.621784821874995952 ) ) ;
#69064 = EDGE_CURVE ( 'NONE', #23337, #16088, #36297, .T. ) ;
#69065 = CARTESIAN_POINT ( 'NONE',  ( 3.756430356250000546, 19.09062499938548640, 27.83122392262697886 ) ) ;
#69066 = CARTESIAN_POINT ( 'NONE',  ( 25.53750000000000142, -2.886751345948129988, 4.999999999999997335 ) ) ;
#69067 = CARTESIAN_POINT ( 'NONE',  ( -4.000000000000000888, 13.21250000000000036, 32.30940107675850470 ) ) ;
#69068 = CARTESIAN_POINT ( 'NONE',  ( -2.121784821874999949, 14.38437500061451679, -33.67503911421598417 ) ) ;
#69069 = CARTESIAN_POINT ( 'NONE',  ( 26.85937500061451644, -4.119189519843965641, -2.378215178125001383 ) ) ;
#69070 = CARTESIAN_POINT ( 'NONE',  ( 17.27812500061451217, -4.541064518000419881, 2.621784821874995952 ) ) ;
#69071 = CARTESIAN_POINT ( 'NONE',  ( 6.524999999999999467, 4.330127018922191873, 2.499999999999999556 ) ) ;
#69072 = DIRECTION ( 'NONE',  ( -0.000000000000000000, -1.000000000000000000, -0.000000000000000000 ) ) ;
#69073 = CARTESIAN_POINT ( 'NONE',  ( 15.15000000000000036, 0.000000000000000000, 4.999999999999998224 ) ) ;
#69074 = CARTESIAN_POINT ( 'NONE',  ( 4.243569643749999010, 11.51562500061451644, 27.54997392385601174 ) ) ;
#69075 = CARTESIAN_POINT ( 'NONE',  ( 13.98750000122903359, -4.330127018922194537, 2.499999999999995559 ) ) ;
#69076 = CARTESIAN_POINT ( 'NONE',  ( 25.77187500061451075, 3.027376345333611329, 5.243569643749999010 ) ) ;
#69077 = ORIENTED_EDGE ( 'NONE', *, *, #50916, .F. ) ;
#69078 = CARTESIAN_POINT ( 'NONE',  ( 18.96562500061451573, 3.027376345333611329, 5.243569643749999010 ) ) ;
#69079 = CARTESIAN_POINT ( 'NONE',  ( 19.88437500061451857, 4.541064518000418104, 2.621784821874999949 ) ) ;
#69080 = CARTESIAN_POINT ( 'NONE',  ( 4.125000000000000000, 6.123233995736764310E-16, -4.999999999999998224 ) ) ;
#69081 = CARTESIAN_POINT ( 'NONE',  ( 7.378125000614518036, -4.541064518000419881, 2.621784821874995952 ) ) ;
#69082 = CARTESIAN_POINT ( 'NONE',  ( 21.62812500061451360, 4.541064518000418104, 2.621784821874999949 ) ) ;
#69083 = CARTESIAN_POINT ( 'NONE',  ( 12.83437500061451786, -4.541064518000419881, 2.621784821874995952 ) ) ;
#69084 = CARTESIAN_POINT ( 'NONE',  ( 17.18437500061451573, 4.541064518000418104, 2.621784821874999949 ) ) ;
#69085 = CARTESIAN_POINT ( 'NONE',  ( -4.243569643749999898, 14.36562500061451786, 27.54997392385601529 ) ) ;
#69086 = CARTESIAN_POINT ( 'NONE',  ( 20.06250000122903643, 4.330127018922192761, -2.499999999999997780 ) ) ;
#69087 = CARTESIAN_POINT ( 'NONE',  ( 15.45937500061451608, 0.000000000000000000, 4.756430356249998326 ) ) ;
#69088 = CARTESIAN_POINT ( 'NONE',  ( 10.41562500061451679, 3.027376345333611329, 5.243569643749999010 ) ) ;
#69089 = CARTESIAN_POINT ( 'NONE',  ( 3.909375000614518481, -4.541064518000417216, -2.621784821875001281 ) ) ;
#69090 = CARTESIAN_POINT ( 'NONE',  ( 3.121875000614518836, 3.027376345333613106, -5.243569643749998122 ) ) ;
#69091 = CARTESIAN_POINT ( 'NONE',  ( 25.80937500061451928, 0.000000000000000000, 5.243569643749999010 ) ) ;
#69092 = CARTESIAN_POINT ( 'NONE',  ( 17.69062500061451715, -3.027376345333614438, 5.243569643749998122 ) ) ;
#69093 = CARTESIAN_POINT ( 'NONE',  ( 26.13750000122903216, -4.330127018922194537, 2.499999999999995559 ) ) ;
#69094 = CARTESIAN_POINT ( 'NONE',  ( 25.00312500061451715, -4.541064518000417216, -2.621784821875001281 ) ) ;
#69095 = CARTESIAN_POINT ( 'NONE',  ( 21.04687500061451644, -3.027376345333610441, -5.243569643749999898 ) ) ;
#69096 = CARTESIAN_POINT ( 'NONE',  ( 16.86562500061451786, -6.054752690667223547, -1.112240025338166033E-15 ) ) ;
#69097 = CARTESIAN_POINT ( 'NONE',  ( -3.000416591977282496E-16, 17.04687500061451644, 25.09994784771203058 ) ) ;
#69098 = VECTOR ( 'NONE', #26180, 1000.000000000000000 ) ;
#69099 = CARTESIAN_POINT ( 'NONE',  ( 23.24062500061451786, -3.027376345333610441, -5.243569643749999898 ) ) ;
#69100 = CARTESIAN_POINT ( 'NONE',  ( 2.775000001229033675, -5.773502691896255534, -1.060575238724906372E-15 ) ) ;
#69101 = EDGE_LOOP ( 'NONE', ( #41383, #8548, #72964, #53551 ) ) ;
#69102 = CARTESIAN_POINT ( 'NONE',  ( 26.43750000000000000, -2.886751345948129988, 4.999999999999997335 ) ) ;
#69103 = CARTESIAN_POINT ( 'NONE',  ( -2.000000000000000000, 12.72499999999999964, -33.46410161513775705 ) ) ;
#69104 = CARTESIAN_POINT ( 'NONE',  ( -1.878215178125001827, 20.70312499938548001, 33.25316411605952283 ) ) ;
#69105 = CARTESIAN_POINT ( 'NONE',  ( 3.196875000614516793, 6.054752690667223547, 3.707466751127219781E-16 ) ) ;
#69106 = CARTESIAN_POINT ( 'NONE',  ( 11.35312500061451679, 0.000000000000000000, 5.243569643749999010 ) ) ;
#69107 = CARTESIAN_POINT ( 'NONE',  ( 21.75000000122903288, -2.886751345948125991, -5.000000000000000000 ) ) ;
#69108 = AXIS2_PLACEMENT_3D ( 'NONE', #38448, #60974, #10374 ) ;
#69109 = EDGE_CURVE ( 'NONE', #26440, #18523, #66494, .T. ) ;
#69110 = CARTESIAN_POINT ( 'NONE',  ( 26.46562500061451573, 3.027376345333613106, -5.243569643749998122 ) ) ;
#69111 = CARTESIAN_POINT ( 'NONE',  ( 25.38749999999999929, 5.773502691896255534, 3.535250795749688894E-16 ) ) ;
#69112 = CARTESIAN_POINT ( 'NONE',  ( 3.999999999999999112, 16.73750000122903359, -30.00000000000000000 ) ) ;
#69113 = CARTESIAN_POINT ( 'NONE',  ( -3.999999999999999112, 15.61250000122903359, -30.00000000000000000 ) ) ;
#69114 = CARTESIAN_POINT ( 'NONE',  ( 10.97812500061451679, -4.541064518000419881, 2.621784821874995952 ) ) ;
#69115 = ORIENTED_EDGE ( 'NONE', *, *, #68939, .F. ) ;
#69116 = CARTESIAN_POINT ( 'NONE',  ( 26.20312500061451644, 0.000000000000000000, 5.243569643749999010 ) ) ;
#69117 = CARTESIAN_POINT ( 'NONE',  ( 6.703125000614516438, 4.541064518000418104, -2.621784821874998173 ) ) ;
#69118 = PRODUCT_DEFINITION_CONTEXT ( 'detailed design', #38961, 'design' ) ;
#69119 = VECTOR ( 'NONE', #12272, 1000.000000000000000 ) ;
#69120 = CARTESIAN_POINT ( 'NONE',  ( 3.928125000614516527, 6.421520780324663323E-16, -5.243569643749999010 ) ) ;
#69121 = CARTESIAN_POINT ( 'NONE',  ( 15.30937500061451750, 4.119189519843966529, -2.378215178124998275 ) ) ;
#69122 = DIRECTION ( 'NONE',  ( -1.000000000000000000, -0.000000000000000000, -0.000000000000000000 ) ) ;
#69123 = CARTESIAN_POINT ( 'NONE',  ( 12.93750000000000178, -2.886751345948129988, 4.999999999999997335 ) ) ;
#69124 = CARTESIAN_POINT ( 'NONE',  ( 13.47187500061451537, 3.027376345333613106, -5.243569643749998122 ) ) ;
#69125 = CARTESIAN_POINT ( 'NONE',  ( 11.66250000122903430, 0.000000000000000000, 4.999999999999998224 ) ) ;
#69126 = CARTESIAN_POINT ( 'NONE',  ( 16.54687500061451644, -3.027376345333610441, -5.243569643749999898 ) ) ;
#69127 = CARTESIAN_POINT ( 'NONE',  ( 17.32499999999999929, 4.330127018922191873, 2.499999999999999556 ) ) ;
#69128 = CARTESIAN_POINT ( 'NONE',  ( 9.196875000614518569, -3.027376345333614438, 5.243569643749998122 ) ) ;
#69129 = CARTESIAN_POINT ( 'NONE',  ( 9.001249775931846008E-16, 12.71562500061451750, -25.09994784771203058 ) ) ;
#69130 = CARTESIAN_POINT ( 'NONE',  ( 7.275000000000000355, 6.123233995736764310E-16, -4.999999999999998224 ) ) ;
#69131 = CARTESIAN_POINT ( 'NONE',  ( 22.84687500061451360, 4.119189519843966529, -2.378215178124998275 ) ) ;
#69132 = ORIENTED_EDGE ( 'NONE', *, *, #4558, .F. ) ;
#69133 = CARTESIAN_POINT ( 'NONE',  ( 24.40312500061451573, 0.000000000000000000, 5.243569643749999010 ) ) ;
#69134 = CARTESIAN_POINT ( 'NONE',  ( 26.58749999999999858, -2.886751345948126435, -5.000000000000000000 ) ) ;
#69135 = CARTESIAN_POINT ( 'NONE',  ( 28.13437500061451502, -4.541064518000419881, 2.621784821874995952 ) ) ;
#69136 = CARTESIAN_POINT ( 'NONE',  ( 23.66250000000000142, 2.886751345948126879, 4.999999999999999112 ) ) ;
#69137 = CARTESIAN_POINT ( 'NONE',  ( 7.528125000614515727, 6.421520780324663323E-16, -5.243569643749999010 ) ) ;
#69138 = CARTESIAN_POINT ( 'NONE',  ( 25.73437500061451644, -2.746126346562646425, 4.756430356249996549 ) ) ;
#69139 = CARTESIAN_POINT ( 'NONE',  ( 18.30937500061451928, -4.541064518000417216, -2.621784821875001281 ) ) ;
#69140 = CARTESIAN_POINT ( 'NONE',  ( 10.17187500061451644, 5.824947211148865298E-16, -4.756430356249998326 ) ) ;
#69141 = CARTESIAN_POINT ( 'NONE',  ( 29.47500000122903430, 2.886751345948129099, -4.999999999999998224 ) ) ;
#69142 = CARTESIAN_POINT ( 'NONE',  ( 9.009375000614518569, 4.541064518000418104, -2.621784821874998173 ) ) ;
#69143 = ORIENTED_EDGE ( 'NONE', *, *, #5554, .T. ) ;
#69144 = CARTESIAN_POINT ( 'NONE',  ( 18.04687500061451999, 6.054752690667223547, 3.707466751127219781E-16 ) ) ;
#69145 = CARTESIAN_POINT ( 'NONE',  ( 16.68750000000000000, -2.886751345948126435, -5.000000000000000000 ) ) ;
#69146 = CARTESIAN_POINT ( 'NONE',  ( 27.11249999999999716, 2.886751345948129099, -4.999999999999998224 ) ) ;
#69147 = CARTESIAN_POINT ( 'NONE',  ( 28.58437500061451786, -4.541064518000419881, 2.621784821874995952 ) ) ;
#69148 = CARTESIAN_POINT ( 'NONE',  ( 26.41875000122903216, 2.886751345948126879, 4.999999999999998224 ) ) ;
#69149 = DIRECTION ( 'NONE',  ( -1.000000000000000000, -0.000000000000000000, -0.000000000000000000 ) ) ;
#69150 = ORIENTED_EDGE ( 'NONE', *, *, #50466, .T. ) ;
#69151 = CARTESIAN_POINT ( 'NONE',  ( 10.83750000000000036, -2.886751345948125991, -5.000000000000000000 ) ) ;
#69152 = CARTESIAN_POINT ( 'NONE',  ( 12.83437500061451786, -2.746126346562642428, -4.756430356249999214 ) ) ;
#69153 = CARTESIAN_POINT ( 'NONE',  ( 23.87812500061451715, 4.541064518000418104, 2.621784821874999949 ) ) ;
#69154 = CARTESIAN_POINT ( 'NONE',  ( 13.04999999999999893, -4.330127018922190985, -2.500000000000001332 ) ) ;
#69155 = CARTESIAN_POINT ( 'NONE',  ( 8.437500001229034652, 4.330127018922191873, 2.499999999999999556 ) ) ;
#69156 = CARTESIAN_POINT ( 'NONE',  ( 7.003125000614518036, -4.541064518000417216, -2.621784821875001281 ) ) ;
#69157 =( BOUNDED_CURVE ( )  B_SPLINE_CURVE ( 2, ( #23609, #24694, #63851, #58670, #736, #17691, #34693 ),
 .UNSPECIFIED., .F., .F. ) 
 B_SPLINE_CURVE_WITH_KNOTS ( ( 3, 2, 2, 3 ),
 ( 0.05000000000000005135, 0.05333333333333338533, 0.05666666666666670543, 0.06000000000000003941 ),
 .UNSPECIFIED. ) 
 CURVE ( )  GEOMETRIC_REPRESENTATION_ITEM ( )  RATIONAL_B_SPLINE_CURVE ( ( 0.9999999999999981126, 0.8660254037844407060, 1.000000000000000000, 0.8660254037844387076, 1.000000000000000000, 0.8660254037844370423, 1.000000000000001776 ) ) 
 REPRESENTATION_ITEM ( '' )  );
#69158 = CARTESIAN_POINT ( 'NONE',  ( 20.99999999999999645, 0.000000000000000000, 4.999999999999998224 ) ) ;
#69159 = CARTESIAN_POINT ( 'NONE',  ( 21.02812500061451573, 6.421520780324663323E-16, -5.243569643749999010 ) ) ;
#69160 = CARTESIAN_POINT ( 'NONE',  ( 5.025000000000002132, 6.123233995736764310E-16, -4.999999999999998224 ) ) ;
#69161 = CARTESIAN_POINT ( 'NONE',  ( 25.53750000122903074, 4.330127018922191873, 2.499999999999999556 ) ) ;
#69162 = CARTESIAN_POINT ( 'NONE',  ( 1.878215178124997609, 17.96562499938548285, 33.25316411605952993 ) ) ;
#69163 = CARTESIAN_POINT ( 'NONE',  ( 3.975000000000002753, -4.330127018922194537, 2.499999999999995559 ) ) ;
#69164 = ORIENTED_EDGE ( 'NONE', *, *, #51006, .T. ) ;
#69165 = CARTESIAN_POINT ( 'NONE',  ( 22.04062500061451502, 6.054752690667223547, 3.707466751127219781E-16 ) ) ;
#69166 = CARTESIAN_POINT ( 'NONE',  ( 27.51562500061451644, 3.027376345333611329, 5.243569643749999010 ) ) ;
#69167 = CARTESIAN_POINT ( 'NONE',  ( 27.49687500061451217, 6.054752690667223547, 3.707466751127219781E-16 ) ) ;
#69168 = CARTESIAN_POINT ( 'NONE',  ( 13.79062500061451502, -3.027376345333610441, -5.243569643749999898 ) ) ;
#69169 = CARTESIAN_POINT ( 'NONE',  ( -3.000416591977282496E-16, 10.24062500061459069, -34.90005215228797653 ) ) ;
#69170 = CARTESIAN_POINT ( 'NONE',  ( 26.32500000122903216, 2.886751345948129099, -4.999999999999998224 ) ) ;
#69171 = CARTESIAN_POINT ( 'NONE',  ( 21.23437500061451644, 4.119189519843966529, 2.378215178124999607 ) ) ;
#69172 = CARTESIAN_POINT ( 'NONE',  ( 17.87812500061451715, 6.421520780324663323E-16, -5.243569643749999010 ) ) ;
#69173 = CARTESIAN_POINT ( 'NONE',  ( 2.393811435568372112E-14, 19.08124999877097139, 34.00000000000000000 ) ) ;
#69174 = CARTESIAN_POINT ( 'NONE',  ( 5.962500001229033231, -4.330127018922190985, -2.500000000000001332 ) ) ;
#69175 = CARTESIAN_POINT ( 'NONE',  ( 10.92187500061451644, 3.027376345333611329, 5.243569643749999010 ) ) ;
#69176 = CARTESIAN_POINT ( 'NONE',  ( 11.70937500061451608, 4.541064518000418104, -2.621784821874998173 ) ) ;
#69177 = CARTESIAN_POINT ( 'NONE',  ( 18.94687500061451502, 6.054752690667223547, 3.707466751127219781E-16 ) ) ;
#69178 = VERTEX_POINT ( 'NONE', #66126 ) ;
#69179 = CARTESIAN_POINT ( 'NONE',  ( 0.000000000000000000, 4.999999999999998224, 0.000000000000000000 ) ) ;
#69180 = CARTESIAN_POINT ( 'NONE',  ( 24.89062500061451644, -3.027376345333614438, 5.243569643749998122 ) ) ;
#69181 = CARTESIAN_POINT ( 'NONE',  ( 19.50937500061451857, 0.000000000000000000, 5.243569643749999010 ) ) ;
#69182 = CARTESIAN_POINT ( 'NONE',  ( 23.80312500061451786, 4.541064518000418104, -2.621784821874998173 ) ) ;
#69183 = DIRECTION ( 'NONE',  ( -1.000000000000000000, -0.000000000000000000, -0.000000000000000000 ) ) ;
#69184 = CARTESIAN_POINT ( 'NONE',  ( 3.999999999999998668, 14.41250000000000142, 27.69059892324149175 ) ) ;
#69185 = CARTESIAN_POINT ( 'NONE',  ( 3.609375000614516882, 4.541064518000418104, -2.621784821874998173 ) ) ;
#69186 = CARTESIAN_POINT ( 'NONE',  ( 8.550000001229031810, -2.886751345948129988, 4.999999999999997335 ) ) ;
#69187 = CARTESIAN_POINT ( 'NONE',  ( 5.062500001229035540, -4.330127018922190985, -2.500000000000001332 ) ) ;
#69188 = CARTESIAN_POINT ( 'NONE',  ( 3.999999999999999112, 19.77500000000000213, -30.00000000000000000 ) ) ;
#69189 = CARTESIAN_POINT ( 'NONE',  ( 28.16250000122903074, 4.330127018922192761, -2.499999999999997780 ) ) ;
#69190 = CARTESIAN_POINT ( 'NONE',  ( -2.000000000000001776, 19.94374999877096499, 33.46410161513775705 ) ) ;
#69191 = CARTESIAN_POINT ( 'NONE',  ( 10.54687500061451644, -3.027376345333614438, 5.243569643749998122 ) ) ;
#69192 = DIRECTION ( 'NONE',  ( -1.000000000000000000, -0.000000000000000000, -0.000000000000000000 ) ) ;
#69193 = CARTESIAN_POINT ( 'NONE',  ( 16.67812500061451786, 4.541064518000418104, 2.621784821874999949 ) ) ;
#69194 = CARTESIAN_POINT ( 'NONE',  ( 10.73437500061451644, 6.421520780324663323E-16, -5.243569643749999010 ) ) ;
#69195 = CARTESIAN_POINT ( 'NONE',  ( 3.515625000614516882, 3.027376345333613106, -5.243569643749998122 ) ) ;
#69196 = CARTESIAN_POINT ( 'NONE',  ( 18.60937500061451644, 0.000000000000000000, 5.243569643749999010 ) ) ;
#69197 = CARTESIAN_POINT ( 'NONE',  ( 7.621875000614519280, 3.027376345333613106, -5.243569643749998122 ) ) ;
#69198 = CARTESIAN_POINT ( 'NONE',  ( 3.045726060920115774, -3.965322109520783567, -3.366821969667765035 ) ) ;
#69199 = CARTESIAN_POINT ( 'NONE',  ( 30.00000000000000000, 6.123233995736764310E-16, -4.999999999999998224 ) ) ;
#69200 = CARTESIAN_POINT ( 'NONE',  ( 8.803125000614517859, -4.541064518000417216, -2.621784821875001281 ) ) ;
#69201 = CARTESIAN_POINT ( 'NONE',  ( 17.16562500061451502, 3.027376345333611329, 5.243569643749999010 ) ) ;
#69202 = EDGE_CURVE ( 'NONE', #38080, #64135, #15505, .T. ) ;
#69203 = EDGE_LOOP ( 'NONE', ( #72332, #3462, #22428, #63304 ) ) ;
#69204 = CARTESIAN_POINT ( 'NONE',  ( 5.737500001229033586, 4.330127018922191873, 2.499999999999999556 ) ) ;
#69205 = CARTESIAN_POINT ( 'NONE',  ( 15.29062500061451679, 6.054752690667223547, 3.707466751127219781E-16 ) ) ;
#69206 = AXIS2_PLACEMENT_3D ( 'NONE', #57648, #41754, #14036 ) ;
#69207 = CARTESIAN_POINT ( 'NONE',  ( 12.02812500061451573, 6.421520780324663323E-16, -5.243569643749999010 ) ) ;
#69208 = CARTESIAN_POINT ( 'NONE',  ( 22.65937500061451715, 0.000000000000000000, 4.756430356249998326 ) ) ;
#69209 = CARTESIAN_POINT ( 'NONE',  ( 13.08750000000000036, -2.886751345948125991, -5.000000000000000000 ) ) ;
#69210 = CARTESIAN_POINT ( 'NONE',  ( 7.125000001229033764, 2.886751345948126879, 4.999999999999999112 ) ) ;
#69211 = CARTESIAN_POINT ( 'NONE',  ( 25.16250000122903074, 0.000000000000000000, 4.999999999999998224 ) ) ;
#69212 = CARTESIAN_POINT ( 'NONE',  ( 14.89687500061451786, 6.054752690667223547, 3.707466751127219781E-16 ) ) ;
#69213 = CARTESIAN_POINT ( 'NONE',  ( 17.43750000122903288, 4.330127018922191873, 2.499999999999999556 ) ) ;
#69214 = CARTESIAN_POINT ( 'NONE',  ( 25.68750000000000000, -2.886751345948125991, -5.000000000000000000 ) ) ;
#69215 = CARTESIAN_POINT ( 'NONE',  ( 4.243569643749999010, 18.71562500061451217, -32.45002607614398471 ) ) ;
#69216 = CARTESIAN_POINT ( 'NONE',  ( -2.672702088255949472E-15, 13.06250000000000355, 26.00000000000000000 ) ) ;
#69217 = DIRECTION ( 'NONE',  ( -0.000000000000000000, -1.000000000000000000, -0.000000000000000000 ) ) ;
#69218 = FACE_OUTER_BOUND ( 'NONE', #31062, .T. ) ;
#69219 = CARTESIAN_POINT ( 'NONE',  ( 17.70937500061451431, 0.000000000000000000, 5.243569643749999010 ) ) ;
#69220 = CARTESIAN_POINT ( 'NONE',  ( 0.000000000000000000, 20.00000000000000000, -33.99999999999999289 ) ) ;
#69221 = CARTESIAN_POINT ( 'NONE',  ( 14.31562500061451537, 3.027376345333613106, -5.243569643749998122 ) ) ;
#69222 = CARTESIAN_POINT ( 'NONE',  ( 10.10625000122903216, 4.330127018922192761, -2.499999999999997780 ) ) ;
#69223 = CARTESIAN_POINT ( 'NONE',  ( 9.074999999999999289, 6.123233995736764310E-16, -4.999999999999998224 ) ) ;
#69224 = CARTESIAN_POINT ( 'NONE',  ( 26.22187500061451715, 3.027376345333611329, 5.243569643749999010 ) ) ;
#69225 = CARTESIAN_POINT ( 'NONE',  ( 18.49687500061451573, 0.000000000000000000, 4.756430356249998326 ) ) ;
#69226 = CARTESIAN_POINT ( 'NONE',  ( 11.24062500061451608, 6.054752690667223547, 3.707466751127219781E-16 ) ) ;
#69227 = CARTESIAN_POINT ( 'NONE',  ( 16.20937500061451786, 4.541064518000418104, -2.621784821874998173 ) ) ;
#69228 = ORIENTED_EDGE ( 'NONE', *, *, #19299, .T. ) ;
#69229 = CARTESIAN_POINT ( 'NONE',  ( 27.51562500061451644, 3.027376345333611329, 5.243569643749999010 ) ) ;
#69230 = CARTESIAN_POINT ( 'NONE',  ( 21.32812500061451644, -4.541064518000419881, 2.621784821874995952 ) ) ;
#69231 = CARTESIAN_POINT ( 'NONE',  ( 29.39062500061451289, -3.027376345333614438, 5.243569643749998122 ) ) ;
#69232 = CARTESIAN_POINT ( 'NONE',  ( -1.071796769724491005, 14.17009619066136672, -34.00000000000000000 ) ) ;
#69233 = CARTESIAN_POINT ( 'NONE',  ( 9.937500000000001776, -2.886751345948125991, -5.000000000000000000 ) ) ;
#69234 = CARTESIAN_POINT ( 'NONE',  ( 18.26250000122903216, 4.330127018922192761, -2.499999999999997780 ) ) ;
#69235 = CARTESIAN_POINT ( 'NONE',  ( 3.752440054025286909, -3.304420318444254878, 4.071342403668507082 ) ) ;
#69236 = CARTESIAN_POINT ( 'NONE',  ( 9.946875000614516793, 0.000000000000000000, 4.756430356249998326 ) ) ;
#69237 = VERTEX_POINT ( 'NONE', #16240 ) ;
#69238 = CARTESIAN_POINT ( 'NONE',  ( 17.32499999999999929, 4.330127018922191873, 2.499999999999999556 ) ) ;
#69239 = CARTESIAN_POINT ( 'NONE',  ( 20.81250000000000000, 2.886751345948129099, -4.999999999999998224 ) ) ;
#69240 = CARTESIAN_POINT ( 'NONE',  ( 18.38437500061451857, 6.421520780324663323E-16, -5.243569643749999010 ) ) ;
#69241 = CARTESIAN_POINT ( 'NONE',  ( 25.56562500061452070, 3.027376345333613106, -5.243569643749998122 ) ) ;
#69242 = VERTEX_POINT ( 'NONE', #56140 ) ;
#69243 = CARTESIAN_POINT ( 'NONE',  ( 13.64999999999999858, 4.330127018922192761, -2.499999999999997780 ) ) ;
#69244 = CARTESIAN_POINT ( 'NONE',  ( 5.840625000614516615, 6.054752690667223547, 3.707466751127219781E-16 ) ) ;
#69245 = CARTESIAN_POINT ( 'NONE',  ( 3.250662400336420177, 3.799104362746421604, 3.614115195980558415 ) ) ;
#69246 = CARTESIAN_POINT ( 'NONE',  ( 12.33750000000000036, 5.773502691896255534, 3.535250795749688894E-16 ) ) ;
#69247 = CARTESIAN_POINT ( 'NONE',  ( 2.121784821874999061, 16.50312500061451715, 26.32496088578401583 ) ) ;
#69248 = CARTESIAN_POINT ( 'NONE',  ( 28.37812500061451715, 4.541064518000418104, 2.621784821874999949 ) ) ;
#69249 = CARTESIAN_POINT ( 'NONE',  ( 9.937500000000001776, -2.886751345948125991, -5.000000000000000000 ) ) ;
#69250 = CARTESIAN_POINT ( 'NONE',  ( 3.756430356250000546, 18.52812499938548285, 27.83122392262697886 ) ) ;
#69251 = CARTESIAN_POINT ( 'NONE',  ( 26.74687500061451573, -3.027376345333614438, 5.243569643749998122 ) ) ;
#69252 = ORIENTED_EDGE ( 'NONE', *, *, #65786, .F. ) ;
#69253 = CARTESIAN_POINT ( 'NONE',  ( 22.11562500061451786, 3.027376345333611329, 5.243569643749999010 ) ) ;
#69254 = CARTESIAN_POINT ( 'NONE',  ( 22.77187500061451786, -6.054752690667223547, -1.112240025338166033E-15 ) ) ;
#69255 = CARTESIAN_POINT ( 'NONE',  ( -2.121784821874999949, 16.12812500061459176, -33.67503911421598417 ) ) ;
#69256 = CARTESIAN_POINT ( 'NONE',  ( 5.803125000614517859, 4.541064518000418104, -2.621784821874998173 ) ) ;
#69257 = CARTESIAN_POINT ( 'NONE',  ( 28.99687500061451573, -2.746126346562646425, 4.756430356249996549 ) ) ;
#69258 = CARTESIAN_POINT ( 'NONE',  ( 23.99062500061451786, -3.027376345333614438, 5.243569643749998122 ) ) ;
#69259 = CARTESIAN_POINT ( 'NONE',  ( 27.15937500061451360, -5.492252693125287522, -1.008910452111647106E-15 ) ) ;
#69260 = CARTESIAN_POINT ( 'NONE',  ( 13.39687500061451608, -2.746126346562642428, -4.756430356249999214 ) ) ;
#69261 = CARTESIAN_POINT ( 'NONE',  ( 16.20937500061451786, 4.541064518000418104, -2.621784821874998173 ) ) ;
#69262 = CARTESIAN_POINT ( 'NONE',  ( 18.98437500061451644, 4.541064518000418104, 2.621784821874999949 ) ) ;
#69263 = CARTESIAN_POINT ( 'NONE',  ( 26.89687500061451431, -3.027376345333610441, -5.243569643749999898 ) ) ;
#69264 = CARTESIAN_POINT ( 'NONE',  ( -4.243569643749999898, 17.57187500061451502, 27.54997392385601529 ) ) ;
#69265 = CARTESIAN_POINT ( 'NONE',  ( 6.853125000614516793, 0.000000000000000000, 5.243569643749999010 ) ) ;
#69266 = DIRECTION ( 'NONE',  ( -1.000000000000000000, -0.000000000000000000, -0.000000000000000000 ) ) ;
#69267 = CARTESIAN_POINT ( 'NONE',  ( 5.146875000614517859, -3.027376345333614438, 5.243569643749998122 ) ) ;
#69268 = CARTESIAN_POINT ( 'NONE',  ( 26.47499999999999787, -4.330127018922194537, 2.499999999999995559 ) ) ;
#69269 = CARTESIAN_POINT ( 'NONE',  ( 5.990625000614517859, -3.027376345333614438, 5.243569643749998122 ) ) ;
#69270 = CARTESIAN_POINT ( 'NONE',  ( 9.609375000614518214, 0.000000000000000000, 5.243569643749999010 ) ) ;
#69271 = FILL_AREA_STYLE_COLOUR ( '', #60310 ) ;
#69272 = CARTESIAN_POINT ( 'NONE',  ( 16.16250000122903430, 0.000000000000000000, 4.999999999999998224 ) ) ;
#69273 = CARTESIAN_POINT ( 'NONE',  ( 6.084375000614518747, -4.541064518000419881, 2.621784821874995952 ) ) ;
#69274 = CARTESIAN_POINT ( 'NONE',  ( 8.090625000614515727, 6.054752690667223547, 3.707466751127219781E-16 ) ) ;
#69275 = CARTESIAN_POINT ( 'NONE',  ( 2.000000000000000444, 12.96874999877096712, 26.53589838486224650 ) ) ;
#69276 = CARTESIAN_POINT ( 'NONE',  ( 23.90625000122903288, -4.330127018922190985, -2.500000000000001332 ) ) ;
#69277 = CARTESIAN_POINT ( 'NONE',  ( 17.85937500061451999, -4.541064518000417216, -2.621784821875001281 ) ) ;
#69278 = CARTESIAN_POINT ( 'NONE',  ( 22.61249999999999361, 2.886751345948101122, -5.000000000000046185 ) ) ;
#69279 = VERTEX_POINT ( 'NONE', #21415 ) ;
#69280 = CARTESIAN_POINT ( 'NONE',  ( 24.77812500061451217, 4.541064518000418104, 2.621784821874999949 ) ) ;
#69281 = CARTESIAN_POINT ( 'NONE',  ( 9.778125000614517504, 6.421520780324663323E-16, -5.243569643749999010 ) ) ;
#69282 = CARTESIAN_POINT ( 'NONE',  ( 26.22187500061451715, 3.027376345333611329, 5.243569643749999010 ) ) ;
#69283 = CARTESIAN_POINT ( 'NONE',  ( 10.15312500061451750, -4.541064518000417216, -2.621784821875001281 ) ) ;
#69284 = CARTESIAN_POINT ( 'NONE',  ( 29.09999999999999787, 0.000000000000000000, 4.999999999999998224 ) ) ;
#69285 = CARTESIAN_POINT ( 'NONE',  ( 10.91250000122903252, -4.330127018922190985, -2.500000000000001332 ) ) ;
#69286 = CARTESIAN_POINT ( 'NONE',  ( 24.92812500061451431, -4.541064518000419881, 2.621784821874995952 ) ) ;
#69287 = ADVANCED_FACE ( 'NONE', ( #49873 ), #22152, .T. ) ;
#69288 = CARTESIAN_POINT ( 'NONE',  ( -4.243569643749999898, 13.50312500061451715, -30.00000000000000000 ) ) ;
#69289 = CARTESIAN_POINT ( 'NONE',  ( 12.56250000122903465, 0.000000000000000000, 4.999999999999998224 ) ) ;
#69290 = CARTESIAN_POINT ( 'NONE',  ( 21.70312500061451644, 0.000000000000000000, 5.243569643749999010 ) ) ;
#69291 = CARTESIAN_POINT ( 'NONE',  ( 10.83750000000000036, -2.886751345948125991, -5.000000000000000000 ) ) ;
#69292 = CARTESIAN_POINT ( 'NONE',  ( 20.99062500061451431, -3.027376345333610441, -5.243569643749999898 ) ) ;
#69293 = CARTESIAN_POINT ( 'NONE',  ( 6.121875000614517504, -6.054752690667223547, -1.112240025338166033E-15 ) ) ;
#69294 = CARTESIAN_POINT ( 'NONE',  ( 20.88749999999999929, 5.773502691896255534, 3.535250795749688894E-16 ) ) ;
#69295 = CARTESIAN_POINT ( 'NONE',  ( 14.51250000122903394, -4.330127018922190985, -2.500000000000001332 ) ) ;
#69296 = VECTOR ( 'NONE', #3736, 1000.000000000000000 ) ;
#69297 = CARTESIAN_POINT ( 'NONE',  ( 10.22812500061451679, 6.421520780324663323E-16, -5.243569643749999010 ) ) ;
#69298 = CARTESIAN_POINT ( 'NONE',  ( 16.97812500061451502, 6.421520780324663323E-16, -5.243569643749999010 ) ) ;
#69299 = CARTESIAN_POINT ( 'NONE',  ( 24.75000000122902932, -2.886751345948129988, 4.999999999999997335 ) ) ;
#69300 = CARTESIAN_POINT ( 'NONE',  ( 22.43437500061451573, 6.421520780324663323E-16, -5.243569643749999010 ) ) ;
#69301 = DIRECTION ( 'NONE',  ( 0.000000000000000000, 0.000000000000000000, 1.000000000000000000 ) ) ;
#69302 = CARTESIAN_POINT ( 'NONE',  ( 8.212500001229035007, -4.330127018922190985, -2.500000000000001332 ) ) ;
#69303 = CARTESIAN_POINT ( 'NONE',  ( 9.159375000614515372, 0.000000000000000000, 5.243569643749999010 ) ) ;
#69304 = CARTESIAN_POINT ( 'NONE',  ( 25.80937500061451928, 0.000000000000000000, 5.243569643749999010 ) ) ;
#69305 =( BOUNDED_CURVE ( )  B_SPLINE_CURVE ( 2, ( #56636, #33380, #50385, #55916, #72910, #36914, #35546 ),
 .UNSPECIFIED., .F., .F. ) 
 B_SPLINE_CURVE_WITH_KNOTS ( ( 3, 2, 2, 3 ),
 ( 0.9699999999999999734, 0.9733333333333333837, 0.9766666666666666829, 0.9799999999999999822 ),
 .UNSPECIFIED. ) 
 CURVE ( )  GEOMETRIC_REPRESENTATION_ITEM ( )  RATIONAL_B_SPLINE_CURVE ( ( 1.000000000000000000, 0.8660254037844387076, 1.000000000000000000, 0.8660254037844387076, 1.000000000000000000, 0.8660254037844387076, 1.000000000000000000 ) ) 
 REPRESENTATION_ITEM ( '' )  );
#69306 = CARTESIAN_POINT ( 'NONE',  ( 3.309375000614518836, 0.000000000000000000, 5.243569643749999010 ) ) ;
#69307 = CARTESIAN_POINT ( 'NONE',  ( 20.12812500061451715, 6.421520780324663323E-16, -5.243569643749999010 ) ) ;
#69308 = CARTESIAN_POINT ( 'NONE',  ( 27.42187500061451644, 3.027376345333613106, -5.243569643749998122 ) ) ;
#69309 = CARTESIAN_POINT ( 'NONE',  ( 2.655984681222220721E-16, 17.81562499938548427, 25.66244784525396483 ) ) ;
#69310 = FACE_OUTER_BOUND ( 'NONE', #69584, .T. ) ;
#69311 = CARTESIAN_POINT ( 'NONE',  ( 8.034375000614518925, 6.421520780324663323E-16, -5.243569643749999010 ) ) ;
#69312 = CARTESIAN_POINT ( 'NONE',  ( 16.97812500061451502, 6.421520780324663323E-16, -5.243569643749999010 ) ) ;
#69313 = ORIENTED_EDGE ( 'NONE', *, *, #33946, .F. ) ;
#69314 = DIRECTION ( 'NONE',  ( 0.000000000000000000, 0.000000000000000000, -1.000000000000000000 ) ) ;
#69315 = CARTESIAN_POINT ( 'NONE',  ( 28.60312500061451502, -4.541064518000417216, -2.621784821875001281 ) ) ;
#69316 = CARTESIAN_POINT ( 'NONE',  ( 3.271875000614519635, 3.027376345333611329, 5.243569643749999010 ) ) ;
#69317 = CARTESIAN_POINT ( 'NONE',  ( 45.00000000000000000, 6.123233995736764310E-16, -4.999999999999998224 ) ) ;
#69318 = CARTESIAN_POINT ( 'NONE',  ( 3.714721736615232306, 3.346823739705472089, -3.745147025001839491 ) ) ;
#69319 = CARTESIAN_POINT ( 'NONE',  ( 15.90000000000000036, 4.330127018922192761, -2.499999999999997780 ) ) ;
#69320 = CARTESIAN_POINT ( 'NONE',  ( 20.24062500061451431, 6.054752690667223547, 3.707466751127219781E-16 ) ) ;
#69321 = ORIENTED_EDGE ( 'NONE', *, *, #59108, .F. ) ;
#69322 = CARTESIAN_POINT ( 'NONE',  ( 24.67500000000000071, -4.330127018922194537, 2.499999999999995559 ) ) ;
#69323 = CARTESIAN_POINT ( 'NONE',  ( 26.44687500061451502, -3.027376345333610441, -5.243569643749999898 ) ) ;
#69324 = EDGE_CURVE ( 'NONE', #24785, #44627, #9332, .T. ) ;
#69325 = ORIENTED_EDGE ( 'NONE', *, *, #46759, .F. ) ;
#69326 = CARTESIAN_POINT ( 'NONE',  ( 12.32812500061451821, -4.541064518000419881, 2.621784821874995952 ) ) ;
#69327 = CARTESIAN_POINT ( 'NONE',  ( 5.315625000614516260, 3.027376345333613106, -5.243569643749998122 ) ) ;
#69328 = CARTESIAN_POINT ( 'NONE',  ( 15.60937500061451644, 2.746126346562645981, -4.756430356249997438 ) ) ;
#69329 = CARTESIAN_POINT ( 'NONE',  ( 29.42812500061451431, -4.541064518000419881, 2.621784821874995952 ) ) ;
#69330 = EDGE_CURVE ( 'NONE', #48240, #66542, #72039, .T. ) ;
#69331 = CARTESIAN_POINT ( 'NONE',  ( 15.63750000122903216, 4.330127018922191873, 2.499999999999999556 ) ) ;
#69332 = CARTESIAN_POINT ( 'NONE',  ( 22.80000000000000071, 0.000000000000000000, 4.999999999999998224 ) ) ;
#69333 = CARTESIAN_POINT ( 'NONE',  ( 29.58749999999999858, -2.886751345948129988, 4.999999999999997335 ) ) ;
#69334 = CARTESIAN_POINT ( 'NONE',  ( 5.296875000614518214, -3.027376345333610441, -5.243569643749999898 ) ) ;
#69335 = CARTESIAN_POINT ( 'NONE',  ( 10.02187500061451964, 3.027376345333611329, 5.243569643749999010 ) ) ;
#69336 = CARTESIAN_POINT ( 'NONE',  ( 18.38437500061451857, 6.421520780324663323E-16, -5.243569643749999010 ) ) ;
#69337 = VERTEX_POINT ( 'NONE', #28421 ) ;
#69338 = CARTESIAN_POINT ( 'NONE',  ( 29.24062500061451431, 6.054752690667223547, 3.707466751127219781E-16 ) ) ;
#69339 = CARTESIAN_POINT ( 'NONE',  ( 29.70937500061451431, 4.541064518000418104, -2.621784821874998173 ) ) ;
#69340 = CARTESIAN_POINT ( 'NONE',  ( 3.984375000614517326, 6.421520780324663323E-16, -5.243569643749999010 ) ) ;
#69341 = CIRCLE ( 'NONE', #37489, 9.000000000000000000 ) ;
#69342 = CARTESIAN_POINT ( 'NONE',  ( 16.01249999999999929, 2.886751345948126879, 4.999999999999999112 ) ) ;
#69343 = CARTESIAN_POINT ( 'NONE',  ( 14.50312500061451537, 0.000000000000000000, 5.243569643749999010 ) ) ;
#69344 = CARTESIAN_POINT ( 'NONE',  ( 3.999999999999998668, 14.07500000122903749, 27.69059892324149530 ) ) ;
#69345 = CARTESIAN_POINT ( 'NONE',  ( 4.012500000000001954, -5.773502691896255534, -1.060575238724906372E-15 ) ) ;
#69346 = CARTESIAN_POINT ( 'NONE',  ( 21.90000000122903145, 5.773502691896255534, 3.535250795749688894E-16 ) ) ;
#69347 = CARTESIAN_POINT ( 'NONE',  ( -1.071796769724491005, 13.27009619066136636, 26.00000000000000355 ) ) ;
#69348 = CARTESIAN_POINT ( 'NONE',  ( 19.28437500061451360, 5.824947211148865298E-16, -4.756430356249998326 ) ) ;
#69349 = CARTESIAN_POINT ( 'NONE',  ( 8.728125000614518569, -4.541064518000419881, 2.621784821874995952 ) ) ;
#69350 = CARTESIAN_POINT ( 'NONE',  ( 24.34687500061451715, 6.054752690667223547, 3.707466751127219781E-16 ) ) ;
#69351 = EDGE_CURVE ( 'NONE', #60873, #62319, #60449, .T. ) ;
#69352 = CARTESIAN_POINT ( 'NONE',  ( -3.000416591977282496E-16, 19.29687500061451644, 25.09994784771203058 ) ) ;
#69353 = CARTESIAN_POINT ( 'NONE',  ( 26.33437500061451431, -4.541064518000419881, 2.621784821874995952 ) ) ;
#69354 = CARTESIAN_POINT ( 'NONE',  ( 8.250000000000000000, 4.330127018922192761, -2.499999999999997780 ) ) ;
#69355 = CARTESIAN_POINT ( 'NONE',  ( -3.999999999999999556, 13.77500000122903678, 27.69059892324149530 ) ) ;
#69356 = CARTESIAN_POINT ( 'NONE',  ( 14.16562500061451679, -6.054752690667223547, -1.112240025338166033E-15 ) ) ;
#69357 = CARTESIAN_POINT ( 'NONE',  ( 6.787500001229032520, -4.330127018922194537, 2.499999999999995559 ) ) ;
#69358 = CARTESIAN_POINT ( 'NONE',  ( 17.14687500061451786, 6.054752690667223547, 3.707466751127219781E-16 ) ) ;
#69359 = CARTESIAN_POINT ( 'NONE',  ( 11.10937500061451644, -4.541064518000417216, -2.621784821875001281 ) ) ;
#69360 = CARTESIAN_POINT ( 'NONE',  ( 1.071796769724489673, 13.88615380933863364, 26.00000000000000000 ) ) ;
#69361 = ORIENTED_EDGE ( 'NONE', *, *, #19740, .T. ) ;
#69362 = CARTESIAN_POINT ( 'NONE',  ( 11.46562500061451573, -6.054752690667223547, -1.112240025338166033E-15 ) ) ;
#69363 = FACE_OUTER_BOUND ( 'NONE', #11770, .T. ) ;
#69364 = CARTESIAN_POINT ( 'NONE',  ( 24.00000000122902932, -2.886751345948125991, -5.000000000000000000 ) ) ;
#69365 = CARTESIAN_POINT ( 'NONE',  ( 12.64687500061451608, 6.054752690667223547, 3.707466751127219781E-16 ) ) ;
#69366 = CARTESIAN_POINT ( 'NONE',  ( 13.79062500061451502, -3.027376345333610441, -5.243569643749999898 ) ) ;
#69367 = EDGE_CURVE ( 'NONE', #59457, #31892, #61669, .T. ) ;
#69368 = DIRECTION ( 'NONE',  ( 1.000000000000000000, 0.000000000000000000, 0.000000000000000000 ) ) ;
#69369 = CARTESIAN_POINT ( 'NONE',  ( 25.02187500061451431, -6.054752690667223547, -1.112240025338166033E-15 ) ) ;
#69370 = CARTESIAN_POINT ( 'NONE',  ( 45.00000000000000000, 0.000000000000000000, 4.999999999999998224 ) ) ;
#69371 =( BOUNDED_CURVE ( )  B_SPLINE_CURVE ( 2, ( #64111, #30508, #2430, #47496, #70027, #14236, #8700 ),
 .UNSPECIFIED., .F., .F. ) 
 B_SPLINE_CURVE_WITH_KNOTS ( ( 3, 2, 2, 3 ),
 ( 0.2583333333333333037, 0.2611111111111110716, 0.2638888888888888395, 0.2666666666666666075 ),
 .UNSPECIFIED. ) 
 CURVE ( )  GEOMETRIC_REPRESENTATION_ITEM ( )  RATIONAL_B_SPLINE_CURVE ( ( 1.000000000000002665, 0.8660254037844360431, 1.000000000000000000, 0.8660254037844387076, 1.000000000000000000, 0.8660254037844413721, 0.9999999999999973355 ) ) 
 REPRESENTATION_ITEM ( '' )  );
#69372 = CARTESIAN_POINT ( 'NONE',  ( 23.92499999999999716, 6.123233995736764310E-16, -4.999999999999998224 ) ) ;
#69373 = CARTESIAN_POINT ( 'NONE',  ( 45.00000000000000000, 0.000000000000000000, 0.000000000000000000 ) ) ;
#69374 = CARTESIAN_POINT ( 'NONE',  ( 2.121784821875001281, 15.95937500061451608, -26.32496088578401938 ) ) ;
#69375 = CARTESIAN_POINT ( 'NONE',  ( 15.12187500061451750, -6.054752690667223547, -1.112240025338166033E-15 ) ) ;
#69376 = CARTESIAN_POINT ( 'NONE',  ( 18.00000000122903288, -2.886751345948129988, 4.999999999999997335 ) ) ;
#69377 =( BOUNDED_CURVE ( )  B_SPLINE_CURVE ( 2, ( #30511, #47499, #63752, #7607, #13141, #8338, #7975 ),
 .UNSPECIFIED., .F., .F. ) 
 B_SPLINE_CURVE_WITH_KNOTS ( ( 3, 2, 2, 3 ),
 ( 0.7166666666666667851, 0.7194444444444445530, 0.7222222222222222099, 0.7249999999999999778 ),
 .UNSPECIFIED. ) 
 CURVE ( )  GEOMETRIC_REPRESENTATION_ITEM ( )  RATIONAL_B_SPLINE_CURVE ( ( 0.9999999999999946709, 0.8660254037844440367, 1.000000000000000000, 0.8660254037844387076, 1.000000000000000000, 0.8660254037844387076, 1.000000000000000000 ) ) 
 REPRESENTATION_ITEM ( '' )  );
#69378 = CARTESIAN_POINT ( 'NONE',  ( 11.52187500061451608, -6.054752690667223547, -1.112240025338166033E-15 ) ) ;
#69379 = CARTESIAN_POINT ( 'NONE',  ( 2.121784821875001281, 10.10937500061451821, 33.67503911421598417 ) ) ;
#69380 = CARTESIAN_POINT ( 'NONE',  ( 19.31250000122903288, 0.000000000000000000, 4.999999999999998224 ) ) ;
#69381 = CARTESIAN_POINT ( 'NONE',  ( 15.96562500061451573, -6.054752690667223547, -1.112240025338166033E-15 ) ) ;
#69382 = ORIENTED_EDGE ( 'NONE', *, *, #22708, .F. ) ;
#69383 = ORIENTED_EDGE ( 'NONE', *, *, #25554, .F. ) ;
#69384 = CARTESIAN_POINT ( 'NONE',  ( 17.81250000000000355, 2.886751345948126879, 4.999999999999999112 ) ) ;
#69385 = CARTESIAN_POINT ( 'NONE',  ( 4.000000000000000000, 14.30000000000000071, 30.00000000000000000 ) ) ;
#69386 = CARTESIAN_POINT ( 'NONE',  ( 12.45937500061451786, -4.541064518000417216, -2.621784821875001281 ) ) ;
#69387 = CARTESIAN_POINT ( 'NONE',  ( 3.009823169949401578, 3.992613741101768365, -3.171945278996665785 ) ) ;
#69388 = CARTESIAN_POINT ( 'NONE',  ( 13.38750000122903394, 4.330127018922191873, 2.499999999999999556 ) ) ;
#69389 = CARTESIAN_POINT ( 'NONE',  ( 21.03750000122903074, 4.330127018922191873, 2.499999999999999556 ) ) ;
#69390 = CARTESIAN_POINT ( 'NONE',  ( 18.74062500061451431, -3.027376345333610441, -5.243569643749999898 ) ) ;
#69391 = CARTESIAN_POINT ( 'NONE',  ( 22.15312500061451573, 0.000000000000000000, 5.243569643749999010 ) ) ;
#69392 = CARTESIAN_POINT ( 'NONE',  ( 3.365625000614516082, -6.054752690667223547, -1.112240025338166033E-15 ) ) ;
#69393 =( BOUNDED_CURVE ( )  B_SPLINE_CURVE ( 2, ( #14595, #37130, #59659, #13492, #24949, #9067, #53399 ),
 .UNSPECIFIED., .F., .T. ) 
 B_SPLINE_CURVE_WITH_KNOTS ( ( 3, 2, 2, 3 ),
 ( 0.06666666666666665186, 0.06944444444444443365, 0.07222222222222218768, 0.07499999999999996947 ),
 .UNSPECIFIED. ) 
 CURVE ( )  GEOMETRIC_REPRESENTATION_ITEM ( )  RATIONAL_B_SPLINE_CURVE ( ( 1.000000000000000666, 0.8660254037844379305, 1.000000000000000000, 0.8660254037844387076, 1.000000000000000000, 0.8660254037844400399, 0.9999999999999986677 ) ) 
 REPRESENTATION_ITEM ( '' )  );
#69394 = CARTESIAN_POINT ( 'NONE',  ( 27.48749999999999716, -2.886751345948125991, -5.000000000000000000 ) ) ;
#69395 = LINE ( 'NONE', #5873, #14778 ) ;
#69396 = CARTESIAN_POINT ( 'NONE',  ( 9.309375000614517504, -4.119189519843965641, -2.378215178125001383 ) ) ;
#69397 = CARTESIAN_POINT ( 'NONE',  ( 5.810221930991193690E-16, 18.01249999999999218, 26.00000000000000000 ) ) ;
#69398 = CARTESIAN_POINT ( 'NONE',  ( 4.243569643749999898, 15.58437500061451786, -30.00000000000000000 ) ) ;
#69399 = CARTESIAN_POINT ( 'NONE',  ( 2.700000001229035718, -2.886751345948129988, 4.999999999999997335 ) ) ;
#69400 = CARTESIAN_POINT ( 'NONE',  ( 6.112499999999999822, 2.886751345948126879, 4.999999999999999112 ) ) ;
#69401 = CARTESIAN_POINT ( 'NONE',  ( 2.393811435568372112E-14, 18.68750000000000355, 34.00000000000000000 ) ) ;
#69402 = CARTESIAN_POINT ( 'NONE',  ( 10.73437500061451644, 6.421520780324663323E-16, -5.243569643749999010 ) ) ;
#69403 = CARTESIAN_POINT ( 'NONE',  ( 27.62812500061451360, -4.541064518000419881, 2.621784821874995952 ) ) ;
#69404 = CARTESIAN_POINT ( 'NONE',  ( 0.000000000000000000, 20.00000000000000000, 30.00000000000000000 ) ) ;
#69405 = CARTESIAN_POINT ( 'NONE',  ( -5.376511845580211002, 8.433624770265602422, -32.69150760605022299 ) ) ;
#69406 = DIRECTION ( 'NONE',  ( 0.000000000000000000, 0.000000000000000000, -1.000000000000000000 ) ) ;
#69407 = CARTESIAN_POINT ( 'NONE',  ( 8.071875000614518569, 3.027376345333613106, -5.243569643749998122 ) ) ;
#69408 = CARTESIAN_POINT ( 'NONE',  ( 10.54687500061451644, -3.027376345333614438, 5.243569643749998122 ) ) ;
#69409 = CARTESIAN_POINT ( 'NONE',  ( 5.962500000000002132, 2.886751345948129099, -4.999999999999998224 ) ) ;
#69410 = CARTESIAN_POINT ( 'NONE',  ( -3.000416591977282496E-16, 15.19062500061459353, 25.09994784771203058 ) ) ;
#69411 = CARTESIAN_POINT ( 'NONE',  ( 1.071796769724490561, 13.30759618943233491, 34.00000000000000000 ) ) ;
#69412 = CARTESIAN_POINT ( 'NONE',  ( 6.000000000000001776, 4.330127018922192761, -2.499999999999997780 ) ) ;
#69413 = CARTESIAN_POINT ( 'NONE',  ( 15.00937500061451502, -5.492252693125287522, -1.008910452111647106E-15 ) ) ;
#69414 = CARTESIAN_POINT ( 'NONE',  ( 23.09062500061451573, -3.027376345333614438, 5.243569643749998122 ) ) ;
#69415 = CARTESIAN_POINT ( 'NONE',  ( 13.75312500061451715, -4.541064518000417216, -2.621784821875001281 ) ) ;
#69416 = CARTESIAN_POINT ( 'NONE',  ( 27.30937500061451217, 2.746126346562645981, -4.756430356249997438 ) ) ;
#69417 = CARTESIAN_POINT ( 'NONE',  ( 8.446875000614518569, -3.027376345333610441, -5.243569643749999898 ) ) ;
#69418 = CARTESIAN_POINT ( 'NONE',  ( 26.47499999999999787, -4.330127018922194537, 2.499999999999995559 ) ) ;
#69419 = CARTESIAN_POINT ( 'NONE',  ( 22.83750000122903501, 4.330127018922191873, 2.499999999999999556 ) ) ;
#69420 = DIRECTION ( 'NONE',  ( -0.000000000000000000, -1.000000000000000000, -0.000000000000000000 ) ) ;
#69421 = CARTESIAN_POINT ( 'NONE',  ( 12.49687500061451573, -3.027376345333610441, -5.243569643749999898 ) ) ;
#69422 = CARTESIAN_POINT ( 'NONE',  ( 27.15937500061451360, 0.000000000000000000, 5.243569643749999010 ) ) ;
#69423 = CARTESIAN_POINT ( 'NONE',  ( 0.000000000000000000, 20.00000000000000000, -33.99999999999999289 ) ) ;
#69424 = CARTESIAN_POINT ( 'NONE',  ( 18.98437500061451644, 4.541064518000418104, 2.621784821874999949 ) ) ;
#69425 = CARTESIAN_POINT ( 'NONE',  ( 12.60937500061451821, 4.541064518000418104, -2.621784821874998173 ) ) ;
#69426 = CARTESIAN_POINT ( 'NONE',  ( 3.756430356249998770, 19.46562499938548285, 32.16877607737302469 ) ) ;
#69427 = CARTESIAN_POINT ( 'NONE',  ( 24.60000000000000142, 0.000000000000000000, 4.999999999999998224 ) ) ;
#69428 = CARTESIAN_POINT ( 'NONE',  ( -1.878215178125001827, 20.59062499938548285, 33.25316411605952283 ) ) ;
#69429 = CARTESIAN_POINT ( 'NONE',  ( 4.243569643749999898, 11.08437500061451786, -30.00000000000000000 ) ) ;
#69430 = CARTESIAN_POINT ( 'NONE',  ( 28.39687500061452141, 5.492252693125287522, 3.363034840372157021E-16 ) ) ;
#69431 = CARTESIAN_POINT ( 'NONE',  ( 15.02812500061451750, -4.541064518000419881, 2.621784821874995952 ) ) ;
#69432 = CARTESIAN_POINT ( 'NONE',  ( 5.400000000000002132, -4.330127018922190985, -2.500000000000001332 ) ) ;
#69433 = EDGE_CURVE ( 'NONE', #47010, #65143, #31114, .T. ) ;
#69434 = CARTESIAN_POINT ( 'NONE',  ( 12.33750000122903145, 6.123233995736764310E-16, -4.999999999999998224 ) ) ;
#69435 = CARTESIAN_POINT ( 'NONE',  ( 65.00000000000000000, 0.000000000000000000, 0.000000000000000000 ) ) ;
#69436 = CARTESIAN_POINT ( 'NONE',  ( 13.79999999999999893, 0.000000000000000000, 4.999999999999998224 ) ) ;
#69437 = CARTESIAN_POINT ( 'NONE',  ( -4.243569643749999898, 9.865625000614517859, 27.54997392385601529 ) ) ;
#69438 = CARTESIAN_POINT ( 'NONE',  ( 13.91250000122903252, 0.000000000000000000, 4.999999999999998224 ) ) ;
#69439 = CARTESIAN_POINT ( 'NONE',  ( 24.04687500061451644, -3.027376345333614438, 5.243569643749998122 ) ) ;
#69440 = ORIENTED_EDGE ( 'NONE', *, *, #23832, .T. ) ;
#69441 = CARTESIAN_POINT ( 'NONE',  ( 18.77812500061451573, 6.421520780324663323E-16, -5.243569643749999010 ) ) ;
#69442 = CARTESIAN_POINT ( 'NONE',  ( 4.790625000614518569, -3.027376345333610441, -5.243569643749999898 ) ) ;
#69443 = CARTESIAN_POINT ( 'NONE',  ( 19.47187500061451360, 3.027376345333611329, 5.243569643749999010 ) ) ;
#69444 = CARTESIAN_POINT ( 'NONE',  ( 4.237500000000001599, 5.773502691896255534, 3.535250795749688894E-16 ) ) ;
#69445 = CARTESIAN_POINT ( 'NONE',  ( 6.815625000614517148, 3.027376345333611329, 5.243569643749999010 ) ) ;
#69446 = CARTESIAN_POINT ( 'NONE',  ( 22.82812500061451644, 6.421520780324663323E-16, -5.243569643749999010 ) ) ;
#69447 = CARTESIAN_POINT ( 'NONE',  ( -3.000416591977282496E-16, 14.29062500061451679, 25.09994784771203058 ) ) ;
#69448 = CARTESIAN_POINT ( 'NONE',  ( 20.13750000122903216, 4.330127018922191873, 2.499999999999999556 ) ) ;
#69449 = CARTESIAN_POINT ( 'NONE',  ( 11.18437500061451928, 5.824947211148865298E-16, -4.756430356249998326 ) ) ;
#69450 = CARTESIAN_POINT ( 'NONE',  ( 9.553125000614517859, 0.000000000000000000, 5.243569643749999010 ) ) ;
#69451 = CARTESIAN_POINT ( 'NONE',  ( 4.359375000614517326, -4.541064518000417216, -2.621784821875001281 ) ) ;
#69452 = CARTESIAN_POINT ( 'NONE',  ( 28.22812500061451502, 6.421520780324663323E-16, -5.243569643749999010 ) ) ;
#69453 = CARTESIAN_POINT ( 'NONE',  ( 24.38437500061451502, 4.541064518000418104, 2.621784821874999949 ) ) ;
#69454 = CARTESIAN_POINT ( 'NONE',  ( 13.64062500061451644, -3.027376345333614438, 5.243569643749998122 ) ) ;
#69455 = CARTESIAN_POINT ( 'NONE',  ( 25.05000000122903714, 5.773502691896255534, 3.535250795749688894E-16 ) ) ;
#69456 = CARTESIAN_POINT ( 'NONE',  ( 25.52812500061451573, 6.421520780324663323E-16, -5.243569643749999010 ) ) ;
#69457 = CARTESIAN_POINT ( 'NONE',  ( 18.45937500061451431, 4.541064518000418104, -2.621784821874998173 ) ) ;
#69458 = CARTESIAN_POINT ( 'NONE',  ( 14.42812500061451786, 4.541064518000418104, 2.621784821874999949 ) ) ;
#69459 = CARTESIAN_POINT ( 'NONE',  ( -2.121784821874996840, 16.33437500061451786, 33.67503911421598417 ) ) ;
#69460 = CARTESIAN_POINT ( 'NONE',  ( 22.71562500061451573, -6.054752690667223547, -1.112240025338166033E-15 ) ) ;
#69461 = CARTESIAN_POINT ( 'NONE',  ( 22.08749999999999503, -2.886751345948181946, -4.999999999999904077 ) ) ;
#69462 = ORIENTED_EDGE ( 'NONE', *, *, #21683, .F. ) ;
#69463 = CARTESIAN_POINT ( 'NONE',  ( 26.36249999999999716, 2.886751345948126879, 4.999999999999999112 ) ) ;
#69464 = CARTESIAN_POINT ( 'NONE',  ( -1.999999999999997113, 11.52500000000000036, -26.53589838486224295 ) ) ;
#69465 = CARTESIAN_POINT ( 'NONE',  ( -3.756430356250001434, 19.31562499938548427, 32.16877607737301048 ) ) ;
#69466 = CARTESIAN_POINT ( 'NONE',  ( 3.234375000614516438, 4.541064518000418104, 2.621784821874999949 ) ) ;
#69467 = CARTESIAN_POINT ( 'NONE',  ( 7.378125000614518036, -4.541064518000419881, 2.621784821874995952 ) ) ;
#69468 = CARTESIAN_POINT ( 'NONE',  ( 23.21250000122903501, 4.330127018922192761, -2.499999999999997780 ) ) ;
#69469 = EDGE_CURVE ( 'NONE', #27313, #30796, #45043, .T. ) ;
#69470 = CARTESIAN_POINT ( 'NONE',  ( 28.26562500061451289, 3.027376345333613106, -5.243569643749998122 ) ) ;
#69471 = CARTESIAN_POINT ( 'NONE',  ( 25.16249999999999432, -5.773502691896255534, -1.060575238724906372E-15 ) ) ;
#69472 = CARTESIAN_POINT ( 'NONE',  ( -3.999999999999999556, 16.47500000122903430, -32.30940107675850470 ) ) ;
#69473 = CARTESIAN_POINT ( 'NONE',  ( -5.810221930991193690E-16, 12.35000000122903430, 26.00000000000000355 ) ) ;
#69474 = CARTESIAN_POINT ( 'NONE',  ( 10.07812500061451644, -4.541064518000419881, 2.621784821874995952 ) ) ;
#69475 = VERTEX_POINT ( 'NONE', #68302 ) ;
#69476 = CARTESIAN_POINT ( 'NONE',  ( 26.80312500061451431, -4.541064518000417216, -2.621784821875001281 ) ) ;
#69477 = CARTESIAN_POINT ( 'NONE',  ( 6.778125000614518392, 4.541064518000418104, 2.621784821874999949 ) ) ;
#69478 = CARTESIAN_POINT ( 'NONE',  ( 3.065625000614517592, 3.027376345333613106, -5.243569643749998122 ) ) ;
#69479 = CARTESIAN_POINT ( 'NONE',  ( 15.87187500061451573, 2.746126346562643317, 4.756430356249998326 ) ) ;
#69480 = EDGE_CURVE ( 'NONE', #12248, #57768, #28319, .T. ) ;
#69481 = CARTESIAN_POINT ( 'NONE',  ( 12.93750000000000178, -2.886751345948130876, 4.999999999999996447 ) ) ;
#69482 = CARTESIAN_POINT ( 'NONE',  ( 12.59999999999999964, -4.330127018922190985, -2.500000000000001332 ) ) ;
#69483 = CARTESIAN_POINT ( 'NONE',  ( 12.72187500061451537, 3.027376345333611329, 5.243569643749999010 ) ) ;
#69484 = CARTESIAN_POINT ( 'NONE',  ( 8.625000001229034652, -5.773502691896255534, -1.060575238724906372E-15 ) ) ;
#69485 = CARTESIAN_POINT ( 'NONE',  ( 16.50937500061451502, -4.541064518000417216, -2.621784821875001281 ) ) ;
#69486 = CARTESIAN_POINT ( 'NONE',  ( 17.77499999999999858, 4.330127018922191873, 2.499999999999999556 ) ) ;
#69487 = CARTESIAN_POINT ( 'NONE',  ( 9.084375000614517859, 4.541064518000418104, 2.621784821874999949 ) ) ;
#69488 = CARTESIAN_POINT ( 'NONE',  ( -4.243569643749997233, 11.74062500061451786, -27.54997392385601174 ) ) ;
#69489 = CARTESIAN_POINT ( 'NONE',  ( -1.071796769724488563, 11.99240381056766758, -26.00000000000000000 ) ) ;
#69490 = CARTESIAN_POINT ( 'NONE',  ( 22.62187500061451573, -4.119189519843968306, 2.378215178124996054 ) ) ;
#69491 = VERTEX_POINT ( 'NONE', #11050 ) ;
#69492 = CARTESIAN_POINT ( 'NONE',  ( 24.32812500061451289, 4.541064518000418104, 2.621784821874999949 ) ) ;
#69493 = CARTESIAN_POINT ( 'NONE',  ( 11.13750000000000107, -2.886751345948130876, 4.999999999999996447 ) ) ;
#69494 = CARTESIAN_POINT ( 'NONE',  ( 27.30937500061451573, -4.541064518000417216, -2.621784821875001281 ) ) ;
#69495 = CARTESIAN_POINT ( 'NONE',  ( 22.08749999999999858, -2.886751345948125991, -5.000000000000000000 ) ) ;
#69496 = CARTESIAN_POINT ( 'NONE',  ( 6.403125000614517504, 0.000000000000000000, 5.243569643749999010 ) ) ;
#69497 = CARTESIAN_POINT ( 'NONE',  ( 24.45937500061451786, -5.492252693125287522, -1.008910452111647106E-15 ) ) ;
#69498 = CARTESIAN_POINT ( 'NONE',  ( 15.75937500061451857, 4.541064518000418104, -2.621784821874998173 ) ) ;
#69499 = CARTESIAN_POINT ( 'NONE',  ( 8.859375000614514661, 2.746126346562645981, -4.756430356249997438 ) ) ;
#69500 = CARTESIAN_POINT ( 'NONE',  ( 28.95000000122903572, -2.886751345948125991, -5.000000000000000000 ) ) ;
#69501 = CARTESIAN_POINT ( 'NONE',  ( 9.046875000614518214, 6.054752690667223547, 3.707466751127219781E-16 ) ) ;
#69502 = VERTEX_POINT ( 'NONE', #66853 ) ;
#69503 = CARTESIAN_POINT ( 'NONE',  ( 20.10937500061451289, -4.541064518000417216, -2.621784821875001281 ) ) ;
#69504 = CARTESIAN_POINT ( 'NONE',  ( 15.43125000122903323, 6.123233995736764310E-16, -4.999999999999998224 ) ) ;
#69505 = CARTESIAN_POINT ( 'NONE',  ( 27.03750000000000142, -2.886751345948125991, -5.000000000000000000 ) ) ;
#69506 = CARTESIAN_POINT ( 'NONE',  ( 29.14687500061451075, -3.027376345333610441, -5.243569643749999898 ) ) ;
#69507 = CARTESIAN_POINT ( 'NONE',  ( 1.999999999999998668, 10.40000000000000213, -33.46410161513775705 ) ) ;
#69508 = VERTEX_POINT ( 'NONE', #45766 ) ;
#69509 = CARTESIAN_POINT ( 'NONE',  ( 11.25000000000000000, -4.330127018922190985, -2.500000000000001332 ) ) ;
#69510 = CARTESIAN_POINT ( 'NONE',  ( 12.45937500061451608, 2.746126346562645981, -4.756430356249997438 ) ) ;
#69511 = CARTESIAN_POINT ( 'NONE',  ( 21.21562500061451573, 3.027376345333611329, 5.243569643749999010 ) ) ;
#69512 = CARTESIAN_POINT ( 'NONE',  ( 14.21249999999999858, 2.886751345948126879, 4.999999999999999112 ) ) ;
#69513 = EDGE_CURVE ( 'NONE', #69611, #860, #55718, .T. ) ;
#69514 = CARTESIAN_POINT ( 'NONE',  ( 8.700000001229032165, -2.886751345948125991, -5.000000000000000000 ) ) ;
#69515 = CARTESIAN_POINT ( 'NONE',  ( 5.953125000614519102, 0.000000000000000000, 5.243569643749999010 ) ) ;
#69516 = CARTESIAN_POINT ( 'NONE',  ( 20.73750000000000071, -2.886751345948125991, -5.000000000000000000 ) ) ;
#69517 = CARTESIAN_POINT ( 'NONE',  ( 21.66562500061451502, 3.027376345333611329, 5.243569643749999010 ) ) ;
#69518 = CARTESIAN_POINT ( 'NONE',  ( 23.69999999999999929, 0.000000000000000000, 4.999999999999998224 ) ) ;
#69519 = CARTESIAN_POINT ( 'NONE',  ( 24.56250000122903288, 4.330127018922192761, -2.499999999999997780 ) ) ;
#69520 = CARTESIAN_POINT ( 'NONE',  ( -3.756430356250000102, 16.91562499938548214, 30.00000000000000000 ) ) ;
#69521 = CARTESIAN_POINT ( 'NONE',  ( 5.887500000000000178, -2.886751345948125991, -5.000000000000000000 ) ) ;
#69522 = ORIENTED_EDGE ( 'NONE', *, *, #69109, .T. ) ;
#69523 = CARTESIAN_POINT ( 'NONE',  ( 20.84062500061451573, -3.027376345333614438, 5.243569643749998122 ) ) ;
#69524 = CARTESIAN_POINT ( 'NONE',  ( 26.35312500061451857, -4.541064518000417216, -2.621784821875001281 ) ) ;
#69525 = CARTESIAN_POINT ( 'NONE',  ( 27.15937500061451360, 0.000000000000000000, 5.243569643749999010 ) ) ;
#69526 = CARTESIAN_POINT ( 'NONE',  ( 15.14062500061451644, -3.027376345333610441, -5.243569643749999898 ) ) ;
#69527 = CARTESIAN_POINT ( 'NONE',  ( -4.243569643749998122, 9.940625000614591755, -27.54997392385601174 ) ) ;
#69528 = CARTESIAN_POINT ( 'NONE',  ( 26.51250000122903216, 0.000000000000000000, 4.999999999999998224 ) ) ;
#69529 = CARTESIAN_POINT ( 'NONE',  ( 19.05937500061451928, 0.000000000000000000, 4.756430356249998326 ) ) ;
#69530 = CARTESIAN_POINT ( 'NONE',  ( 15.96562500061451573, -6.054752690667223547, -1.112240025338166033E-15 ) ) ;
#69531 = CARTESIAN_POINT ( 'NONE',  ( 2.000000000000001332, 14.41250000122903430, -26.53589838486224650 ) ) ;
#69532 = CARTESIAN_POINT ( 'NONE',  ( 3.937500001229034208, 4.330127018922191873, 2.499999999999999556 ) ) ;
#69533 = CARTESIAN_POINT ( 'NONE',  ( 9.946875000614516793, 6.054752690667223547, 3.707466751127219781E-16 ) ) ;
#69534 = CARTESIAN_POINT ( 'NONE',  ( 9.121875000614517504, 3.027376345333611329, 5.243569643749999010 ) ) ;
#69535 = CARTESIAN_POINT ( 'NONE',  ( 18.00937500061451502, 4.541064518000418104, -2.621784821874998173 ) ) ;
#69536 = ORIENTED_EDGE ( 'NONE', *, *, #41902, .F. ) ;
#69537 = CARTESIAN_POINT ( 'NONE',  ( -5.193763058582910652, 8.549021686977596346, 26.97145083886558581 ) ) ;
#69538 = CARTESIAN_POINT ( 'NONE',  ( 24.55312500061451786, -4.541064518000417216, -2.621784821875001281 ) ) ;
#69539 = CARTESIAN_POINT ( 'NONE',  ( 20.03437500061451715, -4.541064518000419881, 2.621784821874995952 ) ) ;
#69540 = CARTESIAN_POINT ( 'NONE',  ( 23.01562500061451644, 3.027376345333611329, 5.243569643749999010 ) ) ;
#69541 = CARTESIAN_POINT ( 'NONE',  ( 1.626862140677534273E-15, 9.875000001229034652, 34.00000000000000000 ) ) ;
#69542 = CARTESIAN_POINT ( 'NONE',  ( 1.999999999999998668, 13.55000000000000071, 26.53589838486224650 ) ) ;
#69543 = CARTESIAN_POINT ( 'NONE',  ( 29.39062500061451289, -3.027376345333614438, 5.243569643749998122 ) ) ;
#69544 = CARTESIAN_POINT ( 'NONE',  ( 9.562500001229032875, -4.330127018922190985, -2.500000000000001332 ) ) ;
#69545 = EDGE_LOOP ( 'NONE', ( #56123, #24837, #36559, #52680 ) ) ;
#69546 = CARTESIAN_POINT ( 'NONE',  ( 5.137500001229033941, 6.123233995736764310E-16, -4.999999999999998224 ) ) ;
#69547 = CARTESIAN_POINT ( 'NONE',  ( 1.999999999999998668, 19.40000000000000213, -33.46410161513775705 ) ) ;
#69548 = CARTESIAN_POINT ( 'NONE',  ( 27.41250000122903430, 0.000000000000000000, 4.999999999999998224 ) ) ;
#69549 = CARTESIAN_POINT ( 'NONE',  ( -3.999999999999999556, 19.83124999877096073, 27.69059892324149175 ) ) ;
#69550 = CARTESIAN_POINT ( 'NONE',  ( 9.384375000614518569, 6.421520780324663323E-16, -5.243569643749999010 ) ) ;
#69551 = CARTESIAN_POINT ( 'NONE',  ( 17.77499999999999858, 4.330127018922191873, 2.499999999999999556 ) ) ;
#69552 = CARTESIAN_POINT ( 'NONE',  ( 14.01562500061451644, 3.027376345333611329, 5.243569643749999010 ) ) ;
#69553 = CARTESIAN_POINT ( 'NONE',  ( 12.15937500061451892, 4.541064518000418104, -2.621784821874998173 ) ) ;
#69554 = CARTESIAN_POINT ( 'NONE',  ( 3.590625000614518836, 6.054752690667223547, 3.707466751127219781E-16 ) ) ;
#69555 = CARTESIAN_POINT ( 'NONE',  ( 20.82187500061451857, 3.027376345333611329, 5.243569643749999010 ) ) ;
#69556 = CARTESIAN_POINT ( 'NONE',  ( 6.759375000614516793, 4.541064518000418104, -2.621784821874998173 ) ) ;
#69557 = CARTESIAN_POINT ( 'NONE',  ( 10.00000000000000000, 1.224646799147353256E-15, 10.00000000000000178 ) ) ;
#69558 = CARTESIAN_POINT ( 'NONE',  ( 8.728125000614518569, -4.541064518000419881, 2.621784821874995952 ) ) ;
#69559 = CARTESIAN_POINT ( 'NONE',  ( 17.76562500061451644, -6.054752690667223547, -1.112240025338166033E-15 ) ) ;
#69560 = VERTEX_POINT ( 'NONE', #27687 ) ;
#69561 = CARTESIAN_POINT ( 'NONE',  ( 15.47812500061451679, -4.541064518000419881, 2.621784821874995952 ) ) ;
#69562 = CARTESIAN_POINT ( 'NONE',  ( 10.37812500061451715, 4.541064518000418104, 2.621784821874999949 ) ) ;
#69563 = CARTESIAN_POINT ( 'NONE',  ( 23.70937500061451786, -4.119189519843965641, -2.378215178125001383 ) ) ;
#69564 = CARTESIAN_POINT ( 'NONE',  ( 11.51250000000000107, 2.886751345948126879, 4.999999999999999112 ) ) ;
#69565 = ADVANCED_FACE ( 'NONE', ( #55758 ), #43417, .T. ) ;
#69566 = CARTESIAN_POINT ( 'NONE',  ( 7.762500001229033053, -4.330127018922190985, -2.500000000000001332 ) ) ;
#69567 = CARTESIAN_POINT ( 'NONE',  ( 14.18437500061451750, -4.541064518000419881, 2.621784821874995952 ) ) ;
#69568 = CARTESIAN_POINT ( 'NONE',  ( 16.72500000122903430, -5.773502691896255534, -1.060575238724906372E-15 ) ) ;
#69569 = CARTESIAN_POINT ( 'NONE',  ( 23.88749999999999929, -2.886751345948125991, -5.000000000000000000 ) ) ;
#69570 = CARTESIAN_POINT ( 'NONE',  ( -2.121784821874999949, 19.27812500061451573, -33.67503911421598417 ) ) ;
#69571 = DIRECTION ( 'NONE',  ( -0.000000000000000000, -1.000000000000000000, -0.000000000000000000 ) ) ;
#69572 = CARTESIAN_POINT ( 'NONE',  ( 23.47500000122903430, -5.773502691896255534, -1.060575238724906372E-15 ) ) ;
#69573 = CARTESIAN_POINT ( 'NONE',  ( 3.408588963864223054, -3.658193339867878535, 3.653826635041531379 ) ) ;
#69574 = CARTESIAN_POINT ( 'NONE',  ( 4.489140539347876491, 3.724300126011093504, -4.036462246613610638 ) ) ;
#69575 = CARTESIAN_POINT ( 'NONE',  ( 17.93437500061451928, 6.421520780324663323E-16, -5.243569643749999010 ) ) ;
#69576 =( BOUNDED_CURVE ( )  B_SPLINE_CURVE ( 2, ( #52492, #25508, #36228, #64665, #35853, #24769, #30325 ),
 .UNSPECIFIED., .F., .F. ) 
 B_SPLINE_CURVE_WITH_KNOTS ( ( 3, 2, 2, 3 ),
 ( 0.3083333333333333481, 0.3111111111111111160, 0.3138888888888888840, 0.3166666666666666519 ),
 .UNSPECIFIED. ) 
 CURVE ( )  GEOMETRIC_REPRESENTATION_ITEM ( )  RATIONAL_B_SPLINE_CURVE ( ( 1.000000000000000000, 0.8660254037844387076, 1.000000000000000000, 0.8660254037844387076, 1.000000000000000000, 0.8660254037844387076, 1.000000000000000000 ) ) 
 REPRESENTATION_ITEM ( '' )  );
#69577 = CARTESIAN_POINT ( 'NONE',  ( 14.35312500061451679, 4.541064518000418104, -2.621784821874998173 ) ) ;
#69578 = CARTESIAN_POINT ( 'NONE',  ( 8.268750001229031810, 2.886751345948129099, -4.999999999999998224 ) ) ;
#69579 = CARTESIAN_POINT ( 'NONE',  ( 4.000000000000000000, 16.58750000000000213, 27.69059892324149885 ) ) ;
#69580 = CARTESIAN_POINT ( 'NONE',  ( 24.34687500061451715, 6.054752690667223547, 3.707466751127219781E-16 ) ) ;
#69581 = CARTESIAN_POINT ( 'NONE',  ( 15.08437500061451431, -2.746126346562641984, -4.756430356249999214 ) ) ;
#69582 = CARTESIAN_POINT ( 'NONE',  ( 10.00312500061451715, 0.000000000000000000, 5.243569643749999010 ) ) ;
#69583 = CARTESIAN_POINT ( 'NONE',  ( 16.17187500061451644, 3.027376345333613106, -5.243569643749998122 ) ) ;
#69584 = EDGE_LOOP ( 'NONE', ( #55101, #51272, #24240, #52884 ) ) ;
#69585 = CARTESIAN_POINT ( 'NONE',  ( 27.00937500061451857, 4.541064518000418104, -2.621784821874998173 ) ) ;
#69586 = CARTESIAN_POINT ( 'NONE',  ( 27.89062500061451289, 6.054752690667223547, 3.707466751127219781E-16 ) ) ;
#69587 = CARTESIAN_POINT ( 'NONE',  ( 17.99062500061451786, 6.054752690667223547, 3.707466751127219781E-16 ) ) ;
#69588 = CARTESIAN_POINT ( 'NONE',  ( 22.12500000000000000, 6.123233995736764310E-16, -4.999999999999998224 ) ) ;
#69589 = CYLINDRICAL_SURFACE ( 'NONE', #46682, 4.999999999999998224 ) ;
#69590 = CARTESIAN_POINT ( 'NONE',  ( 8.812500000000000000, 2.886751345948126879, 4.999999999999999112 ) ) ;
#69591 = CARTESIAN_POINT ( 'NONE',  ( 19.61250000122903359, 4.330127018922192761, -2.499999999999997780 ) ) ;
#69592 = CYLINDRICAL_SURFACE ( 'NONE', #23055, 4.999999999999998224 ) ;
#69593 = CARTESIAN_POINT ( 'NONE',  ( 9.346875000614517148, 4.119189519843966529, -2.378215178124998275 ) ) ;
#69594 = EDGE_LOOP ( 'NONE', ( #19553, #28354, #62228, #11356 ) ) ;
#69595 = CARTESIAN_POINT ( 'NONE',  ( 17.10000000000000142, -4.330127018922190985, -2.500000000000001332 ) ) ;
#69596 = CARTESIAN_POINT ( 'NONE',  ( 21.67500000000000071, 6.123233995736764310E-16, -4.999999999999998224 ) ) ;
#69597 = CARTESIAN_POINT ( 'NONE',  ( 18.27187500061451431, -6.054752690667223547, -1.112240025338166033E-15 ) ) ;
#69598 = CARTESIAN_POINT ( 'NONE',  ( 14.54062500061451679, -3.027376345333614438, 5.243569643749998122 ) ) ;
#69599 = EDGE_CURVE ( 'NONE', #57032, #40816, #32130, .T. ) ;
#69600 = ORIENTED_EDGE ( 'NONE', *, *, #5067, .F. ) ;
#69601 = CARTESIAN_POINT ( 'NONE',  ( 45.00000000000000000, 6.123233995736764310E-16, -4.999999999999998224 ) ) ;
#69602 = CARTESIAN_POINT ( 'NONE',  ( 6.028125000614517504, -4.541064518000419881, 2.621784821874995952 ) ) ;
#69603 = DIRECTION ( 'NONE',  ( 0.000000000000000000, 0.000000000000000000, 1.000000000000000000 ) ) ;
#69604 = CARTESIAN_POINT ( 'NONE',  ( 13.08750000000000036, -2.886751345948125991, -5.000000000000000000 ) ) ;
#69605 = CARTESIAN_POINT ( 'NONE',  ( 28.99687500061451217, -4.119189519843965641, -2.378215178125001383 ) ) ;
#69606 = CARTESIAN_POINT ( 'NONE',  ( 4.243569643749999010, 15.56562500061451715, 27.54997392385601174 ) ) ;
#69607 = CARTESIAN_POINT ( 'NONE',  ( 28.86562500061451786, 3.027376345333611329, 5.243569643749999010 ) ) ;
#69608 = CARTESIAN_POINT ( 'NONE',  ( 8.550000000000002487, -4.330127018922190985, -2.500000000000001332 ) ) ;
#69609 = CARTESIAN_POINT ( 'NONE',  ( -1.878215178125001827, 17.44062499938548072, 33.25316411605952283 ) ) ;
#69610 = CARTESIAN_POINT ( 'NONE',  ( 24.15937500061451715, -4.541064518000417216, -2.621784821875001281 ) ) ;
#69611 = VERTEX_POINT ( 'NONE', #20500 ) ;
#69612 = CARTESIAN_POINT ( 'NONE',  ( 21.66562500061451502, 3.027376345333611329, 5.243569643749999010 ) ) ;
#69613 = CARTESIAN_POINT ( 'NONE',  ( 23.25937500061451857, -4.541064518000417216, -2.621784821875001281 ) ) ;
#69614 = CARTESIAN_POINT ( 'NONE',  ( 4.243569643749999898, 15.94062500061459176, -27.54997392385601529 ) ) ;
#69615 = CARTESIAN_POINT ( 'NONE',  ( 7.265625000614516438, 3.027376345333611329, 5.243569643749999010 ) ) ;
#69616 = CARTESIAN_POINT ( 'NONE',  ( 23.95312500061451289, 0.000000000000000000, 5.243569643749999010 ) ) ;
#69617 = CARTESIAN_POINT ( 'NONE',  ( 26.93437500061451573, 5.492252693125287522, 3.363034840372157021E-16 ) ) ;
#69618 = CARTESIAN_POINT ( 'NONE',  ( 11.25937500061451679, 4.119189519843966529, -2.378215178124998275 ) ) ;
#69619 = CARTESIAN_POINT ( 'NONE',  ( 17.33437500061451431, -4.541064518000419881, 2.621784821874995952 ) ) ;
#69620 = CARTESIAN_POINT ( 'NONE',  ( 27.34687500061451360, -3.027376345333610441, -5.243569643749999898 ) ) ;
#69621 = CARTESIAN_POINT ( 'NONE',  ( -4.243569643749998122, 17.64687500061451786, 32.45002607614398471 ) ) ;
#69622 = CARTESIAN_POINT ( 'NONE',  ( 6.403125000614517504, 0.000000000000000000, 5.243569643749999010 ) ) ;
#69623 = CARTESIAN_POINT ( 'NONE',  ( 2.000000000000001332, 16.10000000000000142, 33.46410161513774995 ) ) ;
#69624 = CARTESIAN_POINT ( 'NONE',  ( 4.209375000614516971, 0.000000000000000000, 5.243569643749999010 ) ) ;
#69625 = CARTESIAN_POINT ( 'NONE',  ( 26.62500000000000000, 6.123233995736764310E-16, -4.999999999999998224 ) ) ;
#69626 = CARTESIAN_POINT ( 'NONE',  ( 6.365625000614518747, 3.027376345333611329, 5.243569643749999010 ) ) ;
#69627 = CARTESIAN_POINT ( 'NONE',  ( 9.496875000614517504, 6.054752690667223547, 3.707466751127219781E-16 ) ) ;
#69628 = CARTESIAN_POINT ( 'NONE',  ( 17.06250000122903288, 0.000000000000000000, 4.999999999999998224 ) ) ;
#69629 = CARTESIAN_POINT ( 'NONE',  ( 29.80312500061451431, 0.000000000000000000, 5.243569643749999010 ) ) ;
#69630 = CARTESIAN_POINT ( 'NONE',  ( 7.303125000614516082, 0.000000000000000000, 5.243569643749999010 ) ) ;
#69631 = CARTESIAN_POINT ( 'NONE',  ( 2.000000000000000444, 13.41874999877096641, 26.53589838486224650 ) ) ;
#69632 = CARTESIAN_POINT ( 'NONE',  ( 22.18125000122903145, 6.123233995736764310E-16, -4.999999999999998224 ) ) ;
#69633 = CARTESIAN_POINT ( 'NONE',  ( 15.64687500061451608, -3.027376345333610441, -5.243569643749999898 ) ) ;
#69634 = LINE ( 'NONE', #18996, #31323 ) ;
#69635 = VERTEX_POINT ( 'NONE', #65582 ) ;
#69636 = CARTESIAN_POINT ( 'NONE',  ( 25.19062500061451715, 6.054752690667223547, 3.707466751127219781E-16 ) ) ;
#69637 = CARTESIAN_POINT ( 'NONE',  ( 10.49062500061451431, -3.027376345333614438, 5.243569643749998122 ) ) ;
#69638 = CARTESIAN_POINT ( 'NONE',  ( 26.63437500061451857, 4.541064518000418104, 2.621784821874999949 ) ) ;
#69639 = CARTESIAN_POINT ( 'NONE',  ( 9.365625000614519635, 3.027376345333613106, -5.243569643749998122 ) ) ;
#69640 = CARTESIAN_POINT ( 'NONE',  ( 3.412500001229032964, 4.330127018922192761, -2.499999999999997780 ) ) ;
#69641 = CARTESIAN_POINT ( 'NONE',  ( 10.95000000122903394, -2.886751345948125991, -5.000000000000000000 ) ) ;
#69642 = CARTESIAN_POINT ( 'NONE',  ( 24.02812500061451573, -4.541064518000419881, 2.621784821874995952 ) ) ;
#69643 = CARTESIAN_POINT ( 'NONE',  ( -4.243569643749999898, 13.91562500061451679, -32.45002607614398471 ) ) ;
#69644 = CARTESIAN_POINT ( 'NONE',  ( 12.86250000122903359, 4.330127018922192761, -2.499999999999997780 ) ) ;
#69645 = CARTESIAN_POINT ( 'NONE',  ( 21.89062500061451289, -3.027376345333610441, -5.243569643749999898 ) ) ;
#69646 = CARTESIAN_POINT ( 'NONE',  ( 18.77812500061451573, 6.421520780324663323E-16, -5.243569643749999010 ) ) ;
#69647 = CARTESIAN_POINT ( 'NONE',  ( 6.496875000614518392, -3.027376345333614438, 5.243569643749998122 ) ) ;
#69648 = CARTESIAN_POINT ( 'NONE',  ( 18.56250000000000000, 2.886751345948129099, -4.999999999999998224 ) ) ;
#69649 = CARTESIAN_POINT ( 'NONE',  ( 13.38750000122903394, 4.330127018922191873, 2.499999999999999556 ) ) ;
#69650 = CARTESIAN_POINT ( 'NONE',  ( 9.740625000614516082, -3.027376345333610441, -5.243569643749999898 ) ) ;
#69651 = CARTESIAN_POINT ( 'NONE',  ( 14.16562500061451679, -6.054752690667223547, -1.112240025338166033E-15 ) ) ;
#69652 = CARTESIAN_POINT ( 'NONE',  ( 25.68750000122903288, -4.330127018922194537, 2.499999999999995559 ) ) ;
#69653 = CARTESIAN_POINT ( 'NONE',  ( 21.75937500061451502, 0.000000000000000000, 5.243569643749999010 ) ) ;
#69654 = CARTESIAN_POINT ( 'NONE',  ( 20.18437500061451573, 6.421520780324663323E-16, -5.243569643749999010 ) ) ;
#69655 = CARTESIAN_POINT ( 'NONE',  ( 13.79999999999999893, 0.000000000000000000, 4.999999999999998224 ) ) ;
#69656 = CARTESIAN_POINT ( 'NONE',  ( 6.825000001229034829, -5.773502691896255534, -1.060575238724906372E-15 ) ) ;
#69657 = CARTESIAN_POINT ( 'NONE',  ( 5.709375000614517859, -4.541064518000417216, -2.621784821875001281 ) ) ;
#69658 = CARTESIAN_POINT ( 'NONE',  ( 26.25937500061451857, 0.000000000000000000, 5.243569643749999010 ) ) ;
#69659 = DIRECTION ( 'NONE',  ( 0.000000000000000000, 0.000000000000000000, 1.000000000000000000 ) ) ;
#69660 = EDGE_CURVE ( 'NONE', #18895, #71251, #68443, .T. ) ;
#69661 = CARTESIAN_POINT ( 'NONE',  ( 21.55312500061451431, 4.541064518000418104, -2.621784821874998173 ) ) ;
#69662 = CARTESIAN_POINT ( 'NONE',  ( 27.75937500061451502, -4.541064518000417216, -2.621784821875001281 ) ) ;
#69663 = CARTESIAN_POINT ( 'NONE',  ( -3.756430356250000102, 17.92812499938548498, 30.00000000000000000 ) ) ;
#69664 = CARTESIAN_POINT ( 'NONE',  ( 18.07499999999999929, 6.123233995736764310E-16, -4.999999999999998224 ) ) ;
#69665 = CARTESIAN_POINT ( 'NONE',  ( 2.000000000000001332, 13.96250000122903323, -26.53589838486224650 ) ) ;
#69666 = CARTESIAN_POINT ( 'NONE',  ( 7.959375000614516971, -4.541064518000417216, -2.621784821875001281 ) ) ;
#69667 = CARTESIAN_POINT ( 'NONE',  ( 17.50312500061451715, 4.541064518000418104, -2.621784821874998173 ) ) ;
#69668 = EDGE_LOOP ( 'NONE', ( #54964, #9960, #71090, #14751 ) ) ;
#69669 = DIRECTION ( 'NONE',  ( -1.000000000000000000, -0.000000000000000000, -0.000000000000000000 ) ) ;
#69670 = CARTESIAN_POINT ( 'NONE',  ( 26.61562500061451786, 3.027376345333611329, 5.243569643749999010 ) ) ;
#69671 = CARTESIAN_POINT ( 'NONE',  ( 4.096875000614518925, 6.054752690667223547, 3.707466751127219781E-16 ) ) ;
#69672 = CARTESIAN_POINT ( 'NONE',  ( -1.999999999999997113, 16.02500000000000213, -26.53589838486224295 ) ) ;
#69673 = CARTESIAN_POINT ( 'NONE',  ( 11.28749999999999432, -2.886751345948181946, -4.999999999999904077 ) ) ;
#69674 = CARTESIAN_POINT ( 'NONE',  ( 17.55000000000000071, -4.330127018922190985, -2.500000000000001332 ) ) ;
#69675 = CARTESIAN_POINT ( 'NONE',  ( 20.95312500061451999, -4.541064518000417216, -2.621784821875001281 ) ) ;
#69676 = ORIENTED_EDGE ( 'NONE', *, *, #58649, .F. ) ;
#69677 = CARTESIAN_POINT ( 'NONE',  ( 25.05000000000000071, 0.000000000000000000, 4.999999999999998224 ) ) ;
#69678 = CARTESIAN_POINT ( 'NONE',  ( 25.39687500061451431, -3.027376345333614438, 5.243569643749998122 ) ) ;
#69679 = EDGE_CURVE ( 'NONE', #7528, #69491, #20305, .T. ) ;
#69680 = ORIENTED_EDGE ( 'NONE', *, *, #63249, .F. ) ;
#69681 = CARTESIAN_POINT ( 'NONE',  ( 3.021917804904423743, -3.983467431823952687, -3.409840147052992432 ) ) ;
#69682 = CARTESIAN_POINT ( 'NONE',  ( 12.85312500061451502, -4.541064518000417216, -2.621784821875001281 ) ) ;
#69683 = CARTESIAN_POINT ( 'NONE',  ( 6.928125000614516082, -4.541064518000419881, 2.621784821874995952 ) ) ;
#69684 = CARTESIAN_POINT ( 'NONE',  ( 17.63437500061451502, -2.746126346562646425, 4.756430356249996549 ) ) ;
#69685 = CARTESIAN_POINT ( 'NONE',  ( 3.159375000614518036, 4.541064518000418104, -2.621784821874998173 ) ) ;
#69686 = CARTESIAN_POINT ( 'NONE',  ( 16.46250000122903501, 4.330127018922192761, -2.499999999999997780 ) ) ;
#69687 = CARTESIAN_POINT ( 'NONE',  ( 20.62499999999999645, -4.330127018922194537, 2.499999999999995559 ) ) ;
#69688 = CARTESIAN_POINT ( 'NONE',  ( 29.51249999999999929, 2.886751345948126879, 4.999999999999999112 ) ) ;
#69689 = CARTESIAN_POINT ( 'NONE',  ( 2.971875000614517592, -6.054752690667223547, -1.112240025338166033E-15 ) ) ;
#69690 = CARTESIAN_POINT ( 'NONE',  ( 9.159375000614515372, 0.000000000000000000, 5.243569643749999010 ) ) ;
#69691 = CARTESIAN_POINT ( 'NONE',  ( 19.02187500061451786, 3.027376345333611329, 5.243569643749999010 ) ) ;
#69692 = CARTESIAN_POINT ( 'NONE',  ( 11.45625000122903181, 4.330127018922192761, -2.499999999999997780 ) ) ;
#69693 = VERTEX_POINT ( 'NONE', #9442 ) ;
#69694 = CARTESIAN_POINT ( 'NONE',  ( 27.77812500061451573, 6.421520780324663323E-16, -5.243569643749999010 ) ) ;
#69695 = CARTESIAN_POINT ( 'NONE',  ( 29.10937500061451644, -4.541064518000417216, -2.621784821875001281 ) ) ;
#69696 = CARTESIAN_POINT ( 'NONE',  ( 4.096875000614518925, 6.054752690667223547, 3.707466751127219781E-16 ) ) ;
#69697 = CARTESIAN_POINT ( 'NONE',  ( 16.72500000000000142, 6.123233995736764310E-16, -4.999999999999998224 ) ) ;
#69698 = CARTESIAN_POINT ( 'NONE',  ( 14.16562500061451679, -6.054752690667223547, -1.112240025338166033E-15 ) ) ;
#69699 = CARTESIAN_POINT ( 'NONE',  ( -2.000000000000001776, 19.09999999999999787, 33.46410161513775705 ) ) ;
#69700 = CARTESIAN_POINT ( 'NONE',  ( 45.00000000000000000, 0.000000000000000000, 4.999999999999998224 ) ) ;
#69701 = CARTESIAN_POINT ( 'NONE',  ( 19.46250000122903145, -4.330127018922190985, -2.500000000000001332 ) ) ;
#69702 = CARTESIAN_POINT ( 'NONE',  ( -3.999999999999997335, 13.40000000122903323, 32.30940107675850470 ) ) ;
#69703 = CARTESIAN_POINT ( 'NONE',  ( 17.07187500061451502, 2.746126346562645981, -4.756430356249997438 ) ) ;
#69704 = CARTESIAN_POINT ( 'NONE',  ( 6.665625000614515905, 3.027376345333613106, -5.243569643749998122 ) ) ;
#69705 = CARTESIAN_POINT ( 'NONE',  ( 25.35937500061451644, 0.000000000000000000, 5.243569643749999010 ) ) ;
#69706 = CARTESIAN_POINT ( 'NONE',  ( -3.000416591977282496E-16, 19.74687500061451928, 25.09994784771203058 ) ) ;
#69707 = CARTESIAN_POINT ( 'NONE',  ( 26.82187500061451857, -6.054752690667223547, -1.112240025338166033E-15 ) ) ;
#69708 = CARTESIAN_POINT ( 'NONE',  ( 7.275000000000000355, 6.123233995736764310E-16, -4.999999999999998224 ) ) ;
#69709 = CARTESIAN_POINT ( 'NONE',  ( -3.999999999999999112, 13.81250000122903465, 30.00000000000000000 ) ) ;
#69710 = CARTESIAN_POINT ( 'NONE',  ( 15.85312500061451857, 0.000000000000000000, 5.243569643749999010 ) ) ;
#69711 = CARTESIAN_POINT ( 'NONE',  ( 6.825000001229034829, -5.773502691896255534, -1.060575238724906372E-15 ) ) ;
#69712 = CARTESIAN_POINT ( 'NONE',  ( 11.18437500061451928, 6.421520780324663323E-16, -5.243569643749999010 ) ) ;
#69713 = LINE ( 'NONE', #42370, #19446 ) ;
#69714 = VERTEX_POINT ( 'NONE', #37138 ) ;
#69715 = CARTESIAN_POINT ( 'NONE',  ( 11.20312500061451644, 4.541064518000418104, -2.621784821874998173 ) ) ;
#69716 = DIRECTION ( 'NONE',  ( 0.000000000000000000, 1.000000000000000000, -6.195440985631455317E-17 ) ) ;
#69717 = CARTESIAN_POINT ( 'NONE',  ( 23.25000000122903288, 5.773502691896255534, 3.535250795749688894E-16 ) ) ;
#69718 = CARTESIAN_POINT ( 'NONE',  ( 11.78437500061451892, 4.541064518000418104, 2.621784821874999949 ) ) ;
#69719 = CARTESIAN_POINT ( 'NONE',  ( 15.62812500061451537, 6.421520780324663323E-16, -5.243569643749999010 ) ) ;
#69720 = CARTESIAN_POINT ( 'NONE',  ( 23.74687500061451573, -3.027376345333610441, -5.243569643749999898 ) ) ;
#69721 = CARTESIAN_POINT ( 'NONE',  ( 45.00000000000000000, 0.000000000000000000, 0.000000000000000000 ) ) ;
#69722 = LINE ( 'NONE', #18728, #48090 ) ;
#69723 = CARTESIAN_POINT ( 'NONE',  ( -4.243569643749999898, 14.42187500061451999, -32.45002607614398471 ) ) ;
#69724 = VECTOR ( 'NONE', #23245, 1000.000000000000000 ) ;
#69725 = CARTESIAN_POINT ( 'NONE',  ( 15.34687500061451537, 6.054752690667223547, 3.707466751127219781E-16 ) ) ;
#69726 = CARTESIAN_POINT ( 'NONE',  ( 18.56250000122903288, -4.330127018922190985, -2.500000000000001332 ) ) ;
#69727 = CARTESIAN_POINT ( 'NONE',  ( 11.82187500061451679, 3.027376345333611329, 5.243569643749999010 ) ) ;
#69728 = CARTESIAN_POINT ( 'NONE',  ( 2.121784821875001281, 19.05312500061451431, -26.32496088578401938 ) ) ;
#69729 = CARTESIAN_POINT ( 'NONE',  ( 19.16250000122903430, 4.330127018922192761, -2.499999999999997780 ) ) ;
#69730 = CARTESIAN_POINT ( 'NONE',  ( 13.37812500061451715, 6.421520780324663323E-16, -5.243569643749999010 ) ) ;
#69731 = VERTEX_POINT ( 'NONE', #32334 ) ;
#69732 = ORIENTED_EDGE ( 'NONE', *, *, #4648, .F. ) ;
#69733 = CARTESIAN_POINT ( 'NONE',  ( 18.41250000000000142, -5.773502691896255534, -1.060575238724906372E-15 ) ) ;
#69734 = CARTESIAN_POINT ( 'NONE',  ( 27.52500000000000213, 6.123233995736764310E-16, -4.999999999999998224 ) ) ;
#69735 = CARTESIAN_POINT ( 'NONE',  ( 13.28437500061451715, -4.541064518000419881, 2.621784821874995952 ) ) ;
#69736 = CARTESIAN_POINT ( 'NONE',  ( 2.483674929639041906, 4.345807424128183882, 26.85429492329592804 ) ) ;
#69737 = CARTESIAN_POINT ( 'NONE',  ( 13.01250000122903394, 0.000000000000000000, 4.999999999999998224 ) ) ;
#69738 = CARTESIAN_POINT ( 'NONE',  ( 20.96250000122903145, 4.330127018922192761, -2.499999999999997780 ) ) ;
#69739 = CARTESIAN_POINT ( 'NONE',  ( 18.21562500061451573, -6.054752690667223547, -1.112240025338166033E-15 ) ) ;
#69740 =( BOUNDED_CURVE ( )  B_SPLINE_CURVE ( 2, ( #44503, #67036, #16396, #38951, #61469, #10864, #33397 ),
 .UNSPECIFIED., .F., .F. ) 
 B_SPLINE_CURVE_WITH_KNOTS ( ( 3, 2, 2, 3 ),
 ( 0.6916666666666666519, 0.6944444444444444198, 0.6972222222222221877, 0.6999999999999999556 ),
 .UNSPECIFIED. ) 
 CURVE ( )  GEOMETRIC_REPRESENTATION_ITEM ( )  RATIONAL_B_SPLINE_CURVE ( ( 1.000000000000000000, 0.8660254037844387076, 1.000000000000000000, 0.8660254037844387076, 1.000000000000000000, 0.8660254037844387076, 1.000000000000000000 ) ) 
 REPRESENTATION_ITEM ( '' )  );
#69741 = CARTESIAN_POINT ( 'NONE',  ( 21.02812500061451573, 6.421520780324663323E-16, -5.243569643749999010 ) ) ;
#69742 = CARTESIAN_POINT ( 'NONE',  ( 29.51250000122903216, 4.330127018922192761, -2.499999999999997780 ) ) ;
#69743 = CARTESIAN_POINT ( 'NONE',  ( 27.07499999999999929, 6.123233995736764310E-16, -4.999999999999998224 ) ) ;
#69744 = CARTESIAN_POINT ( 'NONE',  ( 5.000000000000000000, 6.176262757673013563E-16, -5.043301270189223473 ) ) ;
#69745 = CARTESIAN_POINT ( 'NONE',  ( 29.13749999999999929, -2.886751345948129988, 4.999999999999997335 ) ) ;
#69746 = CARTESIAN_POINT ( 'NONE',  ( 28.69687500061451502, -3.027376345333610441, -5.243569643749999898 ) ) ;
#69747 = CARTESIAN_POINT ( 'NONE',  ( 1.999999999999998668, 14.45000000000000107, -33.46410161513775705 ) ) ;
#69748 = CARTESIAN_POINT ( 'NONE',  ( -3.000416591977282496E-16, 14.79687500061451821, -34.90005215228797653 ) ) ;
#69749 = CARTESIAN_POINT ( 'NONE',  ( 4.537500001229034297, -4.330127018922194537, 2.499999999999995559 ) ) ;
#69750 = CARTESIAN_POINT ( 'NONE',  ( 6.075000000000000178, 4.330127018922191873, 2.499999999999999556 ) ) ;
#69751 = DIRECTION ( 'NONE',  ( 0.000000000000000000, 0.000000000000000000, 1.000000000000000000 ) ) ;
#69752 = CARTESIAN_POINT ( 'NONE',  ( 9.684375000614517504, -4.541064518000419881, 2.621784821874995952 ) ) ;
#69753 = CARTESIAN_POINT ( 'NONE',  ( 28.22812500061451502, 6.421520780324663323E-16, -5.243569643749999010 ) ) ;
#69754 = CARTESIAN_POINT ( 'NONE',  ( 15.43125000122903323, 6.123233995736764310E-16, -4.999999999999998224 ) ) ;
#69755 = CARTESIAN_POINT ( 'NONE',  ( 5.550000001229033586, -2.886751345948126435, -5.000000000000000000 ) ) ;
#69756 = CARTESIAN_POINT ( 'NONE',  ( 15.26250000122903216, 0.000000000000000000, 4.999999999999998224 ) ) ;
#69757 = ADVANCED_FACE ( 'NONE', ( #38236 ), #31235, .T. ) ;
#69758 = CARTESIAN_POINT ( 'NONE',  ( 8.671875000614518214, 3.027376345333611329, 5.243569643749999010 ) ) ;
#69759 = CARTESIAN_POINT ( 'NONE',  ( 10.65937500061451715, -4.541064518000417216, -2.621784821875001281 ) ) ;
#69760 = CARTESIAN_POINT ( 'NONE',  ( 4.650000000000001243, 4.330127018922192761, -2.499999999999997780 ) ) ;
#69761 = CARTESIAN_POINT ( 'NONE',  ( 2.121784821875001281, 14.55312500061459602, 33.67503911421598417 ) ) ;
#69762 = CARTESIAN_POINT ( 'NONE',  ( 2.733878782416514941, -4.186395442746991158, 2.733878782416514941 ) ) ;
#69763 = CARTESIAN_POINT ( 'NONE',  ( 5.662500000000000533, 2.886751345948126879, 4.999999999999999112 ) ) ;
#69764 = CARTESIAN_POINT ( 'NONE',  ( 15.12187500061451573, 5.824947211148865298E-16, -4.756430356249998326 ) ) ;
#69765 = CARTESIAN_POINT ( 'NONE',  ( 20.35312500061451502, 0.000000000000000000, 5.243569643749999010 ) ) ;
#69766 = CARTESIAN_POINT ( 'NONE',  ( 12.29062500061451857, -3.027376345333614438, 5.243569643749998122 ) ) ;
#69767 = CARTESIAN_POINT ( 'NONE',  ( 22.84687500061451360, 4.119189519843966529, -2.378215178124998275 ) ) ;
#69768 = CARTESIAN_POINT ( 'NONE',  ( 9.234375000614518214, -4.541064518000419881, 2.621784821874995952 ) ) ;
#69769 = CARTESIAN_POINT ( 'NONE',  ( 25.72499999999999787, 6.123233995736764310E-16, -4.999999999999998224 ) ) ;
#69770 = CARTESIAN_POINT ( 'NONE',  ( 22.35000000122903074, 5.773502691896255534, 3.535250795749688894E-16 ) ) ;
#69771 = CARTESIAN_POINT ( 'NONE',  ( -2.000000000000000000, 18.23750000122903359, -33.46410161513775705 ) ) ;
#69772 = CARTESIAN_POINT ( 'NONE',  ( 11.18437500061451928, 6.421520780324663323E-16, -5.243569643749999010 ) ) ;
#69773 = CARTESIAN_POINT ( 'NONE',  ( 25.65937500061451715, 4.541064518000418104, -2.621784821874998173 ) ) ;
#69774 = CARTESIAN_POINT ( 'NONE',  ( 4.059375000614519280, 4.541064518000418104, -2.621784821874998173 ) ) ;
#69775 = CARTESIAN_POINT ( 'NONE',  ( 24.30000000122903359, -2.886751345948163738, 4.999999999999939604 ) ) ;
#69776 = CARTESIAN_POINT ( 'NONE',  ( 19.99687500061451573, -3.027376345333614438, 5.243569643749998122 ) ) ;
#69777 =( BOUNDED_CURVE ( )  B_SPLINE_CURVE ( 2, ( #27446, #65495, #54422, #37785, #3822, #42966, #14885 ),
 .UNSPECIFIED., .F., .F. ) 
 B_SPLINE_CURVE_WITH_KNOTS ( ( 3, 2, 2, 3 ),
 ( 0.1699999999999999567, 0.1733333333333332837, 0.1766666666666666108, 0.1799999999999999378 ),
 .UNSPECIFIED. ) 
 CURVE ( )  GEOMETRIC_REPRESENTATION_ITEM ( )  RATIONAL_B_SPLINE_CURVE ( ( 1.000000000000002220, 0.8660254037844364872, 1.000000000000000000, 0.8660254037844387076, 1.000000000000000000, 0.8660254037844409281, 0.9999999999999977796 ) ) 
 REPRESENTATION_ITEM ( '' )  );
#69778 = CARTESIAN_POINT ( 'NONE',  ( 11.85937500061451644, 0.000000000000000000, 5.243569643749999010 ) ) ;
#69779 = CARTESIAN_POINT ( 'NONE',  ( -1.878215178124999163, 18.75312499938548427, 26.74683588394047007 ) ) ;
#69780 = CARTESIAN_POINT ( 'NONE',  ( 23.36250000000000071, -5.773502691896255534, -1.060575238724906372E-15 ) ) ;
#69781 = CARTESIAN_POINT ( 'NONE',  ( -8.484601909799255319E-16, 12.83750000000000036, 34.61880215351700940 ) ) ;
#69782 = CARTESIAN_POINT ( 'NONE',  ( 4.243569643749999898, 11.98437500061451821, -30.00000000000000000 ) ) ;
#69783 = CARTESIAN_POINT ( 'NONE',  ( 25.73437500061451644, 4.119189519843966529, 2.378215178124999607 ) ) ;
#69784 = CARTESIAN_POINT ( 'NONE',  ( 13.86562500061451431, 3.027376345333613106, -5.243569643749998122 ) ) ;
#69785 = CARTESIAN_POINT ( 'NONE',  ( 5.700000000000000178, 0.000000000000000000, 4.999999999999998224 ) ) ;
#69786 = CYLINDRICAL_SURFACE ( 'NONE', #56135, 4.999999999999998224 ) ;
#69787 = CARTESIAN_POINT ( 'NONE',  ( -1.071796769724504328, 12.89240381056766616, 33.99999999999999289 ) ) ;
#69788 =( BOUNDED_CURVE ( )  B_SPLINE_CURVE ( 2, ( #35783, #7717, #52062, #30251, #47243, #69775, #13610 ),
 .UNSPECIFIED., .F., .F. ) 
 B_SPLINE_CURVE_WITH_KNOTS ( ( 3, 2, 2, 3 ),
 ( 0.1916666666666666519, 0.1944444444444444198, 0.1972222222222221599, 0.1999999999999999556 ),
 .UNSPECIFIED. ) 
 CURVE ( )  GEOMETRIC_REPRESENTATION_ITEM ( )  RATIONAL_B_SPLINE_CURVE ( ( 1.000000000000001332, 0.8660254037844373753, 1.000000000000000000, 0.8660254037844387076, 1.000000000000000000, 0.8660254037844413721, 0.9999999999999973355 ) ) 
 REPRESENTATION_ITEM ( '' )  );
#69789 = CARTESIAN_POINT ( 'NONE',  ( 14.06250000000000000, 2.886751345948129099, -4.999999999999998224 ) ) ;
#69790 = CARTESIAN_POINT ( 'NONE',  ( 2.121784821875001281, 10.95312500061451821, 33.67503911421598417 ) ) ;
#69791 = CARTESIAN_POINT ( 'NONE',  ( 13.08750000122903323, -4.330127018922194537, 2.499999999999995559 ) ) ;
#69792 = CARTESIAN_POINT ( 'NONE',  ( 24.64687500061451431, -3.027376345333610441, -5.243569643749999898 ) ) ;
#69793 = CARTESIAN_POINT ( 'NONE',  ( 20.43750000122903643, 6.123233995736764310E-16, -4.999999999999998224 ) ) ;
#69794 = VERTEX_POINT ( 'NONE', #53776 ) ;
#69795 = CARTESIAN_POINT ( 'NONE',  ( 19.94062500061451715, -3.027376345333614438, 5.243569643749998122 ) ) ;
#69796 = CARTESIAN_POINT ( 'NONE',  ( 5.203125000614518214, -4.541064518000417216, -2.621784821875001281 ) ) ;
#69797 = CARTESIAN_POINT ( 'NONE',  ( 19.02187500061451786, 3.027376345333611329, 5.243569643749999010 ) ) ;
#69798 = CARTESIAN_POINT ( 'NONE',  ( 29.82187500061451502, 3.027376345333611329, 5.243569643749999010 ) ) ;
#69799 = CARTESIAN_POINT ( 'NONE',  ( 6.890625000614516438, -3.027376345333614438, 5.243569643749998122 ) ) ;
#69800 = CARTESIAN_POINT ( 'NONE',  ( 22.75312500061451360, -4.541064518000417216, -2.621784821875001281 ) ) ;
#69801 = CARTESIAN_POINT ( 'NONE',  ( -2.121784821874996840, 14.02812500061451750, 33.67503911421598417 ) ) ;
#69802 = CARTESIAN_POINT ( 'NONE',  ( 17.85000000122903430, 5.773502691896255534, 3.535250795749688894E-16 ) ) ;
#69803 = CARTESIAN_POINT ( 'NONE',  ( 12.72187500061451537, 2.746126346562643317, 4.756430356249998326 ) ) ;
#69804 = CARTESIAN_POINT ( 'NONE',  ( 10.64062500061451466, -3.027376345333610441, -5.243569643749999898 ) ) ;
#69805 = CARTESIAN_POINT ( 'NONE',  ( 3.721875000614518036, 3.027376345333611329, 5.243569643749999010 ) ) ;
#69806 = CARTESIAN_POINT ( 'NONE',  ( 28.86562500061451786, 3.027376345333611329, 5.243569643749999010 ) ) ;
#69807 = CARTESIAN_POINT ( 'NONE',  ( 22.20937500061451431, 0.000000000000000000, 5.243569643749999010 ) ) ;
#69808 = CARTESIAN_POINT ( 'NONE',  ( 15.10312500061451502, -4.541064518000417216, -2.621784821875001281 ) ) ;
#69809 = CARTESIAN_POINT ( 'NONE',  ( 23.92500000122903359, -5.773502691896255534, -1.060575238724906372E-15 ) ) ;
#69810 =( BOUNDED_CURVE ( )  B_SPLINE_CURVE ( 2, ( #62070, #384, #39546, #22539, #51349, #56524, #40268 ),
 .UNSPECIFIED., .F., .F. ) 
 B_SPLINE_CURVE_WITH_KNOTS ( ( 3, 2, 2, 3 ),
 ( 0.2100000000000000477, 0.2133333333333333748, 0.2166666666666667018, 0.2200000000000000011 ),
 .UNSPECIFIED. ) 
 CURVE ( )  GEOMETRIC_REPRESENTATION_ITEM ( )  RATIONAL_B_SPLINE_CURVE ( ( 0.9999999999999977796, 0.8660254037844409281, 1.000000000000000000, 0.8660254037844387076, 1.000000000000000000, 0.8660254037844387076, 1.000000000000000000 ) ) 
 REPRESENTATION_ITEM ( '' )  );
#69811 = CARTESIAN_POINT ( 'NONE',  ( 26.39062500061451644, -3.027376345333610441, -5.243569643749999898 ) ) ;
#69812 = CARTESIAN_POINT ( 'NONE',  ( 20.52187500061451786, -6.054752690667223547, -1.112240025338166033E-15 ) ) ;
#69813 = CARTESIAN_POINT ( 'NONE',  ( 14.27812500061451573, 6.421520780324663323E-16, -5.243569643749999010 ) ) ;
#69814 = CARTESIAN_POINT ( 'NONE',  ( 4.243569643749999898, 15.99687500061451573, 32.45002607614398471 ) ) ;
#69815 = CARTESIAN_POINT ( 'NONE',  ( 20.01562500061451644, -6.054752690667223547, -1.112240025338166033E-15 ) ) ;
#69816 = CARTESIAN_POINT ( 'NONE',  ( 30.00000000000000000, 0.000000000000000000, 0.000000000000000000 ) ) ;
#69817 = ORIENTED_EDGE ( 'NONE', *, *, #68436, .T. ) ;
#69818 = CARTESIAN_POINT ( 'NONE',  ( 26.02499999999999858, -4.330127018922194537, 2.499999999999995559 ) ) ;
#69819 = CARTESIAN_POINT ( 'NONE',  ( 3.999999999999998668, 11.71250000000000036, -32.30940107675850470 ) ) ;
#69820 = CARTESIAN_POINT ( 'NONE',  ( 1.878215178125000495, 20.47812499938548569, 26.74683588394047007 ) ) ;
#69821 = CARTESIAN_POINT ( 'NONE',  ( 27.36562500061451786, 3.027376345333613106, -5.243569643749998122 ) ) ;
#69822 = CARTESIAN_POINT ( 'NONE',  ( 8.915625000614515017, 3.027376345333613106, -5.243569643749998122 ) ) ;
#69823 = CARTESIAN_POINT ( 'NONE',  ( 20.36250000122903359, -4.330127018922190985, -2.500000000000001332 ) ) ;
#69824 = CARTESIAN_POINT ( 'NONE',  ( 25.26562500061451289, 3.027376345333611329, 5.243569643749999010 ) ) ;
#69826 = CARTESIAN_POINT ( 'NONE',  ( 25.01249999999999929, 2.886751345948126879, 4.999999999999999112 ) ) ;
#69825 = AXIS2_PLACEMENT_3D ( 'NONE', #66272, #59986, #21563 ) ;
#69827 = CARTESIAN_POINT ( 'NONE',  ( -2.828200636599751609E-16, 15.95000000122903216, -34.61880215351700230 ) ) ;
#69828 = CARTESIAN_POINT ( 'NONE',  ( 29.39062500061451289, -3.027376345333614438, 5.243569643749998122 ) ) ;
#69829 = CARTESIAN_POINT ( 'NONE',  ( 11.31562500061451892, 3.027376345333611329, 5.243569643749999010 ) ) ;
#69830 = ORIENTED_EDGE ( 'NONE', *, *, #15774, .F. ) ;
#69831 = EDGE_CURVE ( 'NONE', #26824, #65546, #33052, .T. ) ;
#69832 = CIRCLE ( 'NONE', #59199, 5.000000000000000000 ) ;
#69833 = CARTESIAN_POINT ( 'NONE',  ( 25.34062500061451217, -3.027376345333614438, 5.243569643749998122 ) ) ;
#69834 = CARTESIAN_POINT ( 'NONE',  ( 6.140625000614516438, -3.027376345333610441, -5.243569643749999898 ) ) ;
#69835 = CARTESIAN_POINT ( 'NONE',  ( 14.48437500061451821, 4.119189519843966529, 2.378215178124999607 ) ) ;
#69836 = CARTESIAN_POINT ( 'NONE',  ( 14.24999999999999822, 0.000000000000000000, 4.999999999999998224 ) ) ;
#69837 = CARTESIAN_POINT ( 'NONE',  ( 14.10937500061451644, 0.000000000000000000, 5.243569643749999010 ) ) ;
#69838 = CARTESIAN_POINT ( 'NONE',  ( 8.100000001229034297, -2.886751345948129988, 4.999999999999997335 ) ) ;
#69839 = CARTESIAN_POINT ( 'NONE',  ( 18.23437500061451999, -4.541064518000419881, 2.621784821874995952 ) ) ;
#69840 = CARTESIAN_POINT ( 'NONE',  ( 17.25000000000000000, 4.330127018922192761, -2.499999999999997780 ) ) ;
#69841 = CARTESIAN_POINT ( 'NONE',  ( 7.359375000614516438, 0.000000000000000000, 5.243569643749999010 ) ) ;
#69842 = CARTESIAN_POINT ( 'NONE',  ( 2.121784821875001281, 12.30312500061451608, -26.32496088578401938 ) ) ;
#69843 = CARTESIAN_POINT ( 'NONE',  ( 22.24687500061451573, -4.119189519843965641, -2.378215178125001383 ) ) ;
#69844 = FACE_OUTER_BOUND ( 'NONE', #41836, .T. ) ;
#69845 = CARTESIAN_POINT ( 'NONE',  ( 24.77812500061451217, 4.541064518000418104, 2.621784821874999949 ) ) ;
#69846 = CARTESIAN_POINT ( 'NONE',  ( -2.000000000000000000, 17.33750000122903145, 26.53589838486224650 ) ) ;
#69847 = CARTESIAN_POINT ( 'NONE',  ( 26.40937500061451715, -4.541064518000417216, -2.621784821875001281 ) ) ;
#69848 = CARTESIAN_POINT ( 'NONE',  ( 28.88437500061451502, 4.541064518000418104, 2.621784821874999949 ) ) ;
#69849 = CARTESIAN_POINT ( 'NONE',  ( 20.88749999999999929, 5.773502691896255534, 3.535250795749688894E-16 ) ) ;
#69850 = CARTESIAN_POINT ( 'NONE',  ( 6.628125000614517148, 6.421520780324663323E-16, -5.243569643749999010 ) ) ;
#69851 = CARTESIAN_POINT ( 'NONE',  ( 21.79687500061451644, -4.119189519843965641, -2.378215178125001383 ) ) ;
#69852 = CARTESIAN_POINT ( 'NONE',  ( 16.84687500061451715, -3.027376345333614438, 5.243569643749998122 ) ) ;
#69853 = CARTESIAN_POINT ( 'NONE',  ( 9.159375000614515372, -5.492252693125287522, -1.008910452111647106E-15 ) ) ;
#69854 = CARTESIAN_POINT ( 'NONE',  ( 3.440625000614518036, -3.027376345333610441, -5.243569643749999898 ) ) ;
#69855 = CARTESIAN_POINT ( 'NONE',  ( 7.846875000614518036, -3.027376345333614438, 5.243569643749998122 ) ) ;
#69856 = CARTESIAN_POINT ( 'NONE',  ( 18.94687500061451502, 6.054752690667223547, 3.707466751127219781E-16 ) ) ;
#69857 = CARTESIAN_POINT ( 'NONE',  ( -3.591883811668507676, 25.10396054455708637, 31.77987931115919906 ) ) ;
#69858 = CARTESIAN_POINT ( 'NONE',  ( 26.51249999999999929, -5.773502691896255534, -1.060575238724906372E-15 ) ) ;
#69860 = EDGE_CURVE ( 'NONE', #22838, #24963, #55244, .T. ) ;
#69859 = CARTESIAN_POINT ( 'NONE',  ( 27.83437500061451786, 6.421520780324663323E-16, -5.243569643749999010 ) ) ;
#69861 = CARTESIAN_POINT ( 'NONE',  ( 45.00000000000000000, 0.000000000000000000, 4.999999999999998224 ) ) ;
#69862 = ORIENTED_EDGE ( 'NONE', *, *, #53711, .F. ) ;
#69863 = CARTESIAN_POINT ( 'NONE',  ( 8.512499999999999289, -5.773502691896255534, -1.060575238724906372E-15 ) ) ;
#69864 = CARTESIAN_POINT ( 'NONE',  ( 12.75937500061451502, -5.492252693125287522, -1.008910452111647106E-15 ) ) ;
#69865 = CARTESIAN_POINT ( 'NONE',  ( 23.16562500061451502, -6.054752690667223547, -1.112240025338166033E-15 ) ) ;
#69866 = CARTESIAN_POINT ( 'NONE',  ( 11.92500000000000071, 4.330127018922191873, 2.499999999999999556 ) ) ;
#69867 = CARTESIAN_POINT ( 'NONE',  ( 8.400000001229035007, 5.773502691896255534, 3.535250795749688894E-16 ) ) ;
#69868 = CARTESIAN_POINT ( 'NONE',  ( 5.428125000614517859, 4.541064518000418104, 2.621784821874999949 ) ) ;
#69869 = CARTESIAN_POINT ( 'NONE',  ( 23.09999999999999787, 4.330127018922192761, -2.499999999999997780 ) ) ;
#69870 = CARTESIAN_POINT ( 'NONE',  ( 19.97812500061451502, -4.541064518000419881, 2.621784821874995952 ) ) ;
#69871 = FACE_OUTER_BOUND ( 'NONE', #2143, .T. ) ;
#69872 = VECTOR ( 'NONE', #3932, 1000.000000000000000 ) ;
#69873 = CARTESIAN_POINT ( 'NONE',  ( 26.02500000122903145, 2.886751345948126879, 4.999999999999999112 ) ) ;
#69874 = CARTESIAN_POINT ( 'NONE',  ( -3.756430356250000102, 18.71562499938548285, 30.00000000000000000 ) ) ;
#69875 = CARTESIAN_POINT ( 'NONE',  ( 4.162499999999999645, 2.886751345948129099, -4.999999999999998224 ) ) ;
#69876 = ORIENTED_EDGE ( 'NONE', *, *, #57675, .T. ) ;
#69877 = CARTESIAN_POINT ( 'NONE',  ( 18.40312500061451573, 4.541064518000418104, -2.621784821874998173 ) ) ;
#69878 = CARTESIAN_POINT ( 'NONE',  ( 26.16562500061451502, 3.027376345333611329, 5.243569643749999010 ) ) ;
#69879 = CARTESIAN_POINT ( 'NONE',  ( 26.25937500061451857, 0.000000000000000000, 5.243569643749999010 ) ) ;
#69880 = CARTESIAN_POINT ( 'NONE',  ( 14.31562500061451537, 3.027376345333613106, -5.243569643749998122 ) ) ;
#69881 = CARTESIAN_POINT ( 'NONE',  ( 28.07812500061451289, -4.541064518000419881, 2.621784821874995952 ) ) ;
#69882 = CARTESIAN_POINT ( 'NONE',  ( 8.278125000614515727, -4.541064518000419881, 2.621784821874995952 ) ) ;
#69883 = FACE_OUTER_BOUND ( 'NONE', #34526, .T. ) ;
#69884 = CARTESIAN_POINT ( 'NONE',  ( 27.37500000122903288, 2.886751345948126879, 4.999999999999999112 ) ) ;
#69885 = CARTESIAN_POINT ( 'NONE',  ( 20.63437500061451857, 5.824947211148865298E-16, -4.756430356249998326 ) ) ;
#69886 = CARTESIAN_POINT ( 'NONE',  ( 16.94062500061451715, -3.027376345333610441, -5.243569643749999898 ) ) ;
#69887 = CARTESIAN_POINT ( 'NONE',  ( -6.275039685470489619E-15, 18.31250000000000000, -26.00000000000000355 ) ) ;
#69888 = CARTESIAN_POINT ( 'NONE',  ( 28.84687500061452070, 6.054752690667223547, 3.707466751127219781E-16 ) ) ;
#69889 = CARTESIAN_POINT ( 'NONE',  ( 11.25937500061451679, 4.541064518000418104, -2.621784821874998173 ) ) ;
#69890 = CARTESIAN_POINT ( 'NONE',  ( 9.984375000614518214, 4.541064518000418104, 2.621784821874999949 ) ) ;
#69891 = CARTESIAN_POINT ( 'NONE',  ( 18.79687500061451644, -3.027376345333610441, -5.243569643749999898 ) ) ;
#69892 = ORIENTED_EDGE ( 'NONE', *, *, #64489, .F. ) ;
#69893 = CARTESIAN_POINT ( 'NONE',  ( 29.03437500061451715, -4.541064518000419881, 2.621784821874995952 ) ) ;
#69894 = CARTESIAN_POINT ( 'NONE',  ( 21.59062500061451928, 6.054752690667223547, 3.707466751127219781E-16 ) ) ;
#69895 = CARTESIAN_POINT ( 'NONE',  ( 17.22187500061451715, 3.027376345333611329, 5.243569643749999010 ) ) ;
#69896 = CARTESIAN_POINT ( 'NONE',  ( 22.19062500061451715, -3.027376345333614438, 5.243569643749998122 ) ) ;
#69897 = CARTESIAN_POINT ( 'NONE',  ( 3.999999999999999112, 14.37500000000000000, 30.00000000000000000 ) ) ;
#69898 = CARTESIAN_POINT ( 'NONE',  ( 28.07812500061451289, -4.541064518000419881, 2.621784821874995952 ) ) ;
#69899 = CARTESIAN_POINT ( 'NONE',  ( 10.08750000122903323, 6.123233995736764310E-16, -4.999999999999998224 ) ) ;
#69900 = EDGE_LOOP ( 'NONE', ( #59445, #52228, #56687, #57042 ) ) ;
#69901 = CARTESIAN_POINT ( 'NONE',  ( 4.650000001229035895, -2.886751345948125991, -5.000000000000000000 ) ) ;
#69902 = CARTESIAN_POINT ( 'NONE',  ( -2.000000000000000000, 18.12500000000000355, -33.46410161513775705 ) ) ;
#69903 = CARTESIAN_POINT ( 'NONE',  ( 23.88750000122903216, -4.330127018922194537, 2.499999999999995559 ) ) ;
#69904 = CARTESIAN_POINT ( 'NONE',  ( 4.000000000000000000, 20.13124999877096499, 27.69059892324149530 ) ) ;
#69905 = CARTESIAN_POINT ( 'NONE',  ( 6.234375000614519102, 6.421520780324663323E-16, -5.243569643749999010 ) ) ;
#69906 = CARTESIAN_POINT ( 'NONE',  ( 9.337500000000002132, -2.886751345948074920, 5.000000000000092371 ) ) ;
#69907 = CARTESIAN_POINT ( 'NONE',  ( 15.59062500061451573, -3.027376345333610441, -5.243569643749999898 ) ) ;
#69908 = CARTESIAN_POINT ( 'NONE',  ( 11.48437500061451644, -4.541064518000419881, 2.621784821874995952 ) ) ;
#69909 = CARTESIAN_POINT ( 'NONE',  ( 26.47500000122903074, 2.886751345948126879, 4.999999999999999112 ) ) ;
#69910 = CARTESIAN_POINT ( 'NONE',  ( 18.49687500061452283, 6.054752690667223547, 3.707466751127219781E-16 ) ) ;
#69911 = CARTESIAN_POINT ( 'NONE',  ( 5.746875000614517504, -3.027376345333610441, -5.243569643749999898 ) ) ;
#69912 = CARTESIAN_POINT ( 'NONE',  ( 3.999999999999999112, 17.52499999999999858, -30.00000000000000000 ) ) ;
#69913 = CARTESIAN_POINT ( 'NONE',  ( 7.678125000614516082, 4.541064518000418104, 2.621784821874999949 ) ) ;
#69914 = CARTESIAN_POINT ( 'NONE',  ( 17.65312500061451573, 0.000000000000000000, 5.243569643749999010 ) ) ;
#69915 = ORIENTED_EDGE ( 'NONE', *, *, #37745, .F. ) ;
#69916 = CARTESIAN_POINT ( 'NONE',  ( 14.54062500061451679, -3.027376345333614438, 5.243569643749998122 ) ) ;
#69917 = CARTESIAN_POINT ( 'NONE',  ( 10.49062500061451431, -3.027376345333614438, 5.243569643749998122 ) ) ;
#69918 = CARTESIAN_POINT ( 'NONE',  ( 20.37187500061451573, 2.746126346562643317, 4.756430356249998326 ) ) ;
#69919 = CARTESIAN_POINT ( 'NONE',  ( 10.65000000000000036, 0.000000000000000000, 4.999999999999998224 ) ) ;
#69920 = CARTESIAN_POINT ( 'NONE',  ( 6.037500001229035185, 6.123233995736764310E-16, -4.999999999999998224 ) ) ;
#69921 = EDGE_CURVE ( 'NONE', #37790, #37474, #71127, .T. ) ;
#69922 = CARTESIAN_POINT ( 'NONE',  ( 15.75937500061451857, 4.541064518000418104, -2.621784821874998173 ) ) ;
#69923 = AXIS2_PLACEMENT_3D ( 'NONE', #38420, #44343, #55777 ) ;
#69924 = CARTESIAN_POINT ( 'NONE',  ( 16.42500000122903359, 2.886751345948129099, -4.999999999999998224 ) ) ;
#69925 = CARTESIAN_POINT ( 'NONE',  ( 23.69999999999999929, 0.000000000000000000, 4.999999999999998224 ) ) ;
#69926 = CARTESIAN_POINT ( 'NONE',  ( -4.243569643749999898, 18.86562500061451431, -32.45002607614398471 ) ) ;
#69927 = CARTESIAN_POINT ( 'NONE',  ( 12.00000000122903465, 5.773502691896255534, 3.535250795749688401E-16 ) ) ;
#69928 = CARTESIAN_POINT ( 'NONE',  ( -1.071796769724488563, 18.74240381056766935, 34.00000000000000000 ) ) ;
#69929 = CYLINDRICAL_SURFACE ( 'NONE', #7650, 3.999999999999996447 ) ;
#69930 = DIRECTION ( 'NONE',  ( 1.000000000000000000, 0.000000000000000000, 0.000000000000000000 ) ) ;
#69931 = CARTESIAN_POINT ( 'NONE',  ( 4.764378199515531875, -1.525943107988289249, -4.942298803467851442 ) ) ;
#69932 = CARTESIAN_POINT ( 'NONE',  ( 16.54687500061451644, -3.027376345333610441, -5.243569643749999898 ) ) ;
#69933 = CARTESIAN_POINT ( 'NONE',  ( 18.13125000122903074, 6.123233995736764310E-16, -4.999999999999998224 ) ) ;
#69934 = CARTESIAN_POINT ( 'NONE',  ( 13.00312500061451537, 4.541064518000418104, -2.621784821874998173 ) ) ;
#69935 = CARTESIAN_POINT ( 'NONE',  ( 7.706250001229031810, -4.330127018922190985, -2.500000000000001332 ) ) ;
#69936 = CARTESIAN_POINT ( 'NONE',  ( 23.10937500061451644, 0.000000000000000000, 5.243569643749999010 ) ) ;
#69937 = CARTESIAN_POINT ( 'NONE',  ( 16.05937500061451573, 2.746126346562645981, -4.756430356249997438 ) ) ;
#69938 = CARTESIAN_POINT ( 'NONE',  ( 9.815625000614518925, 3.027376345333613106, -5.243569643749998122 ) ) ;
#69939 = CARTESIAN_POINT ( 'NONE',  ( 14.78437500061451715, 6.421520780324663323E-16, -5.243569643749999010 ) ) ;
#69940 = ORIENTED_EDGE ( 'NONE', *, *, #17942, .F. ) ;
#69941 = CARTESIAN_POINT ( 'NONE',  ( 26.55937500061451573, 4.541064518000418104, -2.621784821874998173 ) ) ;
#69942 = CARTESIAN_POINT ( 'NONE',  ( 28.15312500061451573, -4.541064518000417216, -2.621784821875001281 ) ) ;
#69943 = CARTESIAN_POINT ( 'NONE',  ( 16.75312500061451715, 0.000000000000000000, 5.243569643749999010 ) ) ;
#69944 = CARTESIAN_POINT ( 'NONE',  ( 3.126873471466460330, 3.901623033231208737, -3.503192874424200465 ) ) ;
#69945 = CARTESIAN_POINT ( 'NONE',  ( 4.890128389269437825, 1.043072884460970684, -5.138907771842282202 ) ) ;
#69946 = CARTESIAN_POINT ( 'NONE',  ( 8.662499999999999645, 2.886751345948129099, -4.999999999999998224 ) ) ;
#69947 = CARTESIAN_POINT ( 'NONE',  ( 19.16250000122903430, 4.330127018922192761, -2.499999999999997780 ) ) ;
#69948 = CARTESIAN_POINT ( 'NONE',  ( -1.071796769724490783, 18.85490381179670649, -26.00000000000000355 ) ) ;
#69949 = CARTESIAN_POINT ( 'NONE',  ( 10.77187500061451608, 4.119189519843966529, 2.378215178124999607 ) ) ;
#69950 = EDGE_LOOP ( 'NONE', ( #59091, #20875, #63588, #49648 ) ) ;
#69951 = CARTESIAN_POINT ( 'NONE',  ( 16.50000000000000000, 0.000000000000000000, 4.999999999999998224 ) ) ;
#69952 = CARTESIAN_POINT ( 'NONE',  ( 18.71249999999999858, 2.886751345948126879, 4.999999999999999112 ) ) ;
#69953 = CARTESIAN_POINT ( 'NONE',  ( 19.95937500061451786, 0.000000000000000000, 5.243569643749999010 ) ) ;
#69954 = CARTESIAN_POINT ( 'NONE',  ( 14.72812500061451679, 6.421520780324663323E-16, -5.243569643749999010 ) ) ;
#69955 = ORIENTED_EDGE ( 'NONE', *, *, #61665, .T. ) ;
#69956 = CARTESIAN_POINT ( 'NONE',  ( 28.46249999999999503, 2.886751345948125103, -5.000000000000004441 ) ) ;
#69957 = CARTESIAN_POINT ( 'NONE',  ( 5.428125000614517859, 4.541064518000418104, 2.621784821874999949 ) ) ;
#69958 = CARTESIAN_POINT ( 'NONE',  ( 19.89375000122903714, -2.886751345948181946, -4.999999999999904077 ) ) ;
#69959 = CARTESIAN_POINT ( 'NONE',  ( 11.92500000000000071, 4.330127018922191873, 2.499999999999999556 ) ) ;
#69960 = CARTESIAN_POINT ( 'NONE',  ( 27.38437500061451502, 5.492252693125287522, 3.363034840372157021E-16 ) ) ;
#69961 = CARTESIAN_POINT ( 'NONE',  ( 4.243569643749999898, 15.04062500061451679, 32.45002607614398471 ) ) ;
#69962 = CARTESIAN_POINT ( 'NONE',  ( 25.82812500061451644, -4.541064518000419881, 2.621784821874995952 ) ) ;
#69963 = CARTESIAN_POINT ( 'NONE',  ( 7.987500000000000711, -2.886751345948129988, 4.999999999999997335 ) ) ;
#69964 = CARTESIAN_POINT ( 'NONE',  ( -1.878215178124999163, 17.29062499938548214, 26.74683588394047007 ) ) ;
#69965 = CARTESIAN_POINT ( 'NONE',  ( 24.94687500061451502, -3.027376345333614438, 5.243569643749998122 ) ) ;
#69966 = ORIENTED_EDGE ( 'NONE', *, *, #27421, .T. ) ;
#69967 = CARTESIAN_POINT ( 'NONE',  ( 20.80312500061451431, 0.000000000000000000, 5.243569643749999010 ) ) ;
#69968 = CARTESIAN_POINT ( 'NONE',  ( 23.03437500061451715, 4.541064518000418104, 2.621784821874999949 ) ) ;
#69969 = ADVANCED_FACE ( 'NONE', ( #21241 ), #43793, .F. ) ;
#69970 = CARTESIAN_POINT ( 'NONE',  ( 2.121784821874999061, 16.50312500061459176, -33.67503911421598417 ) ) ;
#69971 = CARTESIAN_POINT ( 'NONE',  ( 6.290625000614517681, 6.054752690667223547, 3.707466751127219781E-16 ) ) ;
#69972 = CARTESIAN_POINT ( 'NONE',  ( 26.74687500061451573, -2.746126346562646425, 4.756430356249996549 ) ) ;
#69973 = CARTESIAN_POINT ( 'NONE',  ( 24.55312500061451786, -4.541064518000417216, -2.621784821875001281 ) ) ;
#69974 = CARTESIAN_POINT ( 'NONE',  ( 9.459375000614517859, 4.119189519843966529, -2.378215178124998275 ) ) ;
#69975 = CARTESIAN_POINT ( 'NONE',  ( -3.756430356250001434, 15.15312499938548463, 32.16877607737301048 ) ) ;
#69976 = CARTESIAN_POINT ( 'NONE',  ( 17.59687500061451715, 6.054752690667223547, 3.707466751127219781E-16 ) ) ;
#69977 = CARTESIAN_POINT ( 'NONE',  ( 24.08437500061451786, -4.541064518000419881, 2.621784821874995952 ) ) ;
#69978 = CARTESIAN_POINT ( 'NONE',  ( 4.243569643749999010, 14.72187500061451715, 27.54997392385601174 ) ) ;
#69979 = CARTESIAN_POINT ( 'NONE',  ( 7.490625000614516082, -3.027376345333610441, -5.243569643749999898 ) ) ;
#69980 = CARTESIAN_POINT ( 'NONE',  ( 27.89062500061451289, 6.054752690667223547, 3.707466751127219781E-16 ) ) ;
#69981 = CARTESIAN_POINT ( 'NONE',  ( 3.271875000614519635, 3.027376345333611329, 5.243569643749999010 ) ) ;
#69982 = CARTESIAN_POINT ( 'NONE',  ( 4.200000000000001954, 4.330127018922192761, -2.499999999999997780 ) ) ;
#69983 = CARTESIAN_POINT ( 'NONE',  ( 4.603125000614518569, 0.000000000000000000, 5.243569643749999010 ) ) ;
#69984 = CARTESIAN_POINT ( 'NONE',  ( 8.896875000614517859, -3.027376345333610441, -5.243569643749999898 ) ) ;
#69985 = SURFACE_STYLE_USAGE ( .BOTH. , #30465 ) ;
#69986 = CARTESIAN_POINT ( 'NONE',  ( 17.81250000122903288, 4.330127018922192761, -2.499999999999997780 ) ) ;
#69987 = CARTESIAN_POINT ( 'NONE',  ( 29.01562500061451644, -6.054752690667223547, -1.112240025338166033E-15 ) ) ;
#69988 = CARTESIAN_POINT ( 'NONE',  ( 5.128125000614516260, -4.541064518000419881, 2.621784821874995952 ) ) ;
#69989 = CARTESIAN_POINT ( 'NONE',  ( -3.999999999999999556, 13.98124999877096641, 27.69059892324149175 ) ) ;
#69990 = CARTESIAN_POINT ( 'NONE',  ( 21.46875000122903288, 2.886751345948126879, 4.999999999999999112 ) ) ;
#69991 = CARTESIAN_POINT ( 'NONE',  ( 15.87187500061451573, 3.027376345333611329, 5.243569643749999010 ) ) ;
#69992 = CARTESIAN_POINT ( 'NONE',  ( -1.999999999999997113, 10.62500000000000000, 33.46410161513775705 ) ) ;
#69993 = ORIENTED_EDGE ( 'NONE', *, *, #18715, .T. ) ;
#69994 = CARTESIAN_POINT ( 'NONE',  ( 22.49062500061451431, 6.054752690667223547, 3.707466751127219781E-16 ) ) ;
#69995 = CARTESIAN_POINT ( 'NONE',  ( 9.440625000614517148, 6.054752690667223547, 3.707466751127219781E-16 ) ) ;
#69996 = CARTESIAN_POINT ( 'NONE',  ( 24.42187500061451644, 3.027376345333611329, 5.243569643749999010 ) ) ;
#69997 = CARTESIAN_POINT ( 'NONE',  ( 7.115625000614516082, 3.027376345333613106, -5.243569643749998122 ) ) ;
#69998 = DIRECTION ( 'NONE',  ( 1.000000000000000000, -0.000000000000000000, -0.000000000000000000 ) ) ;
#69999 = CARTESIAN_POINT ( 'NONE',  ( 10.20000000122903572, 5.773502691896255534, 3.535250795749688894E-16 ) ) ;
#70000 = CARTESIAN_POINT ( 'NONE',  ( 26.05312500061451431, 4.541064518000418104, -2.621784821874998173 ) ) ;
#70001 = CARTESIAN_POINT ( 'NONE',  ( 4.243569643749999898, 10.54062500061451679, -27.54997392385601529 ) ) ;
#70002 = CARTESIAN_POINT ( 'NONE',  ( 13.38750000122903394, 4.330127018922191873, 2.499999999999999556 ) ) ;
#70003 = CARTESIAN_POINT ( 'NONE',  ( 22.34062500061451573, -3.027376345333610441, -5.243569643749999898 ) ) ;
#70004 = CARTESIAN_POINT ( 'NONE',  ( 18.29062500061451502, -3.027376345333610441, -5.243569643749999898 ) ) ;
#70005 = CARTESIAN_POINT ( 'NONE',  ( 18.80625000122903501, 0.000000000000000000, 4.999999999999998224 ) ) ;
#70006 = CARTESIAN_POINT ( 'NONE',  ( 19.16250000000000142, 2.886751345948126879, 4.999999999999999112 ) ) ;
#70007 = CARTESIAN_POINT ( 'NONE',  ( 12.63750000122903394, -4.330127018922194537, 2.499999999999995559 ) ) ;
#70008 = CARTESIAN_POINT ( 'NONE',  ( 11.35312500061451679, 0.000000000000000000, 5.243569643749999010 ) ) ;
#70009 = ADVANCED_FACE ( 'NONE', ( #42325 ), #64850, .F. ) ;
#70010 = CARTESIAN_POINT ( 'NONE',  ( 13.52812500061451750, 4.541064518000418104, 2.621784821874999949 ) ) ;
#70011 =( BOUNDED_CURVE ( )  B_SPLINE_CURVE ( 2, ( #4204, #14900, #21536, #5285, #27831, #42982, #31901 ),
 .UNSPECIFIED., .F., .F. ) 
 B_SPLINE_CURVE_WITH_KNOTS ( ( 3, 2, 2, 3 ),
 ( 0.5899999999999999689, 0.5933333333333333792, 0.5966666666666666785, 0.5999999999999999778 ),
 .UNSPECIFIED. ) 
 CURVE ( )  GEOMETRIC_REPRESENTATION_ITEM ( )  RATIONAL_B_SPLINE_CURVE ( ( 1.000000000000000000, 0.8660254037844387076, 1.000000000000000000, 0.8660254037844387076, 1.000000000000000000, 0.8660254037844387076, 1.000000000000000000 ) ) 
 REPRESENTATION_ITEM ( '' )  );
#70012 = CARTESIAN_POINT ( 'NONE',  ( 23.58750000122903145, 6.123233995736764310E-16, -4.999999999999998224 ) ) ;
#70013 = CARTESIAN_POINT ( 'NONE',  ( 22.84687500061451715, -3.027376345333610441, -5.243569643749999898 ) ) ;
#70014 = CARTESIAN_POINT ( 'NONE',  ( 21.75937500061451502, 0.000000000000000000, 5.243569643749999010 ) ) ;
#70015 = CARTESIAN_POINT ( 'NONE',  ( 8.400000001229035007, 5.773502691896255534, 3.535250795749688894E-16 ) ) ;
#70016 = CARTESIAN_POINT ( 'NONE',  ( 5.896875000614518747, 6.054752690667223547, 3.707466751127219781E-16 ) ) ;
#70017 = CARTESIAN_POINT ( 'NONE',  ( 24.49687500061451573, -3.027376345333614438, 5.243569643749998122 ) ) ;
#70018 = CARTESIAN_POINT ( 'NONE',  ( 4.603329117574985752, 1.951758446961684434, -4.603329117574985752 ) ) ;
#70019 = CARTESIAN_POINT ( 'NONE',  ( 22.15312500061451573, 0.000000000000000000, 5.243569643749999010 ) ) ;
#70020 = CARTESIAN_POINT ( 'NONE',  ( 26.97187500061451360, 3.027376345333613106, -5.243569643749998122 ) ) ;
#70021 = CARTESIAN_POINT ( 'NONE',  ( -3.756430356250000102, 17.47812499938548214, 30.00000000000000000 ) ) ;
#70022 = CARTESIAN_POINT ( 'NONE',  ( 45.00000000000000000, 0.000000000000000000, 0.000000000000000000 ) ) ;
#70023 = CARTESIAN_POINT ( 'NONE',  ( 16.55625000122903145, 0.000000000000000000, 4.999999999999998224 ) ) ;
#70024 = CARTESIAN_POINT ( 'NONE',  ( 5.521875000614517859, 3.027376345333611329, 5.243569643749999010 ) ) ;
#70025 = CARTESIAN_POINT ( 'NONE',  ( 16.52812500061451573, 6.421520780324663323E-16, -5.243569643749999010 ) ) ;
#70026 = EDGE_LOOP ( 'NONE', ( #4961, #15617, #13358, #62694 ) ) ;
#70027 = CARTESIAN_POINT ( 'NONE',  ( 22.87500000000000000, -4.330127018922194537, 2.499999999999995559 ) ) ;
#70028 = CARTESIAN_POINT ( 'NONE',  ( 25.11562500061451431, 3.027376345333613106, -5.243569643749998122 ) ) ;
#70029 = CARTESIAN_POINT ( 'NONE',  ( 3.009375000614516793, -4.541064518000417216, -2.621784821875001281 ) ) ;
#70030 = CARTESIAN_POINT ( 'NONE',  ( -3.999999999999999112, 15.91249999999999964, -32.30940107675850470 ) ) ;
#70031 = CARTESIAN_POINT ( 'NONE',  ( 7.303125000614516082, 0.000000000000000000, 4.999999999999998224 ) ) ;
#70032 = CARTESIAN_POINT ( 'NONE',  ( 16.16250000000000142, -5.773502691896255534, -1.060575238724906372E-15 ) ) ;
#70033 = CARTESIAN_POINT ( 'NONE',  ( 22.15312500061451573, 0.000000000000000000, 5.243569643749999010 ) ) ;
#70034 = ORIENTED_EDGE ( 'NONE', *, *, #64274, .T. ) ;
#70035 = CARTESIAN_POINT ( 'NONE',  ( 25.50000000000000000, 0.000000000000000000, 4.999999999999998224 ) ) ;
#70036 = CARTESIAN_POINT ( 'NONE',  ( 26.82187500061451857, -6.054752690667223547, -1.112240025338166033E-15 ) ) ;
#70037 = ORIENTED_EDGE ( 'NONE', *, *, #5968, .F. ) ;
#70038 = CARTESIAN_POINT ( 'NONE',  ( 25.87500000000000000, 4.330127018922191873, 2.499999999999999556 ) ) ;
#70039 = CARTESIAN_POINT ( 'NONE',  ( 14.05312500061451431, 0.000000000000000000, 5.243569643749999010 ) ) ;
#70040 = CARTESIAN_POINT ( 'NONE',  ( 6.815625000614517148, 3.027376345333611329, 5.243569643749999010 ) ) ;
#70041 = CARTESIAN_POINT ( 'NONE',  ( 16.05937500061451573, 2.746126346562645981, -4.756430356249997438 ) ) ;
#70042 = CARTESIAN_POINT ( 'NONE',  ( 29.57812500061451644, 6.421520780324663323E-16, -5.243569643749999010 ) ) ;
#70043 = CARTESIAN_POINT ( 'NONE',  ( 13.98750000122903359, -4.330127018922194537, 2.499999999999995559 ) ) ;
#70044 = CARTESIAN_POINT ( 'NONE',  ( 19.01249999999999929, 2.886751345948129099, -4.999999999999998224 ) ) ;
#70045 = CARTESIAN_POINT ( 'NONE',  ( 27.59999999999999787, 4.330127018922192761, -2.499999999999997780 ) ) ;
#70046 = CARTESIAN_POINT ( 'NONE',  ( 65.00000000000000000, -8.874999999999998224, -1.494782592887675232 ) ) ;
#70047 = CARTESIAN_POINT ( 'NONE',  ( 7.621875000614519280, 3.027376345333613106, -5.243569643749998122 ) ) ;
#70048 = CARTESIAN_POINT ( 'NONE',  ( 18.49687500061452283, 6.054752690667223547, 3.707466751127219781E-16 ) ) ;
#70049 = CARTESIAN_POINT ( 'NONE',  ( -5.810221930991193690E-16, 11.45000000122903216, 26.00000000000000355 ) ) ;
#70050 = ORIENTED_EDGE ( 'NONE', *, *, #56762, .T. ) ;
#70051 = CARTESIAN_POINT ( 'NONE',  ( 27.74062500061451431, -3.027376345333610441, -5.243569643749999898 ) ) ;
#70052 = CARTESIAN_POINT ( 'NONE',  ( 3.300000000000000711, 4.330127018922192761, -2.499999999999997780 ) ) ;
#70053 = CARTESIAN_POINT ( 'NONE',  ( 3.646875000614520079, 6.054752690667223547, 3.707466751127219781E-16 ) ) ;
#70054 = CARTESIAN_POINT ( 'NONE',  ( 16.42500000000000071, 4.330127018922191873, 2.499999999999999556 ) ) ;
#70055 = CARTESIAN_POINT ( 'NONE',  ( 13.60312500061451679, 0.000000000000000000, 5.243569643749999010 ) ) ;
#70056 = CARTESIAN_POINT ( 'NONE',  ( -2.498395430326213790E-14, 18.46250000000000213, 26.00000000000000000 ) ) ;
#70057 = DIRECTION ( 'NONE',  ( -1.000000000000000000, -0.000000000000000000, -0.000000000000000000 ) ) ;
#70058 = CARTESIAN_POINT ( 'NONE',  ( 18.18750000122903288, 6.123233995736764310E-16, -4.999999999999998224 ) ) ;
#70059 = CARTESIAN_POINT ( 'NONE',  ( 5.191822204397939622, 8.550203871005528811, 26.96813994412839222 ) ) ;
#70060 = CARTESIAN_POINT ( 'NONE',  ( 17.55937500061451573, 4.119189519843966529, -2.378215178124998275 ) ) ;
#70061 = CARTESIAN_POINT ( 'NONE',  ( 7.828125000614517326, -4.541064518000419881, 2.621784821874995952 ) ) ;
#70062 = CARTESIAN_POINT ( 'NONE',  ( 23.29687500061451644, -3.027376345333610441, -5.243569643749999898 ) ) ;
#70063 = CARTESIAN_POINT ( 'NONE',  ( 4.243569643749999898, 19.59687500061452070, 32.45002607614398471 ) ) ;
#70064 = ADVANCED_FACE ( 'NONE', ( #62587 ), #27898, .T. ) ;
#70065 = CARTESIAN_POINT ( 'NONE',  ( 22.88437500061451857, 6.421520780324663323E-16, -5.243569643749999010 ) ) ;
#70066 = CARTESIAN_POINT ( 'NONE',  ( 6.037500000000001421, 5.773502691896255534, 3.535250795749688894E-16 ) ) ;
#70067 = CARTESIAN_POINT ( 'NONE',  ( 3.999999999999999112, 10.43750000122903465, 30.00000000000000000 ) ) ;
#70068 = CARTESIAN_POINT ( 'NONE',  ( 14.61562500061451608, -6.054752690667223547, -1.112240025338166033E-15 ) ) ;
#70069 = CARTESIAN_POINT ( 'NONE',  ( 5.962500001229033231, -4.330127018922190985, -2.500000000000001332 ) ) ;
#70070 = CARTESIAN_POINT ( 'NONE',  ( 9.759375000614516793, -4.541064518000417216, -2.621784821875001281 ) ) ;
#70071 = CARTESIAN_POINT ( 'NONE',  ( -0.5524690355592173363, 4.971316854763022874, -26.03590284058948612 ) ) ;
#70072 = ORIENTED_EDGE ( 'NONE', *, *, #7700, .T. ) ;
#70073 = CARTESIAN_POINT ( 'NONE',  ( 12.92812500061451786, 6.421520780324663323E-16, -5.243569643749999010 ) ) ;
#70074 = CARTESIAN_POINT ( 'NONE',  ( 24.15000000122903145, 5.773502691896255534, 3.535250795749688894E-16 ) ) ;
#70075 = CARTESIAN_POINT ( 'NONE',  ( 10.62187500061451928, -6.054752690667223547, -1.112240025338166033E-15 ) ) ;
#70076 = CARTESIAN_POINT ( 'NONE',  ( 11.99062500061451608, -3.027376345333610441, -5.243569643749999898 ) ) ;
#70077 = CARTESIAN_POINT ( 'NONE',  ( 27.28125000122902932, 4.330127018922191873, 2.499999999999999556 ) ) ;
#70078 = CARTESIAN_POINT ( 'NONE',  ( 22.77187500061451786, -6.054752690667223547, -1.112240025338166033E-15 ) ) ;
#70079 = CARTESIAN_POINT ( 'NONE',  ( 8.550000000000002487, -4.330127018922190985, -2.500000000000001332 ) ) ;
#70080 = FACE_OUTER_BOUND ( 'NONE', #59079, .T. ) ;
#70081 = CARTESIAN_POINT ( 'NONE',  ( 14.81250000000000178, -5.773502691896255534, -1.060575238724906372E-15 ) ) ;
#70082 = CARTESIAN_POINT ( 'NONE',  ( -2.121784821874999949, 13.93437500061451750, -33.67503911421598417 ) ) ;
#70083 = CARTESIAN_POINT ( 'NONE',  ( 15.79687500061451821, 6.054752690667223547, 3.707466751127219781E-16 ) ) ;
#70084 = CARTESIAN_POINT ( 'NONE',  ( 16.98750000122903359, 4.330127018922191873, 2.499999999999999556 ) ) ;
#70085 = CARTESIAN_POINT ( 'NONE',  ( 12.00937500061451857, -4.541064518000417216, -2.621784821875001281 ) ) ;
#70086 = CARTESIAN_POINT ( 'NONE',  ( 4.243569643749999010, 17.81562500061451715, -32.45002607614398471 ) ) ;
#70087 = CARTESIAN_POINT ( 'NONE',  ( 20.55000000122903359, 5.773502691896255534, 3.535250795749688894E-16 ) ) ;
#70088 = CARTESIAN_POINT ( 'NONE',  ( 13.56562500061451892, 3.027376345333611329, 5.243569643749999010 ) ) ;
#70089 = AXIS2_PLACEMENT_3D ( 'NONE', #17582, #49778, #5792 ) ;
#70090 = ORIENTED_EDGE ( 'NONE', *, *, #2540, .T. ) ;
#70091 = VERTEX_POINT ( 'NONE', #11627 ) ;
#70092 = CARTESIAN_POINT ( 'NONE',  ( 15.59999999999999964, 0.000000000000000000, 4.999999999999998224 ) ) ;
#70093 = CARTESIAN_POINT ( 'NONE',  ( -3.999999999999997335, 17.45000000122903572, -27.69059892324149530 ) ) ;
#70094 = CARTESIAN_POINT ( 'NONE',  ( 12.23437500061451821, 4.541064518000418104, 2.621784821874999949 ) ) ;
#70095 = CARTESIAN_POINT ( 'NONE',  ( 2.675063744352810247, 4.229653939133389606, 27.01553149349311767 ) ) ;
#70096 = CARTESIAN_POINT ( 'NONE',  ( 13.27500000122903323, 2.886751345948129099, -4.999999999999998224 ) ) ;
#70097 = CARTESIAN_POINT ( 'NONE',  ( 20.17500000122903359, 2.886751345948126879, 4.999999999999999112 ) ) ;
#70098 = CARTESIAN_POINT ( 'NONE',  ( 17.69062500061451715, -3.027376345333614438, 5.243569643749998122 ) ) ;
#70099 = CARTESIAN_POINT ( 'NONE',  ( 20.31562500061451715, 3.027376345333611329, 5.243569643749999010 ) ) ;
#70100 = CARTESIAN_POINT ( 'NONE',  ( 28.20000000122903216, 5.773502691896255534, 3.535250795749688894E-16 ) ) ;
#70101 = ADVANCED_FACE ( 'NONE', ( #44164 ), #44536, .F. ) ;
#70102 = CARTESIAN_POINT ( 'NONE',  ( 27.82499999999999929, -4.330127018922194537, 2.499999999999995559 ) ) ;
#70103 = FACE_OUTER_BOUND ( 'NONE', #73099, .T. ) ;
#70104 = CARTESIAN_POINT ( 'NONE',  ( 29.28749999999999787, -2.886751345948125991, -5.000000000000000000 ) ) ;
#70105 = CARTESIAN_POINT ( 'NONE',  ( 26.97187500061451360, 3.027376345333613106, -5.243569643749998122 ) ) ;
#70106 = CARTESIAN_POINT ( 'NONE',  ( 20.38125000122903430, 6.123233995736764310E-16, -4.999999999999998224 ) ) ;
#70107 = CARTESIAN_POINT ( 'NONE',  ( 2.121784821874999061, 12.95937500061451786, -33.67503911421598417 ) ) ;
#70108 = DIRECTION ( 'NONE',  ( -1.000000000000000000, -0.000000000000000000, -0.000000000000000000 ) ) ;
#70109 = CARTESIAN_POINT ( 'NONE',  ( 5.137500000000000178, 5.773502691896255534, 3.535250795749688894E-16 ) ) ;
#70110 = CARTESIAN_POINT ( 'NONE',  ( 11.81250000000000000, 2.886751345948129099, -4.999999999999997335 ) ) ;
#70111 = CARTESIAN_POINT ( 'NONE',  ( 7.621875000614519280, 3.027376345333613106, -5.243569643749998122 ) ) ;
#70112 = CARTESIAN_POINT ( 'NONE',  ( 28.52812500061451573, -4.541064518000419881, 2.621784821874995952 ) ) ;
#70113 = CARTESIAN_POINT ( 'NONE',  ( 10.03125000122903288, 6.123233995736764310E-16, -4.999999999999998224 ) ) ;
#70114 = CARTESIAN_POINT ( 'NONE',  ( -3.968938398713114601, 9.180052406904112061, -25.49615315276739480 ) ) ;
#70115 = CARTESIAN_POINT ( 'NONE',  ( -3.999999999999999112, 19.21250000122903501, 30.00000000000000000 ) ) ;
#70116 = CARTESIAN_POINT ( 'NONE',  ( 6.234375000614519102, 6.421520780324663323E-16, -5.243569643749999010 ) ) ;
#70117 = CARTESIAN_POINT ( 'NONE',  ( 10.77187500061451786, 3.027376345333613106, -5.243569643749998122 ) ) ;
#70118 = CARTESIAN_POINT ( 'NONE',  ( 3.712499999999999911, 2.886751345948129099, -4.999999999999998224 ) ) ;
#70119 = CARTESIAN_POINT ( 'NONE',  ( 4.243569643749999898, 14.59062500061459744, 32.45002607614398471 ) ) ;
#70120 = CARTESIAN_POINT ( 'NONE',  ( 3.793609269539072404, 25.05402749099526005, 28.70526358585616578 ) ) ;
#70121 = CARTESIAN_POINT ( 'NONE',  ( 7.275000000000000355, 6.123233995736764310E-16, -4.999999999999998224 ) ) ;
#70122 = CARTESIAN_POINT ( 'NONE',  ( 16.02187500061451431, 5.824947211148865298E-16, -4.756430356249998326 ) ) ;
#70123 = CARTESIAN_POINT ( 'NONE',  ( 19.30312500061451786, 4.541064518000418104, -2.621784821874998173 ) ) ;
#70124 = CARTESIAN_POINT ( 'NONE',  ( 12.47812500061451502, 6.421520780324663323E-16, -5.243569643749999010 ) ) ;
#70125 = CARTESIAN_POINT ( 'NONE',  ( 24.15937500061451360, 2.746126346562645981, -4.756430356249997438 ) ) ;
#70126 = CARTESIAN_POINT ( 'NONE',  ( 9.084375000614517859, 4.541064518000418104, 2.621784821874999949 ) ) ;
#70127 = CARTESIAN_POINT ( 'NONE',  ( 25.46249999999999858, 2.886751345948126879, 4.999999999999999112 ) ) ;
#70128 = CARTESIAN_POINT ( 'NONE',  ( 21.75000000122903288, -2.886751345948125991, -5.000000000000000000 ) ) ;
#70129 = AXIS2_PLACEMENT_3D ( 'NONE', #41142, #69217, #1983 ) ;
#70130 = CARTESIAN_POINT ( 'NONE',  ( 2.000000000000001332, 10.81250000122903465, 33.46410161513774995 ) ) ;
#70131 = CARTESIAN_POINT ( 'NONE',  ( 9.646875000614516082, -3.027376345333614438, 5.243569643749998122 ) ) ;
#70132 = CARTESIAN_POINT ( 'NONE',  ( 26.55937500061451573, 4.541064518000418104, -2.621784821874998173 ) ) ;
#70133 = CARTESIAN_POINT ( 'NONE',  ( 4.211513410512504940, -3.870537385557588195, 3.783171883119448076 ) ) ;
#70134 = CARTESIAN_POINT ( 'NONE',  ( -1.626862140677534273E-15, 17.33749999999999858, 34.00000000000000000 ) ) ;
#70135 = CARTESIAN_POINT ( 'NONE',  ( 19.05937500061451928, 0.000000000000000000, 5.243569643749999010 ) ) ;
#70136 = CARTESIAN_POINT ( 'NONE',  ( 11.22187500061451892, 3.027376345333613106, -5.243569643749998122 ) ) ;
#70137 = CARTESIAN_POINT ( 'NONE',  ( -3.756430356250000102, 20.17812499938548143, 30.00000000000000000 ) ) ;
#70138 = CARTESIAN_POINT ( 'NONE',  ( 24.14999999999999858, 0.000000000000000000, 4.999999999999998224 ) ) ;
#70139 = CARTESIAN_POINT ( 'NONE',  ( 2.828200636599751609E-16, 15.31250000000000000, 25.38119784648299415 ) ) ;
#70140 = CARTESIAN_POINT ( 'NONE',  ( -2.121784821874996840, 13.18437500061451750, -26.32496088578401583 ) ) ;
#70141 = CARTESIAN_POINT ( 'NONE',  ( 25.13437500061451502, 5.824947211148865298E-16, -4.756430356249998326 ) ) ;
#70142 = CARTESIAN_POINT ( 'NONE',  ( 15.10312500061451502, -4.541064518000417216, -2.621784821875001281 ) ) ;
#70143 = CARTESIAN_POINT ( 'NONE',  ( 3.825000000000001954, 4.330127018922191873, 2.499999999999999556 ) ) ;
#70144 = CARTESIAN_POINT ( 'NONE',  ( 25.12499999999999645, -4.330127018922194537, 2.499999999999995559 ) ) ;
#70145 = CYLINDRICAL_SURFACE ( 'NONE', #37382, 4.999999999999998224 ) ;
#70146 = CARTESIAN_POINT ( 'NONE',  ( 15.29999999999999893, -4.330127018922190985, -2.500000000000001332 ) ) ;
#70147 = CARTESIAN_POINT ( 'NONE',  ( 4.243569643749999010, 10.61562500061451786, 27.54997392385601174 ) ) ;
#70148 = CARTESIAN_POINT ( 'NONE',  ( 12.97500000122903252, 2.886751345948126879, 4.999999999999999112 ) ) ;
#70149 = AXIS2_PLACEMENT_3D ( 'NONE', #10360, #72783, #22166 ) ;
#70150 = CARTESIAN_POINT ( 'NONE',  ( 23.74687500061451573, -3.027376345333610441, -5.243569643749999898 ) ) ;
#70151 = CARTESIAN_POINT ( 'NONE',  ( 18.45937500061451431, 4.541064518000418104, -2.621784821874998173 ) ) ;
#70152 = CYLINDRICAL_SURFACE ( 'NONE', #7694, 4.999999999999998224 ) ;
#70153 = ORIENTED_EDGE ( 'NONE', *, *, #4728, .T. ) ;
#70154 = CARTESIAN_POINT ( 'NONE',  ( 20.31562500061451715, 3.027376345333611329, 5.243569643749999010 ) ) ;
#70155 = AXIS2_PLACEMENT_3D ( 'NONE', #37679, #55773, #44701 ) ;
#70156 = CARTESIAN_POINT ( 'NONE',  ( 3.815625000614518036, -6.054752690667223547, -1.112240025338166033E-15 ) ) ;
#70157 = CARTESIAN_POINT ( 'NONE',  ( 17.18437500061451573, 4.541064518000418104, 2.621784821874999949 ) ) ;
#70158 = CARTESIAN_POINT ( 'NONE',  ( 27.87187500061451573, 3.027376345333613106, -5.243569643749998122 ) ) ;
#70159 = CARTESIAN_POINT ( 'NONE',  ( 5.578125000614518214, -4.541064518000419881, 2.621784821874995952 ) ) ;
#70160 = CARTESIAN_POINT ( 'NONE',  ( 22.90312500061451573, 4.541064518000418104, -2.621784821874998173 ) ) ;
#70161 = CARTESIAN_POINT ( 'NONE',  ( -4.243569643749997233, 15.79062500061451857, 32.45002607614398471 ) ) ;
#70162 = CARTESIAN_POINT ( 'NONE',  ( 16.98750000122903359, 4.330127018922191873, 2.499999999999999556 ) ) ;
#70163 = CARTESIAN_POINT ( 'NONE',  ( 13.13437500061451857, 4.119189519843966529, 2.378215178124999607 ) ) ;
#70164 = CARTESIAN_POINT ( 'NONE',  ( 6.740625000614515194, 6.054752690667223547, 3.707466751127219781E-16 ) ) ;
#70165 = CARTESIAN_POINT ( 'NONE',  ( 0.000000000000000000, 20.00000000000000000, -33.99999999999999289 ) ) ;
#70166 = CARTESIAN_POINT ( 'NONE',  ( 28.79062500061451502, 6.054752690667223547, 3.707466751127219781E-16 ) ) ;
#70167 =( BOUNDED_CURVE ( )  B_SPLINE_CURVE ( 2, ( #15047, #20579, #32779, #43871, #53858, #43504, #8780, #15407, #9150 ),
 .UNSPECIFIED., .F., .F. ) 
 B_SPLINE_CURVE_WITH_KNOTS ( ( 3, 2, 2, 2, 3 ),
 ( 0.3804347826086956763, 0.3840579710144927383, 0.3913043478260869734, 0.3985507246376811530, 0.4021739130434782705 ),
 .UNSPECIFIED. ) 
 CURVE ( )  GEOMETRIC_REPRESENTATION_ITEM ( )  RATIONAL_B_SPLINE_CURVE ( ( 0.9330127018922194093, 0.9330127018922198534, 1.000000000000000000, 0.8660254037844387076, 1.000000000000000000, 0.8660254037844387076, 1.000000000000000000, 0.9330127018922194093, 0.9330127018922194093 ) ) 
 REPRESENTATION_ITEM ( '' )  );
#70168 = CARTESIAN_POINT ( 'NONE',  ( 22.65937500061451715, 0.000000000000000000, 5.243569643749999010 ) ) ;
#70169 = CARTESIAN_POINT ( 'NONE',  ( 14.05312500061451431, 0.000000000000000000, 5.243569643749999010 ) ) ;
#70170 = CARTESIAN_POINT ( 'NONE',  ( 23.77500000122903145, 2.886751345948126879, 4.999999999999999112 ) ) ;
#70171 = CARTESIAN_POINT ( 'NONE',  ( 24.96562500061451573, -6.054752690667223547, -1.112240025338166033E-15 ) ) ;
#70172 = CARTESIAN_POINT ( 'NONE',  ( 20.55937500061451573, -4.541064518000417216, -2.621784821875001281 ) ) ;
#70173 = CARTESIAN_POINT ( 'NONE',  ( 14.84062500061451750, 6.054752690667223547, 3.707466751127219781E-16 ) ) ;
#70174 = CARTESIAN_POINT ( 'NONE',  ( -2.121784821874996840, 18.13437500061451502, 33.67503911421598417 ) ) ;
#70175 = CARTESIAN_POINT ( 'NONE',  ( 19.97812500061451502, -4.541064518000419881, 2.621784821874995952 ) ) ;
#70176 = EDGE_LOOP ( 'NONE', ( #73046, #40521 ) ) ;
#70177 = CARTESIAN_POINT ( 'NONE',  ( 26.13749999999999929, -2.886751345948125991, -5.000000000000000000 ) ) ;
#70178 = CARTESIAN_POINT ( 'NONE',  ( 3.999999999999998668, 11.26250000000000107, -32.30940107675850470 ) ) ;
#70179 = CARTESIAN_POINT ( 'NONE',  ( 3.862478830110306571, -3.175243778317320409, -4.133272023037573462 ) ) ;
#70180 = CARTESIAN_POINT ( 'NONE',  ( 27.74062500061451431, -3.027376345333610441, -5.243569643749999898 ) ) ;
#70181 = CARTESIAN_POINT ( 'NONE',  ( 8.465625000614515727, 3.027376345333613106, -5.243569643749998122 ) ) ;
#70182 = CARTESIAN_POINT ( 'NONE',  ( 20.92500000122903714, 2.886751345948129099, -4.999999999999998224 ) ) ;
#70183 = CARTESIAN_POINT ( 'NONE',  ( 23.91562500061451502, 3.027376345333611329, 5.243569643749999010 ) ) ;
#70184 = CARTESIAN_POINT ( 'NONE',  ( 26.47499999999999787, -4.330127018922194537, 2.499999999999995559 ) ) ;
#70185 = CARTESIAN_POINT ( 'NONE',  ( 28.60312500061451502, -4.541064518000417216, -2.621784821875001281 ) ) ;
#70186 = CARTESIAN_POINT ( 'NONE',  ( 7.378125000614518036, -4.541064518000419881, 2.621784821874995952 ) ) ;
#70187 = ORIENTED_EDGE ( 'NONE', *, *, #16958, .T. ) ;
#70188 = ADVANCED_FACE ( 'NONE', ( #50064 ), #61860, .T. ) ;
#70189 = CARTESIAN_POINT ( 'NONE',  ( 26.09062500061451573, 6.054752690667223547, 3.707466751127219781E-16 ) ) ;
#70190 = CARTESIAN_POINT ( 'NONE',  ( 5.540625000614515905, -3.027376345333614438, 5.243569643749998122 ) ) ;
#70191 = CARTESIAN_POINT ( 'NONE',  ( 14.78437500061451715, 5.824947211148865298E-16, -4.756430356249998326 ) ) ;
#70192 = CARTESIAN_POINT ( 'NONE',  ( 13.01249999999999929, -5.773502691896255534, -1.060575238724906372E-15 ) ) ;
#70193 = VECTOR ( 'NONE', #26813, 1000.000000000000000 ) ;
#70194 = CARTESIAN_POINT ( 'NONE',  ( 12.11250000000000249, -5.773502691896255534, -1.060575238724906372E-15 ) ) ;
#70196 = CARTESIAN_POINT ( 'NONE',  ( 13.02187500061451608, 3.027376345333613106, -5.243569643749998122 ) ) ;
#70195 = AXIS2_PLACEMENT_3D ( 'NONE', #10723, #50615, #33255 ) ;
#70197 = CARTESIAN_POINT ( 'NONE',  ( 9.862500001229033586, 0.000000000000000000, 4.999999999999998224 ) ) ;
#70198 = CARTESIAN_POINT ( 'NONE',  ( 17.03437500061451715, 6.421520780324663323E-16, -5.243569643749999010 ) ) ;
#70199 = CARTESIAN_POINT ( 'NONE',  ( 15.52500000000000036, 4.330127018922191873, 2.499999999999999556 ) ) ;
#70200 = CARTESIAN_POINT ( 'NONE',  ( 8.709375000614517859, 0.000000000000000000, 5.243569643749999010 ) ) ;
#70201 = CARTESIAN_POINT ( 'NONE',  ( 2.121784821874999061, 12.45312500061451821, -33.67503911421598417 ) ) ;
#70202 = AXIS2_PLACEMENT_3D ( 'NONE', #62382, #46488, #51668 ) ;
#70203 = CARTESIAN_POINT ( 'NONE',  ( 30.00000000000000000, 6.123233995736764310E-16, -4.999999999999998224 ) ) ;
#70204 = CARTESIAN_POINT ( 'NONE',  ( 22.02187500061451431, 4.119189519843966529, 2.378215178124999607 ) ) ;
#70205 = DIRECTION ( 'NONE',  ( 0.000000000000000000, 0.000000000000000000, 1.000000000000000000 ) ) ;
#70206 = CARTESIAN_POINT ( 'NONE',  ( 24.10312500061451502, -4.541064518000417216, -2.621784821875001281 ) ) ;
#70207 = CARTESIAN_POINT ( 'NONE',  ( -4.243569643749999898, 11.27187500061451786, 27.54997392385601529 ) ) ;
#70208 = CARTESIAN_POINT ( 'NONE',  ( 1.626862140677534273E-15, 17.52500000122903145, 34.00000000000000000 ) ) ;
#70209 = CARTESIAN_POINT ( 'NONE',  ( 25.73437500061451644, 4.541064518000418104, 2.621784821874999949 ) ) ;
#70210 = CARTESIAN_POINT ( 'NONE',  ( 29.14687500061451075, -3.027376345333610441, -5.243569643749999898 ) ) ;
#70211 =( BOUNDED_CURVE ( )  B_SPLINE_CURVE ( 2, ( #48430, #64307, #41425, #53594, #8528, #42149, #63941 ),
 .UNSPECIFIED., .F., .F. ) 
 B_SPLINE_CURVE_WITH_KNOTS ( ( 3, 2, 2, 3 ),
 ( 0.8699999999999999956, 0.8733333333333332948, 0.8766666666666667052, 0.8800000000000000044 ),
 .UNSPECIFIED. ) 
 CURVE ( )  GEOMETRIC_REPRESENTATION_ITEM ( )  RATIONAL_B_SPLINE_CURVE ( ( 1.000000000000000000, 0.8660254037844387076, 1.000000000000000000, 0.8660254037844387076, 1.000000000000000000, 0.8660254037844387076, 1.000000000000000000 ) ) 
 REPRESENTATION_ITEM ( '' )  );
#70212 = CARTESIAN_POINT ( 'NONE',  ( 4.228125000614517681, -4.541064518000419881, 2.621784821874995952 ) ) ;
#70213 = CARTESIAN_POINT ( 'NONE',  ( 21.64687500061451431, 0.000000000000000000, 4.756430356249998326 ) ) ;
#70214 = CARTESIAN_POINT ( 'NONE',  ( 16.69687500061451502, 6.054752690667223547, 3.707466751127219781E-16 ) ) ;
#70215 = CARTESIAN_POINT ( 'NONE',  ( 9.534375000614517148, -2.746126346562646425, 4.756430356249996549 ) ) ;
#70216 = CARTESIAN_POINT ( 'NONE',  ( 28.98750000122903359, 6.123233995736764310E-16, -4.999999999999998224 ) ) ;
#70217 = CARTESIAN_POINT ( 'NONE',  ( 9.421875000614519990, 3.027376345333613106, -5.243569643749998122 ) ) ;
#70218 = CARTESIAN_POINT ( 'NONE',  ( 15.72187500061451892, 3.027376345333613106, -5.243569643749998122 ) ) ;
#70219 = CARTESIAN_POINT ( 'NONE',  ( -1.042164773807799261, 25.50793453900451979, 26.12922642428445741 ) ) ;
#70220 = CARTESIAN_POINT ( 'NONE',  ( 25.72499999999999787, 6.123233995736764310E-16, -4.999999999999998224 ) ) ;
#70221 = CARTESIAN_POINT ( 'NONE',  ( 27.64687500061452141, -3.027376345333614438, 5.243569643749998122 ) ) ;
#70222 = CARTESIAN_POINT ( 'NONE',  ( -3.756430356250000102, 14.77812499938548463, 30.00000000000000000 ) ) ;
#70223 = CARTESIAN_POINT ( 'NONE',  ( -2.556497649636125342E-15, 19.21250000000000213, -26.00000000000000355 ) ) ;
#70224 = ORIENTED_EDGE ( 'NONE', *, *, #34645, .T. ) ;
#70225 = CARTESIAN_POINT ( 'NONE',  ( 8.287499999999999645, 5.773502691896255534, 3.535250795749688894E-16 ) ) ;
#70226 = CARTESIAN_POINT ( 'NONE',  ( 8.409375000614517148, 2.746126346562645981, -4.756430356249997438 ) ) ;
#70227 = CARTESIAN_POINT ( 'NONE',  ( 22.71562500061451573, -6.054752690667223547, -1.112240025338166033E-15 ) ) ;
#70228 = CARTESIAN_POINT ( 'NONE',  ( 12.37500000000000000, 4.330127018922191873, 2.499999999999999556 ) ) ;
#70229 = CARTESIAN_POINT ( 'NONE',  ( 7.875000001229034652, 2.886751345948129099, -4.999999999999998224 ) ) ;
#70230 = CARTESIAN_POINT ( 'NONE',  ( 7.678125000614516082, 4.541064518000418104, 2.621784821874999949 ) ) ;
#70231 = CARTESIAN_POINT ( 'NONE',  ( 21.48750000000000071, -2.886751345948129988, 4.999999999999997335 ) ) ;
#70232 = EDGE_CURVE ( 'NONE', #5506, #20508, #30670, .T. ) ;
#70233 = CARTESIAN_POINT ( 'NONE',  ( 18.44062500061451715, 6.054752690667223547, 3.707466751127219781E-16 ) ) ;
#70234 = CARTESIAN_POINT ( 'NONE',  ( 4.148274082013050368, -2.791383553096713044, 4.344604658505033079 ) ) ;
#70235 = CARTESIAN_POINT ( 'NONE',  ( 26.66250000122903430, -4.330127018922190985, -2.500000000000001332 ) ) ;
#70236 = CARTESIAN_POINT ( 'NONE',  ( 3.756430356250000546, 18.97812499938548214, 27.83122392262697886 ) ) ;
#70237 = CARTESIAN_POINT ( 'NONE',  ( 4.612500000000002487, 2.886751345948129099, -4.999999999999998224 ) ) ;
#70238 = ADVANCED_FACE ( 'NONE', ( #10535 ), #4639, .T. ) ;
#70239 = AXIS2_PLACEMENT_3D ( 'NONE', #6563, #50183, #72711 ) ;
#70240 = ORIENTED_EDGE ( 'NONE', *, *, #35309, .F. ) ;
#70241 = CARTESIAN_POINT ( 'NONE',  ( 19.34062500061451573, 6.054752690667223547, 3.707466751127219781E-16 ) ) ;
#70242 = CARTESIAN_POINT ( 'NONE',  ( 25.64062500061451644, 6.054752690667223547, 3.707466751127219781E-16 ) ) ;
#70243 = CARTESIAN_POINT ( 'NONE',  ( 26.89687500061451431, -3.027376345333610441, -5.243569643749999898 ) ) ;
#70244 = CARTESIAN_POINT ( 'NONE',  ( 9.937500000000001776, -2.886751345948125991, -5.000000000000000000 ) ) ;
#70245 = CARTESIAN_POINT ( 'NONE',  ( 12.10312500061451857, 4.541064518000418104, -2.621784821874998173 ) ) ;
#70246 = CARTESIAN_POINT ( 'NONE',  ( 29.05312500061451431, -4.541064518000417216, -2.621784821875001281 ) ) ;
#70247 = CARTESIAN_POINT ( 'NONE',  ( 8.578125000614518214, 4.541064518000418104, 2.621784821874999949 ) ) ;
#70248 = CARTESIAN_POINT ( 'NONE',  ( 14.11875000122903323, 2.886751345948073588, -5.000000000000094147 ) ) ;
#70249 = CARTESIAN_POINT ( 'NONE',  ( -4.243569643749999898, 13.10937500061451821, 30.00000000000000000 ) ) ;
#70250 = CARTESIAN_POINT ( 'NONE',  ( 26.96250000122903145, 0.000000000000000000, 4.999999999999998224 ) ) ;
#70251 = CARTESIAN_POINT ( 'NONE',  ( 20.22187500061451715, 2.746126346562645981, -4.756430356249997438 ) ) ;
#70252 = CARTESIAN_POINT ( 'NONE',  ( 13.60312500061451679, 0.000000000000000000, 5.243569643749999010 ) ) ;
#70253 = CARTESIAN_POINT ( 'NONE',  ( 9.834375000614517859, 6.421520780324663323E-16, -5.243569643749999010 ) ) ;
#70254 = CARTESIAN_POINT ( 'NONE',  ( 10.09687500061451715, -3.027376345333614438, 5.243569643749998122 ) ) ;
#70256 = EDGE_CURVE ( 'NONE', #72227, #755, #10837, .T. ) ;
#70255 = CARTESIAN_POINT ( 'NONE',  ( 17.74687500061451928, -3.027376345333614438, 5.243569643749998122 ) ) ;
#70257 = ORIENTED_EDGE ( 'NONE', *, *, #35738, .F. ) ;
#70258 = CARTESIAN_POINT ( 'NONE',  ( 29.33437500061451431, 4.541064518000418104, 2.621784821874999949 ) ) ;
#70259 = CARTESIAN_POINT ( 'NONE',  ( 22.37812500061451360, 6.421520780324663323E-16, -5.243569643749999010 ) ) ;
#70260 = AXIS2_PLACEMENT_3D ( 'NONE', #20066, #42622, #65146 ) ;
#70261 = CARTESIAN_POINT ( 'NONE',  ( 16.69687500061451502, 6.054752690667223547, 3.707466751127219781E-16 ) ) ;
#70262 = CARTESIAN_POINT ( 'NONE',  ( 21.25312500061451715, 0.000000000000000000, 5.243569643749999010 ) ) ;
#70263 = CARTESIAN_POINT ( 'NONE',  ( -1.999999999999997113, 13.77500000000000036, 33.46410161513775705 ) ) ;
#70264 = CARTESIAN_POINT ( 'NONE',  ( 27.06562500061451004, 3.027376345333611329, 5.243569643749999010 ) ) ;
#70265 = CARTESIAN_POINT ( 'NONE',  ( 6.975000001229032520, 2.886751345948129099, -4.999999999999998224 ) ) ;
#70266 = ORIENTED_EDGE ( 'NONE', *, *, #29620, .T. ) ;
#70267 = CARTESIAN_POINT ( 'NONE',  ( 3.525000001229034119, 2.886751345948126879, 4.999999999999999112 ) ) ;
#70268 = CARTESIAN_POINT ( 'NONE',  ( 4.000000000000000000, 17.93750000000000355, -27.69059892324149530 ) ) ;
#70269 = CARTESIAN_POINT ( 'NONE',  ( 24.75000000122902932, -2.886751345948129988, 4.999999999999997335 ) ) ;
#70270 = CARTESIAN_POINT ( 'NONE',  ( -2.000000000000001776, 20.39374999877096428, 33.46410161513775705 ) ) ;
#70271 = ADVANCED_FACE ( 'NONE', ( #5721 ), #16425, .F. ) ;
#70272 = CARTESIAN_POINT ( 'NONE',  ( 7.959375000614516971, -4.541064518000417216, -2.621784821875001281 ) ) ;
#70273 = CARTESIAN_POINT ( 'NONE',  ( 23.28750000000000142, -2.886751345948130876, 4.999999999999996447 ) ) ;
#70274 = CARTESIAN_POINT ( 'NONE',  ( 15.14062500061451644, -3.027376345333610441, -5.243569643749999898 ) ) ;
#70275 = CARTESIAN_POINT ( 'NONE',  ( 8.184375000614515727, 4.541064518000418104, 2.621784821874999949 ) ) ;
#70276 = CARTESIAN_POINT ( 'NONE',  ( 27.52500000122903145, -5.773502691896255534, -1.060575238724906372E-15 ) ) ;
#70277 = CARTESIAN_POINT ( 'NONE',  ( 16.77187500061451786, 3.027376345333611329, 5.243569643749999010 ) ) ;
#70278 = CARTESIAN_POINT ( 'NONE',  ( 5.146875000614517859, -3.027376345333614438, 5.243569643749998122 ) ) ;
#70279 = CARTESIAN_POINT ( 'NONE',  ( 1.071796769724500997, 18.70759618943233349, 33.99999999999999289 ) ) ;
#70280 = CARTESIAN_POINT ( 'NONE',  ( 4.528125000614516615, 4.541064518000418104, 2.621784821874999949 ) ) ;
#70281 = CARTESIAN_POINT ( 'NONE',  ( 16.64062500061451289, 6.054752690667223547, 3.707466751127219781E-16 ) ) ;
#70282 = ORIENTED_EDGE ( 'NONE', *, *, #71109, .T. ) ;
#70283 = CARTESIAN_POINT ( 'NONE',  ( 13.67812500061451786, -4.541064518000419881, 2.621784821874995952 ) ) ;
#70284 = CARTESIAN_POINT ( 'NONE',  ( 4.950000001229033941, -2.886751345948129988, 4.999999999999997335 ) ) ;
#70285 = CARTESIAN_POINT ( 'NONE',  ( 11.31562500061451892, 3.027376345333611329, 5.243569643749999010 ) ) ;
#70286 = CARTESIAN_POINT ( 'NONE',  ( 21.60937500061451644, 4.119189519843966529, -2.378215178124998275 ) ) ;
#70287 = CARTESIAN_POINT ( 'NONE',  ( 10.12500000000000178, 4.330127018922191873, 2.499999999999999556 ) ) ;
#70288 = CARTESIAN_POINT ( 'NONE',  ( 7.537500001229033408, 4.330127018922191873, 2.499999999999999556 ) ) ;
#70289 = CARTESIAN_POINT ( 'NONE',  ( 21.26249999999999574, 2.886751345948129099, -4.999999999999998224 ) ) ;
#70290 = EDGE_CURVE ( 'NONE', #17018, #38031, #10935, .T. ) ;
#70291 = CARTESIAN_POINT ( 'NONE',  ( 16.05937500061451573, -4.541064518000417216, -2.621784821875001281 ) ) ;
#70292 = CARTESIAN_POINT ( 'NONE',  ( 15.71250000122903501, 0.000000000000000000, 4.999999999999998224 ) ) ;
#70293 = CARTESIAN_POINT ( 'NONE',  ( 23.40000000000000213, -4.330127018922190985, -2.500000000000001332 ) ) ;
#70294 = AXIS2_PLACEMENT_3D ( 'NONE', #41471, #17824, #34834 ) ;
#70295 = CARTESIAN_POINT ( 'NONE',  ( 4.243569643749999898, 19.54062500061451857, -27.54997392385601529 ) ) ;
#70296 = CARTESIAN_POINT ( 'NONE',  ( 9.150000000000002132, 4.330127018922192761, -2.499999999999997780 ) ) ;
#70297 = CARTESIAN_POINT ( 'NONE',  ( -1.243387493232115393E-14, 15.31250000000000000, 26.00000000000000000 ) ) ;
#70298 = CARTESIAN_POINT ( 'NONE',  ( 3.486133158594716510E-16, 19.88749999999999929, 26.00000000000000355 ) ) ;
#70299 = CARTESIAN_POINT ( 'NONE',  ( 1.626862140677534273E-15, 10.32500000122903572, -26.00000000000000355 ) ) ;
#70300 = CARTESIAN_POINT ( 'NONE',  ( 16.88437500061451502, -4.541064518000419881, 2.621784821874995952 ) ) ;
#70301 = CARTESIAN_POINT ( 'NONE',  ( 28.12499999999999645, 4.330127018922191873, 2.499999999999999556 ) ) ;
#70302 = CARTESIAN_POINT ( 'NONE',  ( 11.57812500061451644, 6.421520780324663323E-16, -5.243569643749999010 ) ) ;
#70303 = CARTESIAN_POINT ( 'NONE',  ( 8.156250001229034652, -4.330127018922190985, -2.500000000000001332 ) ) ;
#70304 = CARTESIAN_POINT ( 'NONE',  ( 23.48437500061451644, 4.541064518000418104, 2.621784821874999949 ) ) ;
#70305 = CARTESIAN_POINT ( 'NONE',  ( 16.35937500061451644, -5.492252693125287522, -1.008910452111647106E-15 ) ) ;
#70306 = CARTESIAN_POINT ( 'NONE',  ( 9.290625000614515017, -3.027376345333610441, -5.243569643749999898 ) ) ;
#70307 = CARTESIAN_POINT ( 'NONE',  ( 15.45937500061451608, 0.000000000000000000, 5.243569643749999010 ) ) ;
#70308 = VERTEX_POINT ( 'NONE', #28612 ) ;
#70309 = CARTESIAN_POINT ( 'NONE',  ( 27.04687500061451644, 6.054752690667223547, 3.707466751127219781E-16 ) ) ;
#70310 = CARTESIAN_POINT ( 'NONE',  ( 27.10312500061451502, 0.000000000000000000, 5.243569643749999010 ) ) ;
#70311 = CARTESIAN_POINT ( 'NONE',  ( 28.82812500061451644, 4.541064518000418104, 2.621784821874999949 ) ) ;
#70312 = CARTESIAN_POINT ( 'NONE',  ( 1.999999999999998668, 12.76250000122903394, -33.46410161513775705 ) ) ;
#70313 = CARTESIAN_POINT ( 'NONE',  ( 6.562500000000001776, 2.886751345948126879, 4.999999999999999112 ) ) ;
#70314 = CARTESIAN_POINT ( 'NONE',  ( 20.40000000122903145, -2.886751345948125991, -5.000000000000000000 ) ) ;
#70315 = CARTESIAN_POINT ( 'NONE',  ( 7.359375000614517326, -5.492252693125287522, -1.008910452111647106E-15 ) ) ;
#70316 = ORIENTED_EDGE ( 'NONE', *, *, #68178, .T. ) ;
#70317 = CARTESIAN_POINT ( 'NONE',  ( 16.31250000000000000, 2.886751345948129099, -4.999999999999998224 ) ) ;
#70318 = CARTESIAN_POINT ( 'NONE',  ( 19.50000000000000000, 4.330127018922192761, -2.499999999999997780 ) ) ;
#70319 = CARTESIAN_POINT ( 'NONE',  ( 14.42812500061451786, 4.541064518000418104, 2.621784821874999949 ) ) ;
#70320 = ORIENTED_EDGE ( 'NONE', *, *, #72450, .T. ) ;
#70321 = CARTESIAN_POINT ( 'NONE',  ( 2.121784821875001281, 15.95937500061451608, -26.32496088578401938 ) ) ;
#70322 = CARTESIAN_POINT ( 'NONE',  ( 6.365625000614518747, 3.027376345333611329, 5.243569643749999010 ) ) ;
#70323 = CARTESIAN_POINT ( 'NONE',  ( -7.967954043666661671E-16, 12.97812499938548392, 34.33755215474603517 ) ) ;
#70324 = CARTESIAN_POINT ( 'NONE',  ( 11.32500000000000107, 6.123233995736764310E-16, -4.999999999999998224 ) ) ;
#70325 = CARTESIAN_POINT ( 'NONE',  ( 29.18437500061451217, 5.492252693125287522, 3.363034840372157021E-16 ) ) ;
#70326 = EDGE_LOOP ( 'NONE', ( #68995, #39942, #51005, #39734 ) ) ;
#70327 = CARTESIAN_POINT ( 'NONE',  ( -4.243569643749997233, 16.24062500061451431, 32.45002607614398471 ) ) ;
#70328 = CARTESIAN_POINT ( 'NONE',  ( 25.71562500061451573, 3.027376345333611329, 5.243569643749999010 ) ) ;
#70329 = CARTESIAN_POINT ( 'NONE',  ( 7.575000000000001954, -4.330127018922194537, 2.499999999999995559 ) ) ;
#70330 = CARTESIAN_POINT ( 'NONE',  ( 3.756430356250000546, 18.07812499938548711, 27.83122392262697886 ) ) ;
#70331 = CARTESIAN_POINT ( 'NONE',  ( 24.49687500061451573, -3.027376345333614438, 5.243569643749998122 ) ) ;
#70332 = CARTESIAN_POINT ( 'NONE',  ( 21.36562500061451431, -6.054752690667223547, -1.112240025338166033E-15 ) ) ;
#70333 = CARTESIAN_POINT ( 'NONE',  ( 4.243569643749999898, 15.04062500061459495, -27.54997392385601529 ) ) ;
#70334 = CARTESIAN_POINT ( 'NONE',  ( 24.18750000122903288, 4.330127018922191873, 2.499999999999999556 ) ) ;
#70335 = CARTESIAN_POINT ( 'NONE',  ( 6.103125000614515905, -4.541064518000417216, -2.621784821875001281 ) ) ;
#70336 = CARTESIAN_POINT ( 'NONE',  ( 25.62187500061451928, 2.746126346562645981, -4.756430356249997438 ) ) ;
#70337 = CARTESIAN_POINT ( 'NONE',  ( 24.36562500061451786, 3.027376345333611329, 5.243569643749999010 ) ) ;
#70338 = CARTESIAN_POINT ( 'NONE',  ( 11.44687500061451857, -2.746126346562646425, 4.756430356249996549 ) ) ;
#70339 = CARTESIAN_POINT ( 'NONE',  ( 3.756430356250000546, 15.37812499938548427, 27.83122392262697886 ) ) ;
#70340 = EDGE_CURVE ( 'NONE', #55366, #26340, #23126, .T. ) ;
#70341 = CARTESIAN_POINT ( 'NONE',  ( 16.99687500061451573, -3.027376345333610441, -5.243569643749999898 ) ) ;
#70342 = CARTESIAN_POINT ( 'NONE',  ( 25.84687500061451360, -3.027376345333614438, 5.243569643749998122 ) ) ;
#70343 = CARTESIAN_POINT ( 'NONE',  ( 4.243569643749999898, 14.23437500061451821, 30.00000000000000000 ) ) ;
#70344 = CARTESIAN_POINT ( 'NONE',  ( 5.915625000614515905, 3.027376345333611329, 5.243569643749999010 ) ) ;
#70345 = CARTESIAN_POINT ( 'NONE',  ( 29.69062500061451715, 6.054752690667223547, 3.707466751127219781E-16 ) ) ;
#70346 = CARTESIAN_POINT ( 'NONE',  ( 29.39062500061451289, -3.027376345333614438, 5.243569643749998122 ) ) ;
#70347 = CYLINDRICAL_SURFACE ( 'NONE', #39574, 4.999999999999998224 ) ;
#70348 = CARTESIAN_POINT ( 'NONE',  ( 3.203127373816005541, 9.474626018533117033, -35.07709628816699166 ) ) ;
#70349 = AXIS2_PLACEMENT_3D ( 'NONE', #69816, #1505, #34735 ) ;
#70350 = CARTESIAN_POINT ( 'NONE',  ( 29.47500000122903430, 2.886751345948129099, -4.999999999999998224 ) ) ;
#70351 = CARTESIAN_POINT ( 'NONE',  ( 8.371875000614515727, -6.054752690667223547, -1.112240025338166033E-15 ) ) ;
#70352 = CARTESIAN_POINT ( 'NONE',  ( 16.23750000122903359, -4.330127018922194537, 2.499999999999995559 ) ) ;
#70353 = CARTESIAN_POINT ( 'NONE',  ( 3.346875000614518036, -3.027376345333614438, 5.243569643749998122 ) ) ;
#70354 = CARTESIAN_POINT ( 'NONE',  ( 11.47500000122903252, 2.886751345948129099, -4.999999999999998224 ) ) ;
#70355 = CARTESIAN_POINT ( 'NONE',  ( 4.153125000614515727, 0.000000000000000000, 5.243569643749999010 ) ) ;
#70356 = CARTESIAN_POINT ( 'NONE',  ( -1.999999999999999112, 13.49374999877096570, 26.53589838486224650 ) ) ;
#70357 = CARTESIAN_POINT ( 'NONE',  ( 20.53125000122903288, 4.330127018922191873, 2.499999999999999556 ) ) ;
#70358 = CARTESIAN_POINT ( 'NONE',  ( 14.29687500061451821, -3.027376345333610441, -5.243569643749999898 ) ) ;
#70359 = CARTESIAN_POINT ( 'NONE',  ( 11.84999999999999964, 4.330127018922192761, -2.499999999999997780 ) ) ;
#70360 = ORIENTED_EDGE ( 'NONE', *, *, #29725, .F. ) ;
#70361 = CARTESIAN_POINT ( 'NONE',  ( 22.97812500061451857, 4.541064518000418104, 2.621784821874999949 ) ) ;
#70362 = CARTESIAN_POINT ( 'NONE',  ( 7.640625000614517326, 6.054752690667223547, 3.707466751127219781E-16 ) ) ;
#70363 = CARTESIAN_POINT ( 'NONE',  ( 24.90937500061451715, 0.000000000000000000, 5.243569643749999010 ) ) ;
#70364 = CARTESIAN_POINT ( 'NONE',  ( 6.965625000614518392, -6.054752690667223547, -1.112240025338166033E-15 ) ) ;
#70365 = CARTESIAN_POINT ( 'NONE',  ( 3.405214727565324839, 4.049716704864715133, -2.985684910913894097 ) ) ;
#70366 = CARTESIAN_POINT ( 'NONE',  ( 11.32500000122903394, -5.773502691896255534, -1.060575238724906372E-15 ) ) ;
#70367 = CARTESIAN_POINT ( 'NONE',  ( 24.21562500061451573, 3.027376345333613106, -5.243569643749998122 ) ) ;
#70368 = CARTESIAN_POINT ( 'NONE',  ( -4.243569643749997233, 11.74062500061451786, -27.54997392385601174 ) ) ;
#70369 = CARTESIAN_POINT ( 'NONE',  ( 10.53750000122903252, 6.123233995736764310E-16, -4.999999999999998224 ) ) ;
#70370 = CARTESIAN_POINT ( 'NONE',  ( 19.97812500061451502, -4.541064518000419881, 2.621784821874995952 ) ) ;
#70371 = CARTESIAN_POINT ( 'NONE',  ( 17.69062500061451715, -3.027376345333614438, 5.243569643749998122 ) ) ;
#70372 = CARTESIAN_POINT ( 'NONE',  ( 27.60937500061451644, 0.000000000000000000, 4.756430356249998326 ) ) ;
#70373 = CARTESIAN_POINT ( 'NONE',  ( 17.81250000000000355, 2.886751345948126879, 4.999999999999999112 ) ) ;
#70374 = CARTESIAN_POINT ( 'NONE',  ( 13.91250000122903252, 0.000000000000000000, 4.999999999999998224 ) ) ;
#70375 = EDGE_CURVE ( 'NONE', #3193, #1870, #10415, .T. ) ;
#70376 = CARTESIAN_POINT ( 'NONE',  ( 10.82812500061451644, 4.541064518000418104, 2.621784821874999949 ) ) ;
#70377 = CARTESIAN_POINT ( 'NONE',  ( 14.20312500061451644, -4.541064518000417216, -2.621784821875001281 ) ) ;
#70378 = CARTESIAN_POINT ( 'NONE',  ( 24.07500000122903216, 2.886751345948129099, -4.999999999999998224 ) ) ;
#70379 = CARTESIAN_POINT ( 'NONE',  ( 21.34687500061451715, -3.027376345333614438, 5.243569643749998122 ) ) ;
#70380 = CARTESIAN_POINT ( 'NONE',  ( 21.19687500061451502, 6.054752690667223547, 3.707466751127219781E-16 ) ) ;
#70381 = CARTESIAN_POINT ( 'NONE',  ( 50.00000000000000000, 8.875000000000000000, 1.494782592887675232 ) ) ;
#70382 = AXIS2_PLACEMENT_3D ( 'NONE', #10823, #15623, #38165 ) ;
#70383 = EDGE_CURVE ( 'NONE', #42390, #10555, #24510, .T. ) ;
#70384 = CARTESIAN_POINT ( 'NONE',  ( 8.512500001229033941, 0.000000000000000000, 4.999999999999998224 ) ) ;
#70385 = CARTESIAN_POINT ( 'NONE',  ( 5.371875000614516615, 3.027376345333613106, -5.243569643749998122 ) ) ;
#70386 = CARTESIAN_POINT ( 'NONE',  ( 24.08437500061451786, -4.541064518000419881, 2.621784821874995952 ) ) ;
#70387 = CARTESIAN_POINT ( 'NONE',  ( 26.55000000122903359, -2.886751345948121994, 5.000000000000011546 ) ) ;
#70388 = CARTESIAN_POINT ( 'NONE',  ( 19.11562500061451431, -6.054752690667223547, -1.112240025338166033E-15 ) ) ;
#70389 = CARTESIAN_POINT ( 'NONE',  ( 25.09687500061451715, -3.027376345333610441, -5.243569643749999898 ) ) ;
#70390 = CARTESIAN_POINT ( 'NONE',  ( -3.756430356249999214, 19.24062499938548143, 27.83122392262697176 ) ) ;
#70391 = CARTESIAN_POINT ( 'NONE',  ( -1.999999999999997113, 11.18750000122903288, -26.53589838486224295 ) ) ;
#70392 = CARTESIAN_POINT ( 'NONE',  ( 11.04375000122903216, 5.773502691896255534, 3.535250795749688401E-16 ) ) ;
#70393 = CARTESIAN_POINT ( 'NONE',  ( 4.734375000614518214, -4.541064518000419881, 2.621784821874995952 ) ) ;
#70394 = CARTESIAN_POINT ( 'NONE',  ( 16.37812500061451715, -4.541064518000419881, 2.621784821874995952 ) ) ;
#70395 = ORIENTED_EDGE ( 'NONE', *, *, #21542, .T. ) ;
#70396 = CARTESIAN_POINT ( 'NONE',  ( -1.071796769724491005, 12.70759618943233349, -34.00000000000000000 ) ) ;
#70397 = CARTESIAN_POINT ( 'NONE',  ( 24.77812500061451217, 4.541064518000418104, 2.621784821874999949 ) ) ;
#70398 = DIRECTION ( 'NONE',  ( 0.000000000000000000, 0.000000000000000000, -1.000000000000000000 ) ) ;
#70399 = CARTESIAN_POINT ( 'NONE',  ( 28.12499999999999645, 4.330127018922191873, 2.499999999999999556 ) ) ;
#70400 = DIRECTION ( 'NONE',  ( -1.000000000000000000, -0.000000000000000000, -0.000000000000000000 ) ) ;
#70401 = CARTESIAN_POINT ( 'NONE',  ( 14.40000000000000036, -4.330127018922190985, -2.500000000000001332 ) ) ;
#70402 = CARTESIAN_POINT ( 'NONE',  ( 26.17500000122903359, -5.773502691896255534, -1.060575238724906372E-15 ) ) ;
#70403 = CARTESIAN_POINT ( 'NONE',  ( 20.72812500061451502, 4.541064518000418104, 2.621784821874999949 ) ) ;
#70404 = EDGE_CURVE ( 'NONE', #66841, #53581, #52897, .T. ) ;
#70405 = ORIENTED_EDGE ( 'NONE', *, *, #54179, .T. ) ;
#70406 = CARTESIAN_POINT ( 'NONE',  ( 23.32499999999999929, -4.330127018922194537, 2.499999999999995559 ) ) ;
#70407 = CARTESIAN_POINT ( 'NONE',  ( 23.29687500061451644, -3.027376345333610441, -5.243569643749999898 ) ) ;
#70408 = ORIENTED_EDGE ( 'NONE', *, *, #71580, .T. ) ;
#70409 = CARTESIAN_POINT ( 'NONE',  ( 25.76249999999999218, 2.886751345948087355, -5.000000000000071054 ) ) ;
#70410 = CARTESIAN_POINT ( 'NONE',  ( 12.47812500061451502, 6.421520780324663323E-16, -5.243569643749999010 ) ) ;
#70411 = CARTESIAN_POINT ( 'NONE',  ( 3.703125000614516882, 0.000000000000000000, 5.243569643749999010 ) ) ;
#70412 = CARTESIAN_POINT ( 'NONE',  ( 15.94687500061451502, -4.119189519843965641, -2.378215178125001383 ) ) ;
#70413 = CARTESIAN_POINT ( 'NONE',  ( 28.22812500061451502, 6.421520780324663323E-16, -5.243569643749999010 ) ) ;
#70414 = CARTESIAN_POINT ( 'NONE',  ( 13.16250000122903430, -4.330127018922190985, -2.500000000000001332 ) ) ;
#70415 = CARTESIAN_POINT ( 'NONE',  ( 18.56250000000000000, 2.886751345948129099, -4.999999999999998224 ) ) ;
#70416 = CARTESIAN_POINT ( 'NONE',  ( 27.18750000000000000, 5.773502691896255534, 3.535250795749688894E-16 ) ) ;
#70417 = CARTESIAN_POINT ( 'NONE',  ( 1.071796769724491227, 14.33615380933862937, 26.00000000000000000 ) ) ;
#70418 = CARTESIAN_POINT ( 'NONE',  ( 6.834375000614518747, 4.541064518000418104, 2.621784821874999949 ) ) ;
#70419 = CARTESIAN_POINT ( 'NONE',  ( 20.40937500061451715, 0.000000000000000000, 5.243569643749999010 ) ) ;
#70420 = CARTESIAN_POINT ( 'NONE',  ( 28.87499999999999645, 6.123233995736764310E-16, -4.999999999999998224 ) ) ;
#70421 = ORIENTED_EDGE ( 'NONE', *, *, #12871, .F. ) ;
#70422 = CARTESIAN_POINT ( 'NONE',  ( 27.59062500061451573, -3.027376345333614438, 5.243569643749998122 ) ) ;
#70423 = CARTESIAN_POINT ( 'NONE',  ( 28.99687500061451573, -3.027376345333614438, 5.243569643749998122 ) ) ;
#70424 = CARTESIAN_POINT ( 'NONE',  ( 4.959375000614516971, 4.541064518000418104, -2.621784821874998173 ) ) ;
#70425 = CARTESIAN_POINT ( 'NONE',  ( 16.16250000000000142, -5.773502691896255534, -1.060575238724906372E-15 ) ) ;
#70426 = CARTESIAN_POINT ( 'NONE',  ( 13.26562500061451644, -6.054752690667223547, -1.112240025338166033E-15 ) ) ;
#70427 = CARTESIAN_POINT ( 'NONE',  ( 15.20625000122903181, 0.000000000000000000, 4.999999999999998224 ) ) ;
#70428 = CARTESIAN_POINT ( 'NONE',  ( 45.00000000000000000, 8.874999999999998224, 1.494782592887687667 ) ) ;
#70429 = CARTESIAN_POINT ( 'NONE',  ( 0.000000000000000000, 20.00000000000000000, -30.00000000000000000 ) ) ;
#70430 = CARTESIAN_POINT ( 'NONE',  ( 17.36250000122903359, 4.330127018922192761, -2.499999999999997780 ) ) ;
#70431 = CARTESIAN_POINT ( 'NONE',  ( -5.810221930991193690E-16, 10.55000000122903359, 26.00000000000000355 ) ) ;
#70432 = CARTESIAN_POINT ( 'NONE',  ( 17.85937500061451999, -4.119189519843965641, -2.378215178125001383 ) ) ;
#70433 = CARTESIAN_POINT ( 'NONE',  ( 8.128125000614515372, 4.541064518000418104, 2.621784821874999949 ) ) ;
#70434 = CARTESIAN_POINT ( 'NONE',  ( 23.25937500061451857, -4.541064518000417216, -2.621784821875001281 ) ) ;
#70435 = CARTESIAN_POINT ( 'NONE',  ( 4.243569643749999898, 16.44687500061451857, 32.45002607614398471 ) ) ;
#70436 = CARTESIAN_POINT ( 'NONE',  ( 23.33437500061451786, 6.421520780324663323E-16, -5.243569643749999010 ) ) ;
#70437 = CARTESIAN_POINT ( 'NONE',  ( 6.075000000000000178, 4.330127018922191873, 2.499999999999999556 ) ) ;
#70438 = CARTESIAN_POINT ( 'NONE',  ( 1.999999999999998668, 10.06250000122903465, 26.53589838486224650 ) ) ;
#70439 = CARTESIAN_POINT ( 'NONE',  ( 12.70312500061451821, 0.000000000000000000, 5.243569643749999010 ) ) ;
#70440 = CARTESIAN_POINT ( 'NONE',  ( 3.675000001229035362, -5.773502691896255534, -1.060575238724906372E-15 ) ) ;
#70441 = CARTESIAN_POINT ( 'NONE',  ( 8.559375000614515727, 4.541064518000418104, -2.621784821874998173 ) ) ;
#70442 = CARTESIAN_POINT ( 'NONE',  ( 3.895888853841904531, -3.134084140313734501, 4.010892849215046851 ) ) ;
#70443 = VERTEX_POINT ( 'NONE', #69588 ) ;
#70444 = CARTESIAN_POINT ( 'NONE',  ( 10.52812500061451750, -4.541064518000419881, 2.621784821874995952 ) ) ;
#70445 = CARTESIAN_POINT ( 'NONE',  ( 14.18437500061451750, -4.541064518000419881, 2.621784821874995952 ) ) ;
#70446 = CARTESIAN_POINT ( 'NONE',  ( 29.17500000122903359, 2.886751345948106007, 5.000000000000033751 ) ) ;
#70447 = CARTESIAN_POINT ( 'NONE',  ( 23.62500000122902932, 2.886751345948129099, -4.999999999999998224 ) ) ;
#70448 = CARTESIAN_POINT ( 'NONE',  ( 9.834375000614517859, 6.421520780324663323E-16, -5.243569643749999010 ) ) ;
#70449 = CARTESIAN_POINT ( 'NONE',  ( 12.51562500061451821, 3.027376345333613106, -5.243569643749998122 ) ) ;
#70450 = CARTESIAN_POINT ( 'NONE',  ( 27.46875000122903288, -5.773502691896255534, -1.060575238724906372E-15 ) ) ;
#70451 = CARTESIAN_POINT ( 'NONE',  ( 22.24687500061451217, -3.027376345333614438, 5.243569643749998122 ) ) ;
#70452 = CYLINDRICAL_SURFACE ( 'NONE', #14811, 3.999999999999996447 ) ;
#70453 = CARTESIAN_POINT ( 'NONE',  ( 5.362500000000002487, -5.773502691896255534, -1.060575238724906372E-15 ) ) ;
#70454 = CARTESIAN_POINT ( 'NONE',  ( 8.212500000000000355, 2.886751345948129099, -4.999999999999997335 ) ) ;
#70455 = CARTESIAN_POINT ( 'NONE',  ( -4.243569643749999898, 14.45937500061451964, -30.00000000000000000 ) ) ;
#70456 = CARTESIAN_POINT ( 'NONE',  ( 16.50937500061451502, -4.541064518000417216, -2.621784821875001281 ) ) ;
#70457 = CARTESIAN_POINT ( 'NONE',  ( 16.65000000122903501, -2.886751345948129988, 4.999999999999997335 ) ) ;
#70458 =( BOUNDED_CURVE ( )  B_SPLINE_CURVE ( 2, ( #66826, #16558, #39109, #16916, #27298, #33550, #38750, #56100, #45376 ),
 .UNSPECIFIED., .F., .F. ) 
 B_SPLINE_CURVE_WITH_KNOTS ( ( 3, 2, 2, 2, 3 ),
 ( 0.8750000000000000000, 0.8796296296296296502, 0.8888888888888888395, 0.8981481481481481399, 0.9027777777777777901 ),
 .UNSPECIFIED. ) 
 CURVE ( )  GEOMETRIC_REPRESENTATION_ITEM ( )  RATIONAL_B_SPLINE_CURVE ( ( 0.9330127018922194093, 0.9330127018922194093, 1.000000000000000000, 0.8660254037844387076, 1.000000000000000000, 0.8660254037844387076, 1.000000000000000000, 0.9330127018922194093, 0.9330127018922194093 ) ) 
 REPRESENTATION_ITEM ( '' )  );
#70459 = CARTESIAN_POINT ( 'NONE',  ( 11.29687500061451644, 6.054752690667223547, 3.707466751127219781E-16 ) ) ;
#70460 = CARTESIAN_POINT ( 'NONE',  ( -4.243569643749999898, 18.00312500061451715, -30.00000000000000000 ) ) ;
#70461 = CARTESIAN_POINT ( 'NONE',  ( 16.80000000122903359, -2.886751345948125991, -5.000000000000000000 ) ) ;
#70462 = CARTESIAN_POINT ( 'NONE',  ( 13.26562500061451644, -6.054752690667223547, -1.112240025338166033E-15 ) ) ;
#70463 = EDGE_LOOP ( 'NONE', ( #44395, #41423, #53229, #67626 ) ) ;
#70464 = CARTESIAN_POINT ( 'NONE',  ( 15.56250000000000000, 2.886751345948126879, 4.999999999999999112 ) ) ;
#70465 = DIRECTION ( 'NONE',  ( -1.000000000000000000, -0.000000000000000000, -0.000000000000000000 ) ) ;
#70466 = CARTESIAN_POINT ( 'NONE',  ( 9.721875000614517148, -6.054752690667223547, -1.112240025338166033E-15 ) ) ;
#70467 = CARTESIAN_POINT ( 'NONE',  ( 3.458282317606259149, 3.615826433065254530, 27.97484066355150034 ) ) ;
#70468 = CARTESIAN_POINT ( 'NONE',  ( 11.88750000122903216, 6.123233995736764310E-16, -4.999999999999998224 ) ) ;
#70469 = CARTESIAN_POINT ( 'NONE',  ( 22.16250000122903074, -4.330127018922190985, -2.500000000000001332 ) ) ;
#70470 = CARTESIAN_POINT ( 'NONE',  ( 17.16562500061451502, 3.027376345333611329, 5.243569643749999010 ) ) ;
#70471 = CARTESIAN_POINT ( 'NONE',  ( 21.81562500061451004, -6.054752690667223547, -1.112240025338166033E-15 ) ) ;
#70472 = CARTESIAN_POINT ( 'NONE',  ( 27.22500000122903430, 2.886751345948129099, -4.999999999999998224 ) ) ;
#70473 = CARTESIAN_POINT ( 'NONE',  ( 24.93750000000000355, 5.773502691896255534, 3.535250795749688894E-16 ) ) ;
#70474 = CARTESIAN_POINT ( 'NONE',  ( 17.60625000122903572, -4.330127018922190985, -2.500000000000001332 ) ) ;
#70475 = CARTESIAN_POINT ( 'NONE',  ( 7.621875000614519280, 2.746126346562645981, -4.756430356249997438 ) ) ;
#70476 = CARTESIAN_POINT ( 'NONE',  ( 27.53437500061451360, 4.541064518000418104, 2.621784821874999949 ) ) ;
#70477 = CARTESIAN_POINT ( 'NONE',  ( 26.68125000122903145, 6.123233995736764310E-16, -4.999999999999998224 ) ) ;
#70478 = CARTESIAN_POINT ( 'NONE',  ( 4.243569643749999898, 13.29687500061451644, -27.54997392385601529 ) ) ;
#70479 = CARTESIAN_POINT ( 'NONE',  ( 3.487500001229035362, 4.330127018922191873, 2.499999999999999556 ) ) ;
#70480 = CARTESIAN_POINT ( 'NONE',  ( 29.37187500061451928, 3.027376345333611329, 5.243569643749999010 ) ) ;
#70481 = DIRECTION ( 'NONE',  ( -1.000000000000000000, -0.000000000000000000, -0.000000000000000000 ) ) ;
#70482 = CARTESIAN_POINT ( 'NONE',  ( 7.396875000614519635, -3.027376345333614438, 5.243569643749998122 ) ) ;
#70483 = CARTESIAN_POINT ( 'NONE',  ( 29.50312500061451360, -4.541064518000417216, -2.621784821875001281 ) ) ;
#70484 = CARTESIAN_POINT ( 'NONE',  ( 4.837952263367122363, -3.387542794378833211, -4.619743054822007089 ) ) ;
#70485 = CARTESIAN_POINT ( 'NONE',  ( 11.43750000122903465, 6.123233995736764310E-16, -4.999999999999998224 ) ) ;
#70486 = CARTESIAN_POINT ( 'NONE',  ( -3.999999999999999112, 20.00000000000000000, 30.00000000000000000 ) ) ;
#70487 = CARTESIAN_POINT ( 'NONE',  ( 6.046875000614519102, -3.027376345333614438, 5.243569643749998122 ) ) ;
#70488 = CARTESIAN_POINT ( 'NONE',  ( 10.50937500061451679, 0.000000000000000000, 5.243569643749999010 ) ) ;
#70489 = CARTESIAN_POINT ( 'NONE',  ( 4.012500000000001954, -5.773502691896255534, -1.060575238724906372E-15 ) ) ;
#70490 = CARTESIAN_POINT ( 'NONE',  ( 4.243569643749999898, 13.69062500061459176, 32.45002607614398471 ) ) ;
#70492 = MECHANICAL_DESIGN_GEOMETRIC_PRESENTATION_REPRESENTATION (  '', ( #41039 ), #68221 ) ;
#70491 = CARTESIAN_POINT ( 'NONE',  ( 5.850000000000001421, -4.330127018922190985, -2.500000000000001332 ) ) ;
#70493 = CARTESIAN_POINT ( 'NONE',  ( 14.67187500061451644, 5.824947211148865298E-16, -4.756430356249998326 ) ) ;
#70494 = CARTESIAN_POINT ( 'NONE',  ( 21.21562500061451573, 3.027376345333611329, 5.243569643749999010 ) ) ;
#70495 = CARTESIAN_POINT ( 'NONE',  ( 11.87812500061451537, -4.541064518000419881, 2.621784821874995952 ) ) ;
#70496 = CARTESIAN_POINT ( 'NONE',  ( 24.08437500061451075, -2.746126346562642428, -4.756430356249999214 ) ) ;
#70497 = CARTESIAN_POINT ( 'NONE',  ( 8.971875000614515372, 3.027376345333613106, -5.243569643749998122 ) ) ;
#70498 = CARTESIAN_POINT ( 'NONE',  ( 25.05000000000000071, 0.000000000000000000, 4.999999999999998224 ) ) ;
#70499 = CARTESIAN_POINT ( 'NONE',  ( 19.61250000122903359, 4.330127018922192761, -2.499999999999997780 ) ) ;
#70500 = CARTESIAN_POINT ( 'NONE',  ( 28.45312500061451289, 0.000000000000000000, 5.243569643749999010 ) ) ;
#70501 = CARTESIAN_POINT ( 'NONE',  ( 0.000000000000000000, 27.50000000000000000, 30.00000000000000000 ) ) ;
#70502 = CARTESIAN_POINT ( 'NONE',  ( 8.971875000614515372, 3.027376345333613106, -5.243569643749998122 ) ) ;
#70503 = CARTESIAN_POINT ( 'NONE',  ( 13.58437500061451786, 4.541064518000418104, 2.621784821874999949 ) ) ;
#70504 = CARTESIAN_POINT ( 'NONE',  ( 26.40937500061451715, -4.541064518000417216, -2.621784821875001281 ) ) ;
#70505 = CARTESIAN_POINT ( 'NONE',  ( 8.700000001229032165, -2.886751345948193048, -4.999999999999883649 ) ) ;
#70506 = CARTESIAN_POINT ( 'NONE',  ( 11.96250000000000213, 2.886751345948126879, 4.999999999999999112 ) ) ;
#70507 = EDGE_CURVE ( 'NONE', #1970, #68292, #50712, .T. ) ;
#70508 = CARTESIAN_POINT ( 'NONE',  ( 20.52187500061451786, -6.054752690667223547, -1.112240025338166033E-15 ) ) ;
#70509 = CARTESIAN_POINT ( 'NONE',  ( 12.23437500061451821, 4.541064518000418104, 2.621784821874999949 ) ) ;
#70510 = CARTESIAN_POINT ( 'NONE',  ( 3.756430356249998770, 13.05312499938548321, 32.16877607737302469 ) ) ;
#70511 = CARTESIAN_POINT ( 'NONE',  ( 24.22500000000000142, -4.330127018922194537, 2.499999999999995559 ) ) ;
#70512 = CARTESIAN_POINT ( 'NONE',  ( 3.999999999999998668, 16.06250000000000000, 32.30940107675850470 ) ) ;
#70513 = CARTESIAN_POINT ( 'NONE',  ( 9.001249775931846008E-16, 11.87187500061451750, -25.09994784771203058 ) ) ;
#70514 = CARTESIAN_POINT ( 'NONE',  ( 25.84687500061451360, -2.746126346562646425, 4.756430356249996549 ) ) ;
#70515 = CARTESIAN_POINT ( 'NONE',  ( 15.59062500061451573, -3.027376345333610441, -5.243569643749999898 ) ) ;
#70516 = CARTESIAN_POINT ( 'NONE',  ( 5.250000000000000888, 0.000000000000000000, 4.999999999999998224 ) ) ;
#70517 = CARTESIAN_POINT ( 'NONE',  ( 2.393811435568372112E-14, 18.23750000000000071, 34.00000000000000000 ) ) ;
#70518 = DIRECTION ( 'NONE',  ( -0.000000000000000000, -1.000000000000000000, -0.000000000000000000 ) ) ;
#70519 = CARTESIAN_POINT ( 'NONE',  ( 13.46249999999999858, -5.773502691896255534, -1.060575238724906372E-15 ) ) ;
#70520 = EDGE_CURVE ( 'NONE', #43636, #27655, #62942, .T. ) ;
#70521 = CARTESIAN_POINT ( 'NONE',  ( -2.828200636599751609E-16, 17.30000000122903359, 25.38119784648299770 ) ) ;
#70522 = CARTESIAN_POINT ( 'NONE',  ( 11.10000000122903252, 5.773502691896255534, 3.535250795749688894E-16 ) ) ;
#70523 = CARTESIAN_POINT ( 'NONE',  ( 22.02187500061452141, 3.027376345333613106, -5.243569643749998122 ) ) ;
#70524 = CARTESIAN_POINT ( 'NONE',  ( 16.65937500061452070, 4.541064518000418104, -2.621784821874998173 ) ) ;
#70525 = DIRECTION ( 'NONE',  ( -1.000000000000000000, 0.000000000000000000, 0.000000000000000000 ) ) ;
#70526 = VERTEX_POINT ( 'NONE', #19314 ) ;
#70527 = CARTESIAN_POINT ( 'NONE',  ( 18.51562500061451289, 3.027376345333611329, 5.243569643749999010 ) ) ;
#70528 = CARTESIAN_POINT ( 'NONE',  ( 3.890625000614517326, -3.027376345333610441, -5.243569643749999898 ) ) ;
#70529 = CARTESIAN_POINT ( 'NONE',  ( 18.75937500061451857, -4.541064518000417216, -2.621784821875001281 ) ) ;
#70530 = CARTESIAN_POINT ( 'NONE',  ( 28.17187500061451644, -6.054752690667223547, -1.112240025338166033E-15 ) ) ;
#70531 = CARTESIAN_POINT ( 'NONE',  ( 4.153125000614515727, 0.000000000000000000, 5.243569643749999010 ) ) ;
#70532 = CARTESIAN_POINT ( 'NONE',  ( 19.67812500061451786, 6.421520780324663323E-16, -5.243569643749999010 ) ) ;
#70533 = CARTESIAN_POINT ( 'NONE',  ( -3.000416591977282496E-16, 14.74062500061451786, 25.09994784771203058 ) ) ;
#70534 = CARTESIAN_POINT ( 'NONE',  ( 16.23750000122903359, -4.330127018922194537, 2.499999999999995559 ) ) ;
#70535 = CARTESIAN_POINT ( 'NONE',  ( 11.93437500061451573, -4.119189519843968306, 2.378215178124996054 ) ) ;
#70536 = CARTESIAN_POINT ( 'NONE',  ( 7.340625000614518392, -3.027376345333614438, 5.243569643749998122 ) ) ;
#70537 = CARTESIAN_POINT ( 'NONE',  ( 29.09062500061451573, -3.027376345333610441, -5.243569643749999898 ) ) ;
#70538 = CARTESIAN_POINT ( 'NONE',  ( 23.10937500061451644, 0.000000000000000000, 5.243569643749999010 ) ) ;
#70539 = CARTESIAN_POINT ( 'NONE',  ( 14.99062500061451786, -3.027376345333614438, 5.243569643749998122 ) ) ;
#70540 = CARTESIAN_POINT ( 'NONE',  ( 25.68750000122903288, -4.330127018922194537, 2.499999999999995559 ) ) ;
#70541 = CARTESIAN_POINT ( 'NONE',  ( 23.61562500061451431, -6.054752690667223547, -1.112240025338166033E-15 ) ) ;
#70542 = CARTESIAN_POINT ( 'NONE',  ( 18.75937500061451857, -4.541064518000417216, -2.621784821875001281 ) ) ;
#70543 = CARTESIAN_POINT ( 'NONE',  ( 15.70312500061451644, 4.541064518000418104, -2.621784821874998173 ) ) ;
#70544 = CARTESIAN_POINT ( 'NONE',  ( -4.243569643749999898, 14.87187500061451928, 27.54997392385601529 ) ) ;
#70545 = CARTESIAN_POINT ( 'NONE',  ( 20.72812500061451502, 4.541064518000418104, 2.621784821874999949 ) ) ;
#70546 = CARTESIAN_POINT ( 'NONE',  ( 28.52812500061451573, -4.541064518000419881, 2.621784821874995952 ) ) ;
#70547 = ORIENTED_EDGE ( 'NONE', *, *, #65932, .T. ) ;
#70548 = ORIENTED_EDGE ( 'NONE', *, *, #16156, .F. ) ;
#70549 = CARTESIAN_POINT ( 'NONE',  ( 23.21250000000000213, 2.886751345948126879, 4.999999999999999112 ) ) ;
#70550 = CARTESIAN_POINT ( 'NONE',  ( -3.000416591977282496E-16, 19.74687500061451928, -34.90005215228797653 ) ) ;
#70551 = CARTESIAN_POINT ( 'NONE',  ( 16.16250000000000142, -5.773502691896255534, -1.060575238724906372E-15 ) ) ;
#70552 = CARTESIAN_POINT ( 'NONE',  ( 27.55312500061451786, 0.000000000000000000, 5.243569643749999010 ) ) ;
#70553 = CARTESIAN_POINT ( 'NONE',  ( 8.278125000614515727, -4.541064518000419881, 2.621784821874995952 ) ) ;
#70554 = CARTESIAN_POINT ( 'NONE',  ( 20.10000000122903074, 5.773502691896255534, 3.535250795749688894E-16 ) ) ;
#70555 = CARTESIAN_POINT ( 'NONE',  ( 25.97812500061451502, 6.421520780324663323E-16, -5.243569643749999010 ) ) ;
#70556 = CARTESIAN_POINT ( 'NONE',  ( 24.41250000000000142, 2.886751345948129099, -4.999999999999998224 ) ) ;
#70557 = CARTESIAN_POINT ( 'NONE',  ( 26.95312500061451644, 4.541064518000418104, -2.621784821874998173 ) ) ;
#70558 = CARTESIAN_POINT ( 'NONE',  ( 9.140625000614518214, -3.027376345333614438, 5.243569643749998122 ) ) ;
#70559 = VERTEX_POINT ( 'NONE', #1635 ) ;
#70560 = CARTESIAN_POINT ( 'NONE',  ( 22.56562500061451715, 3.027376345333611329, 5.243569643749999010 ) ) ;
#70561 = CARTESIAN_POINT ( 'NONE',  ( 4.940625000614515372, 6.054752690667223547, 3.707466751127219781E-16 ) ) ;
#70562 = UNCERTAINTY_MEASURE_WITH_UNIT (LENGTH_MEASURE( 1.000000000000000082E-05 ), #54189, 'distance_accuracy_value', 'NONE');
#70563 = CARTESIAN_POINT ( 'NONE',  ( 13.62187500061451750, 2.746126346562643317, 4.756430356249998326 ) ) ;
#70564 = CARTESIAN_POINT ( 'NONE',  ( 3.290625000614516793, -3.027376345333614438, 5.243569643749998122 ) ) ;
#70565 = CARTESIAN_POINT ( 'NONE',  ( 2.121784821874999061, 19.70937500061451786, -33.67503911421598417 ) ) ;
#70566 = CARTESIAN_POINT ( 'NONE',  ( 13.95000000000000107, -4.330127018922190985, -2.500000000000001332 ) ) ;
#70567 = CARTESIAN_POINT ( 'NONE',  ( 14.33437500061451786, 6.421520780324663323E-16, -5.243569643749999010 ) ) ;
#70568 = CARTESIAN_POINT ( 'NONE',  ( 8.212500001229035007, -4.330127018922190985, -2.500000000000001332 ) ) ;
#70569 = CARTESIAN_POINT ( 'NONE',  ( 15.49687500061451750, -3.027376345333614438, 5.243569643749998122 ) ) ;
#70570 = CARTESIAN_POINT ( 'NONE',  ( 14.73749999999999893, -2.886751345948129988, 4.999999999999997335 ) ) ;
#70571 = CARTESIAN_POINT ( 'NONE',  ( 8.896875000614517859, -3.027376345333610441, -5.243569643749999898 ) ) ;
#70572 = CARTESIAN_POINT ( 'NONE',  ( 16.91250000000000142, 2.886751345948182834, 4.999999999999902300 ) ) ;
#70573 = CARTESIAN_POINT ( 'NONE',  ( 24.78750000000000142, -2.886751345948126435, -5.000000000000000000 ) ) ;
#70574 = CARTESIAN_POINT ( 'NONE',  ( 12.57187500061451857, 3.027376345333613106, -5.243569643749998122 ) ) ;
#70575 = ORIENTED_EDGE ( 'NONE', *, *, #14684, .T. ) ;
#70576 = CARTESIAN_POINT ( 'NONE',  ( 23.16562500061451502, -6.054752690667223547, -1.112240025338166033E-15 ) ) ;
#70577 = DIRECTION ( 'NONE',  ( -1.000000000000000000, -0.000000000000000000, -0.000000000000000000 ) ) ;
#70578 = LINE ( 'NONE', #42139, #61141 ) ;
#70579 = CARTESIAN_POINT ( 'NONE',  ( 26.25937500061451857, 0.000000000000000000, 5.243569643749999010 ) ) ;
#70580 = CARTESIAN_POINT ( 'NONE',  ( 4.490625000614516971, 6.054752690667223547, 3.707466751127219781E-16 ) ) ;
#70581 = CARTESIAN_POINT ( 'NONE',  ( 22.39687500061451431, 4.119189519843966529, -2.378215178124998275 ) ) ;
#70582 = CARTESIAN_POINT ( 'NONE',  ( 16.99687500061451573, -3.027376345333610441, -5.243569643749999898 ) ) ;
#70583 = CARTESIAN_POINT ( 'NONE',  ( 9.271875000614517859, 5.824947211148865298E-16, -4.756430356249998326 ) ) ;
#70584 = CARTESIAN_POINT ( 'NONE',  ( 26.55000000122902648, -2.886751345948129988, 4.999999999999997335 ) ) ;
#70585 = CARTESIAN_POINT ( 'NONE',  ( 6.159375000614517148, -4.541064518000417216, -2.621784821875001281 ) ) ;
#70586 = CARTESIAN_POINT ( 'NONE',  ( 15.60937500061451644, -4.541064518000417216, -2.621784821875001281 ) ) ;
#70587 = CARTESIAN_POINT ( 'NONE',  ( 6.600000000000001421, 0.000000000000000000, 4.999999999999998224 ) ) ;
#70588 = CARTESIAN_POINT ( 'NONE',  ( 24.75000000000000000, -4.330127018922190985, -2.500000000000001332 ) ) ;
#70589 = CARTESIAN_POINT ( 'NONE',  ( 27.60937500061451644, 0.000000000000000000, 5.243569643749999010 ) ) ;
#70590 = CARTESIAN_POINT ( 'NONE',  ( 3.756430356249998770, 14.06562499938548250, 32.16877607737302469 ) ) ;
#70591 = CARTESIAN_POINT ( 'NONE',  ( 8.868750001229031454, 2.886751345948182834, 4.999999999999902300 ) ) ;
#70592 = CARTESIAN_POINT ( 'NONE',  ( 7.237500000000000711, -2.886751345948125991, -5.000000000000000000 ) ) ;
#70593 = CARTESIAN_POINT ( 'NONE',  ( 9.534375000614517148, -2.746126346562646425, 4.756430356249996549 ) ) ;
#70594 = CARTESIAN_POINT ( 'NONE',  ( 22.97812500061451857, 4.541064518000418104, 2.621784821874999949 ) ) ;
#70595 = CARTESIAN_POINT ( 'NONE',  ( 12.78749999999999964, 5.773502691896255534, 3.535250795749688894E-16 ) ) ;
#70596 =( BOUNDED_CURVE ( )  B_SPLINE_CURVE ( 2, ( #53632, #54371, #30730, #2300, #59522, #53262, #8935 ),
 .UNSPECIFIED., .F., .F. ) 
 B_SPLINE_CURVE_WITH_KNOTS ( ( 3, 2, 2, 3 ),
 ( 0.5416666666666666297, 0.5444444444444443976, 0.5472222222222222765, 0.5500000000000000444 ),
 .UNSPECIFIED. ) 
 CURVE ( )  GEOMETRIC_REPRESENTATION_ITEM ( )  RATIONAL_B_SPLINE_CURVE ( ( 1.000000000000000000, 0.8660254037844387076, 1.000000000000000000, 0.8660254037844387076, 1.000000000000000000, 0.8660254037844387076, 1.000000000000000000 ) ) 
 REPRESENTATION_ITEM ( '' )  );
#70597 = CARTESIAN_POINT ( 'NONE',  ( 6.028125000614517504, -4.541064518000419881, 2.621784821874995952 ) ) ;
#70598 = CARTESIAN_POINT ( 'NONE',  ( 18.59999999999999787, 4.330127018922192761, -2.499999999999997780 ) ) ;
#70599 = ADVANCED_FACE ( 'NONE', ( #68502 ), #40425, .F. ) ;
#70600 = CARTESIAN_POINT ( 'NONE',  ( 19.34062500061451573, 6.054752690667223547, 3.707466751127219781E-16 ) ) ;
#70601 = CARTESIAN_POINT ( 'NONE',  ( 14.88749999999999929, -2.886751345948126435, -5.000000000000000000 ) ) ;
#70602 = CARTESIAN_POINT ( 'NONE',  ( 24.26250000122903216, 0.000000000000000000, 4.999999999999998224 ) ) ;
#70603 = CARTESIAN_POINT ( 'NONE',  ( -1.878215178124999163, 19.54062499938548214, 26.74683588394047007 ) ) ;
#70604 = CARTESIAN_POINT ( 'NONE',  ( 5.437500000000001776, -2.886751345948125991, -5.000000000000000000 ) ) ;
#70605 = ORIENTED_EDGE ( 'NONE', *, *, #4912, .F. ) ;
#70606 = CARTESIAN_POINT ( 'NONE',  ( 19.52812500061451573, -4.541064518000419881, 2.621784821874995952 ) ) ;
#70607 = CARTESIAN_POINT ( 'NONE',  ( 27.66562500061451146, -6.054752690667223547, -1.112240025338166033E-15 ) ) ;
#70608 = CARTESIAN_POINT ( 'NONE',  ( 24.15937500061451715, -4.541064518000417216, -2.621784821875001281 ) ) ;
#70609 = CARTESIAN_POINT ( 'NONE',  ( 7.912499999999999645, 2.886751345948126879, 4.999999999999999112 ) ) ;
#70610 = CARTESIAN_POINT ( 'NONE',  ( 11.84062500061451750, -3.027376345333614438, 5.243569643749998122 ) ) ;
#70611 = CARTESIAN_POINT ( 'NONE',  ( 26.76562500061451644, -6.054752690667223547, -1.112240025338166033E-15 ) ) ;
#70612 = CARTESIAN_POINT ( 'NONE',  ( 15.94687500061451502, -3.027376345333614438, 5.243569643749998122 ) ) ;
#70613 = CARTESIAN_POINT ( 'NONE',  ( 9.028125000614517504, 4.541064518000418104, 2.621784821874999949 ) ) ;
#70614 = CARTESIAN_POINT ( 'NONE',  ( 4.243569643749999898, 11.49687500061451928, 32.45002607614398471 ) ) ;
#70615 = CARTESIAN_POINT ( 'NONE',  ( 23.81250000122903288, 0.000000000000000000, 4.999999999999998224 ) ) ;
#70616 = CARTESIAN_POINT ( 'NONE',  ( 19.02187500061451786, 2.746126346562643317, 4.756430356249998326 ) ) ;
#70617 = CARTESIAN_POINT ( 'NONE',  ( 13.19062500061451537, -3.027376345333614438, 5.243569643749998122 ) ) ;
#70618 = CARTESIAN_POINT ( 'NONE',  ( 10.62187500061451928, -6.054752690667223547, -1.112240025338166033E-15 ) ) ;
#70619 = CARTESIAN_POINT ( 'NONE',  ( 9.834375000614517859, 6.421520780324663323E-16, -5.243569643749999010 ) ) ;
#70620 = VERTEX_POINT ( 'NONE', #23422 ) ;
#70621 = CARTESIAN_POINT ( 'NONE',  ( 21.70312500061451644, 0.000000000000000000, 5.243569643749999010 ) ) ;
#70622 = CARTESIAN_POINT ( 'NONE',  ( 16.65937500061452070, 4.541064518000418104, -2.621784821874998173 ) ) ;
#70623 = CARTESIAN_POINT ( 'NONE',  ( 22.75312500061451360, -4.541064518000417216, -2.621784821875001281 ) ) ;
#70624 = CARTESIAN_POINT ( 'NONE',  ( -3.999999999999999556, 12.31250000000000000, 27.69059892324149530 ) ) ;
#70625 = CARTESIAN_POINT ( 'NONE',  ( 28.00312500061451715, 0.000000000000000000, 5.243569643749999010 ) ) ;
#70626 = CARTESIAN_POINT ( 'NONE',  ( 6.450000001229034829, -2.886751345948125991, -5.000000000000000000 ) ) ;
#70627 = EDGE_LOOP ( 'NONE', ( #23927, #53243, #35283, #43439 ) ) ;
#70628 = CARTESIAN_POINT ( 'NONE',  ( 29.58749999999999858, -2.886751345948129988, 4.999999999999997335 ) ) ;
#70629 = CARTESIAN_POINT ( 'NONE',  ( -3.999999999999999556, 17.71249999999999858, -32.30940107675850470 ) ) ;
#70630 = CARTESIAN_POINT ( 'NONE',  ( 23.62500000122902932, 2.886751345948129099, -4.999999999999998224 ) ) ;
#70631 = CARTESIAN_POINT ( 'NONE',  ( -3.756430356250001434, 16.16562499938548569, 32.16877607737301048 ) ) ;
#70632 = CARTESIAN_POINT ( 'NONE',  ( 6.384375000614516793, 4.541064518000418104, 2.621784821874999949 ) ) ;
#70633 = CARTESIAN_POINT ( 'NONE',  ( 4.396896640047911475, 2.380805009064795197, -4.642950682235516879 ) ) ;
#70634 = CARTESIAN_POINT ( 'NONE',  ( 15.40312500061451573, 0.000000000000000000, 5.243569643749999010 ) ) ;
#70635 = CARTESIAN_POINT ( 'NONE',  ( 7.996875000614519280, -3.027376345333610441, -5.243569643749999898 ) ) ;
#70636 = CARTESIAN_POINT ( 'NONE',  ( 26.10000000122903430, -2.886751345948129988, 4.999999999999997335 ) ) ;
#70637 = CARTESIAN_POINT ( 'NONE',  ( 16.95937500061451786, -4.541064518000417216, -2.621784821875001281 ) ) ;
#70638 = CARTESIAN_POINT ( 'NONE',  ( 6.121875000614517504, -6.054752690667223547, -1.112240025338166033E-15 ) ) ;
#70639 = CARTESIAN_POINT ( 'NONE',  ( 3.999999999999998668, 18.76250000000000284, 32.30940107675850470 ) ) ;
#70640 = CARTESIAN_POINT ( 'NONE',  ( 5.503125000614516260, 0.000000000000000000, 5.243569643749999010 ) ) ;
#70641 = CARTESIAN_POINT ( 'NONE',  ( 16.26562500061451289, 3.027376345333611329, 5.243569643749999010 ) ) ;
#70642 = EDGE_LOOP ( 'NONE', ( #5452, #42815, #60176, #59164 ) ) ;
#70643 = CARTESIAN_POINT ( 'NONE',  ( 11.72812500061451857, 4.541064518000418104, 2.621784821874999949 ) ) ;
#70644 = CARTESIAN_POINT ( 'NONE',  ( 4.687500001229034652, 6.123233995736764310E-16, -4.999999999999998224 ) ) ;
#70645 = CARTESIAN_POINT ( 'NONE',  ( 10.34062500061451750, 6.054752690667223547, 3.707466751127219781E-16 ) ) ;
#70646 = CARTESIAN_POINT ( 'NONE',  ( 20.48437500061451289, -4.119189519843968306, 2.378215178124996054 ) ) ;
#70647 = CARTESIAN_POINT ( 'NONE',  ( 11.32500000000000107, 6.123233995736764310E-16, -4.999999999999998224 ) ) ;
#70648 = CARTESIAN_POINT ( 'NONE',  ( 4.050000001229035362, -2.886751345948129988, 4.999999999999997335 ) ) ;
#70649 = CARTESIAN_POINT ( 'NONE',  ( 19.34999999999999787, -4.330127018922190985, -2.500000000000001332 ) ) ;
#70650 =( BOUNDED_CURVE ( )  B_SPLINE_CURVE ( 2, ( #20529, #15002, #37539, #55632, #55995, #62260, #56708 ),
 .UNSPECIFIED., .F., .F. ) 
 B_SPLINE_CURVE_WITH_KNOTS ( ( 3, 2, 2, 3 ),
 ( 0.9300000000000001599, 0.9333333333333334592, 0.9366666666666668695, 0.9400000000000001688 ),
 .UNSPECIFIED. ) 
 CURVE ( )  GEOMETRIC_REPRESENTATION_ITEM ( )  RATIONAL_B_SPLINE_CURVE ( ( 0.9999999999999955591, 0.8660254037844431485, 1.000000000000000000, 0.8660254037844387076, 1.000000000000000000, 0.8660254037844298258, 1.000000000000008882 ) ) 
 REPRESENTATION_ITEM ( '' )  );
#70651 = CARTESIAN_POINT ( 'NONE',  ( 15.87187500061451573, 3.027376345333611329, 5.243569643749999010 ) ) ;
#70652 = CARTESIAN_POINT ( 'NONE',  ( 16.01250000122903216, 4.330127018922192761, -2.499999999999997780 ) ) ;
#70653 = CARTESIAN_POINT ( 'NONE',  ( 21.52499999999999858, -4.330127018922194537, 2.499999999999995559 ) ) ;
#70654 = CARTESIAN_POINT ( 'NONE',  ( -2.121784821874999949, 17.92812500061451786, -33.67503911421598417 ) ) ;
#70655 = CARTESIAN_POINT ( 'NONE',  ( -3.999999999999997335, 16.10000000122903430, 32.30940107675850470 ) ) ;
#70656 = CARTESIAN_POINT ( 'NONE',  ( -1.243387493232115393E-14, 16.15624999877096712, 26.00000000000000000 ) ) ;
#70657 = CARTESIAN_POINT ( 'NONE',  ( 28.41562500061451502, 3.027376345333611329, 5.243569643749999010 ) ) ;
#70658 = DIRECTION ( 'NONE',  ( -1.000000000000000000, -0.000000000000000000, -0.000000000000000000 ) ) ;
#70659 = CARTESIAN_POINT ( 'NONE',  ( 19.55625000122903145, 4.330127018922192761, -2.499999999999997780 ) ) ;
#70660 = CARTESIAN_POINT ( 'NONE',  ( 15.83437500061451608, 4.541064518000418104, 2.621784821874999949 ) ) ;
#70661 = CARTESIAN_POINT ( 'NONE',  ( 29.28749999999999787, -2.886751345948125991, -5.000000000000000000 ) ) ;
#70662 = CARTESIAN_POINT ( 'NONE',  ( 12.81562500061451537, -6.054752690667223547, -1.112240025338166033E-15 ) ) ;
#70663 = CARTESIAN_POINT ( 'NONE',  ( 7.218750001229033764, -5.773502691896255534, -1.060575238724906372E-15 ) ) ;
#70664 = CARTESIAN_POINT ( 'NONE',  ( 24.79687500061451999, 6.054752690667223547, 3.707466751127219781E-16 ) ) ;
#70665 = CARTESIAN_POINT ( 'NONE',  ( 17.03437500061451715, 5.492252693125287522, 3.363034840372157021E-16 ) ) ;
#70666 = CARTESIAN_POINT ( 'NONE',  ( 10.26562500061451644, 3.027376345333613106, -5.243569643749998122 ) ) ;
#70667 = CARTESIAN_POINT ( 'NONE',  ( 13.50937500061451679, 4.541064518000418104, -2.621784821874998173 ) ) ;
#70668 = ORIENTED_EDGE ( 'NONE', *, *, #53326, .T. ) ;
#70669 = CARTESIAN_POINT ( 'NONE',  ( 23.74687500061451573, -3.027376345333610441, -5.243569643749999898 ) ) ;
#70670 = CARTESIAN_POINT ( 'NONE',  ( 27.62812500061451360, -4.541064518000419881, 2.621784821874995952 ) ) ;
#70671 = ADVANCED_FACE ( 'NONE', ( #52231 ), #48590, .T. ) ;
#70672 = DIRECTION ( 'NONE',  ( -0.000000000000000000, -1.000000000000000000, -0.000000000000000000 ) ) ;
#70673 = CARTESIAN_POINT ( 'NONE',  ( 6.675000000000000711, -4.330127018922194537, 2.499999999999995559 ) ) ;
#70674 = CARTESIAN_POINT ( 'NONE',  ( 16.05000000122903359, 5.773502691896255534, 3.535250795749688894E-16 ) ) ;
#70675 = CARTESIAN_POINT ( 'NONE',  ( -1.999999999999997113, 17.93750000122903288, -26.53589838486224295 ) ) ;
#70676 = FACE_OUTER_BOUND ( 'NONE', #64893, .T. ) ;
#70677 = VERTEX_POINT ( 'NONE', #21111 ) ;
#70678 = CARTESIAN_POINT ( 'NONE',  ( 14.28750000000000142, -2.886751345948129988, 4.999999999999997335 ) ) ;
#70679 = CARTESIAN_POINT ( 'NONE',  ( 19.01249999999999929, 2.886751345948129099, -4.999999999999998224 ) ) ;
#70680 = CARTESIAN_POINT ( 'NONE',  ( 14.35312500061451679, 4.541064518000418104, -2.621784821874998173 ) ) ;
#70681 = ORIENTED_EDGE ( 'NONE', *, *, #38932, .F. ) ;
#70682 = CARTESIAN_POINT ( 'NONE',  ( 3.999999999999999112, 18.53750000122903430, -30.00000000000000000 ) ) ;
#70683 = CARTESIAN_POINT ( 'NONE',  ( -3.000416591977282496E-16, 17.04687500061451644, -34.90005215228797653 ) ) ;
#70684 = CARTESIAN_POINT ( 'NONE',  ( 6.928125000614516082, -4.541064518000419881, 2.621784821874995952 ) ) ;
#70685 = CARTESIAN_POINT ( 'NONE',  ( -1.999999999999999112, 14.00000000000000000, 26.53589838486224650 ) ) ;
#70686 = CARTESIAN_POINT ( 'NONE',  ( 11.96250000000000213, 2.886751345948126879, 4.999999999999999112 ) ) ;
#70687 = CARTESIAN_POINT ( 'NONE',  ( 28.50937500061451857, -5.492252693125287522, -1.008910452111647106E-15 ) ) ;
#70688 = ORIENTED_EDGE ( 'NONE', *, *, #40125, .F. ) ;
#70689 = CARTESIAN_POINT ( 'NONE',  ( 4.243569643749999898, 15.49062500061451786, 32.45002607614398471 ) ) ;
#70690 = CARTESIAN_POINT ( 'NONE',  ( 27.47812500061451502, 4.541064518000418104, 2.621784821874999949 ) ) ;
#70691 = DIRECTION ( 'NONE',  ( -0.000000000000000000, -1.000000000000000000, -0.000000000000000000 ) ) ;
#70692 = CARTESIAN_POINT ( 'NONE',  ( -1.878215178125001827, 20.59062499938548285, 33.25316411605952283 ) ) ;
#70693 = CARTESIAN_POINT ( 'NONE',  ( 22.88437500061451857, 6.421520780324663323E-16, -5.243569643749999010 ) ) ;
#70694 = CARTESIAN_POINT ( 'NONE',  ( 19.82812500061451644, 4.541064518000418104, 2.621784821874999949 ) ) ;
#70695 = CARTESIAN_POINT ( 'NONE',  ( 4.243569643749999010, 13.31562500061459531, -32.45002607614398471 ) ) ;
#70696 = CARTESIAN_POINT ( 'NONE',  ( 23.28750000122903430, 4.330127018922191873, 2.499999999999999556 ) ) ;
#70697 = CARTESIAN_POINT ( 'NONE',  ( 4.490625000614516971, 6.054752690667223547, 3.707466751127219781E-16 ) ) ;
#70698 = CARTESIAN_POINT ( 'NONE',  ( 26.14687500061451431, 5.492252693125287522, 3.363034840372157021E-16 ) ) ;
#70699 = CARTESIAN_POINT ( 'NONE',  ( 20.46562500061451573, -6.054752690667223547, -1.112240025338166033E-15 ) ) ;
#70700 = CARTESIAN_POINT ( 'NONE',  ( 9.759375000614516793, -4.119189519843965641, -2.378215178125001383 ) ) ;
#70701 = CARTESIAN_POINT ( 'NONE',  ( 3.756430356250000102, 16.24062499938548143, 30.00000000000000000 ) ) ;
#70702 = CARTESIAN_POINT ( 'NONE',  ( 16.54687500061451644, -3.027376345333610441, -5.243569643749999898 ) ) ;
#70703 = CARTESIAN_POINT ( 'NONE',  ( 17.74687500061451928, -3.027376345333614438, 5.243569643749998122 ) ) ;
#70704 = CARTESIAN_POINT ( 'NONE',  ( 23.70937500061451786, -4.541064518000417216, -2.621784821875001281 ) ) ;
#70705 = CARTESIAN_POINT ( 'NONE',  ( -4.243569643749999898, 14.87187500061451928, 27.54997392385601529 ) ) ;
#70706 = CARTESIAN_POINT ( 'NONE',  ( 4.265625000614517326, -6.054752690667223547, -1.112240025338166033E-15 ) ) ;
#70707 = CARTESIAN_POINT ( 'NONE',  ( 28.64062500061451289, -3.027376345333610441, -5.243569643749999898 ) ) ;
#70708 = CARTESIAN_POINT ( 'NONE',  ( 28.45312500061451289, 0.000000000000000000, 5.243569643749999010 ) ) ;
#70709 = DIRECTION ( 'NONE',  ( 1.000000000000000000, -0.000000000000000000, -0.000000000000000000 ) ) ;
#70710 = CARTESIAN_POINT ( 'NONE',  ( 3.999999999999999112, 19.32500000000000284, 30.00000000000000000 ) ) ;
#70711 = CARTESIAN_POINT ( 'NONE',  ( 2.953125000614516438, -4.541064518000417216, -2.621784821875001281 ) ) ;
#70712 = CARTESIAN_POINT ( 'NONE',  ( 6.534375000614517148, -4.541064518000419881, 2.621784821874995952 ) ) ;
#70713 = CARTESIAN_POINT ( 'NONE',  ( 13.57500000122903572, -5.773502691896255534, -1.060575238724906372E-15 ) ) ;
#70714 = CARTESIAN_POINT ( 'NONE',  ( 12.03750000122903430, 4.330127018922191873, 2.499999999999999556 ) ) ;
#70715 = CARTESIAN_POINT ( 'NONE',  ( 4.678125000614516971, -4.541064518000419881, 2.621784821874995952 ) ) ;
#70716 = CARTESIAN_POINT ( 'NONE',  ( 1.999999999999997335, 15.06874999877096677, 33.46410161513775705 ) ) ;
#70717 = CARTESIAN_POINT ( 'NONE',  ( 21.69375000122903430, -2.886751345948125991, -5.000000000000000000 ) ) ;
#70718 = CARTESIAN_POINT ( 'NONE',  ( 14.70937500061451786, -4.541064518000417216, -2.621784821875001281 ) ) ;
#70719 = CARTESIAN_POINT ( 'NONE',  ( 21.22500000000000142, 6.123233995736764310E-16, -4.999999999999998224 ) ) ;
#70720 = VERTEX_POINT ( 'NONE', #26675 ) ;
#70721 = CARTESIAN_POINT ( 'NONE',  ( 22.45312500061451644, 4.541064518000418104, -2.621784821874998173 ) ) ;
#70722 = CARTESIAN_POINT ( 'NONE',  ( 8.053125000614516082, 4.541064518000418104, -2.621784821874998173 ) ) ;
#70723 = CARTESIAN_POINT ( 'NONE',  ( 24.60937500061451644, -4.541064518000417216, -2.621784821875001281 ) ) ;
#70724 = CARTESIAN_POINT ( 'NONE',  ( 7.265625000614516438, 3.027376345333611329, 5.243569643749999010 ) ) ;
#70725 = CARTESIAN_POINT ( 'NONE',  ( 23.19375000122903074, 5.773502691896255534, 3.535250795749688401E-16 ) ) ;
#70726 = CARTESIAN_POINT ( 'NONE',  ( 7.875000001229034652, 2.886751345948129099, -4.999999999999998224 ) ) ;
#70727 = CARTESIAN_POINT ( 'NONE',  ( 22.52812500061451573, 4.541064518000418104, 2.621784821874999949 ) ) ;
#70728 = CARTESIAN_POINT ( 'NONE',  ( 4.243569643749999010, 11.51562500061451644, -32.45002607614398471 ) ) ;
#70729 = CARTESIAN_POINT ( 'NONE',  ( 10.72500000122903252, 2.886751345948126879, 4.999999999999999112 ) ) ;
#70730 = CARTESIAN_POINT ( 'NONE',  ( 19.86562500061451786, 3.027376345333611329, 5.243569643749999010 ) ) ;
#70731 = CARTESIAN_POINT ( 'NONE',  ( 18.70312500061451644, -4.541064518000417216, -2.621784821875001281 ) ) ;
#70732 = CARTESIAN_POINT ( 'NONE',  ( 27.38437500061451857, 5.824947211148865298E-16, -4.756430356249998326 ) ) ;
#70733 = CARTESIAN_POINT ( 'NONE',  ( 17.21249999999999858, 2.886751345948129099, -4.999999999999998224 ) ) ;
#70734 = CARTESIAN_POINT ( 'NONE',  ( 13.23750000122903359, 6.123233995736764310E-16, -4.999999999999998224 ) ) ;
#70735 = CARTESIAN_POINT ( 'NONE',  ( 9.290625000614515017, -3.027376345333610441, -5.243569643749999898 ) ) ;
#70736 = CARTESIAN_POINT ( 'NONE',  ( 14.24062500061451608, -3.027376345333610441, -5.243569643749999898 ) ) ;
#70737 = ADVANCED_FACE ( 'NONE', ( #48836 ), #31843, .F. ) ;
#70738 = CARTESIAN_POINT ( 'NONE',  ( 22.38750000122903216, 4.330127018922191873, 2.499999999999999556 ) ) ;
#70739 = CARTESIAN_POINT ( 'NONE',  ( 22.73437500061451644, -4.541064518000419881, 2.621784821874995952 ) ) ;
#70740 = CARTESIAN_POINT ( 'NONE',  ( 20.44687500061451857, -3.027376345333614438, 5.243569643749998122 ) ) ;
#70741 = CARTESIAN_POINT ( 'NONE',  ( 3.581485683406023135, 3.488985925492861906, -3.914339967783176721 ) ) ;
#70742 = VECTOR ( 'NONE', #21418, 1000.000000000000000 ) ;
#70743 = EDGE_CURVE ( 'NONE', #5008, #68026, #49572, .T. ) ;
#70744 = CARTESIAN_POINT ( 'NONE',  ( 7.012500001229035718, 4.330127018922192761, -2.499999999999997780 ) ) ;
#70745 = CARTESIAN_POINT ( 'NONE',  ( 7.434375000614519280, -4.541064518000419881, 2.621784821874995952 ) ) ;
#70746 = CARTESIAN_POINT ( 'NONE',  ( 22.62187500061451573, 3.027376345333611329, 5.243569643749999010 ) ) ;
#70747 = EDGE_CURVE ( 'NONE', #15624, #10453, #48473, .T. ) ;
#70748 = CARTESIAN_POINT ( 'NONE',  ( -3.999999999999999112, 12.68750000000000000, 27.69059892324149530 ) ) ;
#70749 = CARTESIAN_POINT ( 'NONE',  ( 19.79062500061451502, 6.054752690667223547, 3.707466751127219781E-16 ) ) ;
#70750 = CARTESIAN_POINT ( 'NONE',  ( 24.57187500061451502, -6.054752690667223547, -1.112240025338166033E-15 ) ) ;
#70751 = CARTESIAN_POINT ( 'NONE',  ( 1.878215178125000495, 19.57812499938548356, 26.74683588394047007 ) ) ;
#70752 = LINE ( 'NONE', #36769, #10245 ) ;
#70753 = DIRECTION ( 'NONE',  ( 1.000000000000000000, -0.000000000000000000, 0.000000000000000000 ) ) ;
#70754 = CARTESIAN_POINT ( 'NONE',  ( 5.409375000614516260, 4.541064518000418104, -2.621784821874998173 ) ) ;
#70755 = CARTESIAN_POINT ( 'NONE',  ( 16.34062500061451573, -3.027376345333614438, 5.243569643749998122 ) ) ;
#70756 = CARTESIAN_POINT ( 'NONE',  ( 13.65937500061451715, 0.000000000000000000, 5.243569643749999010 ) ) ;
#70757 = EDGE_LOOP ( 'NONE', ( #3097, #50429, #24557, #54296 ) ) ;
#70758 = DIRECTION ( 'NONE',  ( -1.000000000000000000, -0.000000000000000000, -0.000000000000000000 ) ) ;
#70759 = CARTESIAN_POINT ( 'NONE',  ( 24.17812500061451786, 6.421520780324663323E-16, -5.243569643749999010 ) ) ;
#70760 = CARTESIAN_POINT ( 'NONE',  ( 3.517413553188016628, 3.553619953230496176, -3.820619027221005659 ) ) ;
#70761 = CARTESIAN_POINT ( 'NONE',  ( 28.16250000000000142, 2.886751345948119774, 5.000000000000010658 ) ) ;
#70762 = CARTESIAN_POINT ( 'NONE',  ( 15.41250000000000142, 2.886751345948129099, -4.999999999999998224 ) ) ;
#70763 = CARTESIAN_POINT ( 'NONE',  ( 23.70000000122903216, 5.773502691896255534, 3.535250795749688894E-16 ) ) ;
#70764 = CARTESIAN_POINT ( 'NONE',  ( 18.17812500061451786, -4.541064518000419881, 2.621784821874995952 ) ) ;
#70765 = VERTEX_POINT ( 'NONE', #32937 ) ;
#70766 = CARTESIAN_POINT ( 'NONE',  ( 22.38749999999999929, -2.886751345948129988, 4.999999999999997335 ) ) ;
#70767 = CARTESIAN_POINT ( 'NONE',  ( 24.04687500061451644, -3.027376345333614438, 5.243569643749998122 ) ) ;
#70768 = ORIENTED_EDGE ( 'NONE', *, *, #19616, .T. ) ;
#70769 = CARTESIAN_POINT ( 'NONE',  ( 13.31250000122903288, 4.330127018922192761, -2.499999999999997780 ) ) ;
#70770 = CARTESIAN_POINT ( 'NONE',  ( 12.10312500061451857, 4.541064518000418104, -2.621784821874998173 ) ) ;
#70771 = CARTESIAN_POINT ( 'NONE',  ( 4.228125000614517681, -4.541064518000419881, 2.621784821874995952 ) ) ;
#70772 = CARTESIAN_POINT ( 'NONE',  ( 16.35937500061451644, -5.492252693125287522, -1.008910452111647106E-15 ) ) ;
#70773 = CARTESIAN_POINT ( 'NONE',  ( 27.81562500061452070, 3.027376345333613106, -5.243569643749998122 ) ) ;
#70774 = CARTESIAN_POINT ( 'NONE',  ( 12.90000000122903145, 5.773502691896255534, 3.535250795749688894E-16 ) ) ;
#70775 = CARTESIAN_POINT ( 'NONE',  ( 19.79999999999999716, -4.330127018922190985, -2.500000000000001332 ) ) ;
#70776 = CARTESIAN_POINT ( 'NONE',  ( 26.69999999999999929, 4.330127018922192761, -2.499999999999997780 ) ) ;
#70777 = DIRECTION ( 'NONE',  ( -1.000000000000000000, -0.000000000000000000, -0.000000000000000000 ) ) ;
#70778 = CARTESIAN_POINT ( 'NONE',  ( 6.309375000614517504, 4.541064518000418104, -2.621784821874998173 ) ) ;
#70779 = CARTESIAN_POINT ( 'NONE',  ( 16.80937500061451573, 0.000000000000000000, 5.243569643749999010 ) ) ;
#70780 = DIRECTION ( 'NONE',  ( 0.000000000000000000, 0.000000000000000000, 1.000000000000000000 ) ) ;
#70781 = ORIENTED_EDGE ( 'NONE', *, *, #9299, .T. ) ;
#70782 = CARTESIAN_POINT ( 'NONE',  ( 26.27812500061451573, -4.541064518000419881, 2.621784821874995952 ) ) ;
#70783 = CARTESIAN_POINT ( 'NONE',  ( 26.67187500061451644, 3.027376345333611329, 5.243569643749999010 ) ) ;
#70785 = ADVANCED_FACE ( 'NONE', ( #38107 ), #35408, .T. ) ;
#70784 = PLANE ( 'NONE',  #27437 ) ;
#70786 = CARTESIAN_POINT ( 'NONE',  ( 16.57499999999999929, -4.330127018922194537, 2.499999999999995559 ) ) ;
#70787 = CARTESIAN_POINT ( 'NONE',  ( 14.27812500061451573, 6.421520780324663323E-16, -5.243569643749999010 ) ) ;
#70788 = CARTESIAN_POINT ( 'NONE',  ( -3.999999999999999112, 15.01250000000000107, -32.30940107675850470 ) ) ;
#70789 = CARTESIAN_POINT ( 'NONE',  ( 9.806250001229033231, 0.000000000000000000, 4.999999999999998224 ) ) ;
#70790 = CARTESIAN_POINT ( 'NONE',  ( 29.24062500061451431, 6.054752690667223547, 3.707466751127219781E-16 ) ) ;
#70791 = CARTESIAN_POINT ( 'NONE',  ( 18.03750000122903430, -4.330127018922194537, 2.499999999999995559 ) ) ;
#70792 = CARTESIAN_POINT ( 'NONE',  ( 27.01875000122903359, -5.773502691896255534, -1.060575238724906372E-15 ) ) ;
#70793 = CARTESIAN_POINT ( 'NONE',  ( 18.79687500061451644, -2.746126346562642428, -4.756430356249999214 ) ) ;
#70794 = CARTESIAN_POINT ( 'NONE',  ( 4.078125000614517326, 4.541064518000418104, 2.621784821874999949 ) ) ;
#70795 = CARTESIAN_POINT ( 'NONE',  ( 25.13437500061451502, 6.421520780324663323E-16, -5.243569643749999010 ) ) ;
#70796 = CARTESIAN_POINT ( 'NONE',  ( -4.243569643749997233, 18.09687500061452070, 32.45002607614398471 ) ) ;
#70797 = CARTESIAN_POINT ( 'NONE',  ( 24.83437500061451431, 4.541064518000418104, 2.621784821874999949 ) ) ;
#70798 = CARTESIAN_POINT ( 'NONE',  ( 5.737499999999998934, -2.886751345948129988, 4.999999999999997335 ) ) ;
#70799 = CARTESIAN_POINT ( 'NONE',  ( 8.484601909799253346E-16, 10.77500000122903501, 34.61880215351700230 ) ) ;
#70800 = CARTESIAN_POINT ( 'NONE',  ( 12.14062500061451821, 6.054752690667223547, 3.707466751127219781E-16 ) ) ;
#70801 = CARTESIAN_POINT ( 'NONE',  ( 3.562500001229033764, 0.000000000000000000, 4.999999999999998224 ) ) ;
#70802 = CARTESIAN_POINT ( 'NONE',  ( 8.334375000614516082, -4.541064518000419881, 2.621784821874995952 ) ) ;
#70803 = FACE_OUTER_BOUND ( 'NONE', #23571, .T. ) ;
#70804 = EDGE_LOOP ( 'NONE', ( #28946, #37061 ) ) ;
#70805 = CARTESIAN_POINT ( 'NONE',  ( 11.09062500061451573, -3.027376345333610441, -5.243569643749999898 ) ) ;
#70806 = CARTESIAN_POINT ( 'NONE',  ( 13.47187500061451537, 3.027376345333613106, -5.243569643749998122 ) ) ;
#70807 = CARTESIAN_POINT ( 'NONE',  ( 45.00000000000000000, 0.000000000000000000, 0.000000000000000000 ) ) ;
#70808 = CARTESIAN_POINT ( 'NONE',  ( 22.68750000122903288, 6.123233995736764310E-16, -4.999999999999998224 ) ) ;
#70809 = CARTESIAN_POINT ( 'NONE',  ( 10.02187500061451964, 3.027376345333611329, 5.243569643749999010 ) ) ;
#70810 = CARTESIAN_POINT ( 'NONE',  ( 13.19062500061451537, -3.027376345333614438, 5.243569643749998122 ) ) ;
#70811 = CARTESIAN_POINT ( 'NONE',  ( 28.51875000122903359, 2.886751345948129099, -4.999999999999998224 ) ) ;
#70812 = CARTESIAN_POINT ( 'NONE',  ( 20.55937500061451573, -4.541064518000417216, -2.621784821875001281 ) ) ;
#70813 = CARTESIAN_POINT ( 'NONE',  ( 45.00000000000000000, 0.000000000000000000, 0.000000000000000000 ) ) ;
#70814 = CARTESIAN_POINT ( 'NONE',  ( -3.992479141629563077, 3.010095094815110617, 30.28109884793043705 ) ) ;
#70815 = FACE_OUTER_BOUND ( 'NONE', #16224, .T. ) ;
#70816 = CARTESIAN_POINT ( 'NONE',  ( -2.121784821874996840, 14.53437500061451715, -26.32496088578401583 ) ) ;
#70817 =( BOUNDED_CURVE ( )  B_SPLINE_CURVE ( 2, ( #10387, #55093, #15914, #4493, #60988, #32919, #72439, #16281, #61352 ),
 .UNSPECIFIED., .F., .F. ) 
 B_SPLINE_CURVE_WITH_KNOTS ( ( 3, 2, 2, 2, 3 ),
 ( 0.7500000000000000000, 0.7536231884057971175, 0.7608695652173913526, 0.7681159420289854767, 0.7717391304347825942 ),
 .UNSPECIFIED. ) 
 CURVE ( )  GEOMETRIC_REPRESENTATION_ITEM ( )  RATIONAL_B_SPLINE_CURVE ( ( 0.9330127018922194093, 0.9330127018922194093, 1.000000000000000000, 0.8660254037844387076, 1.000000000000000000, 0.8660254037844387076, 1.000000000000000000, 0.9330127018922194093, 0.9330127018922194093 ) ) 
 REPRESENTATION_ITEM ( '' )  );
#70818 = CARTESIAN_POINT ( 'NONE',  ( 15.98437500061451821, -4.541064518000419881, 2.621784821874995952 ) ) ;
#70819 = CARTESIAN_POINT ( 'NONE',  ( 15.41250000122903252, -4.330127018922190985, -2.500000000000001332 ) ) ;
#70820 = CARTESIAN_POINT ( 'NONE',  ( 12.15937500061451892, 4.541064518000418104, -2.621784821874998173 ) ) ;
#70821 = CARTESIAN_POINT ( 'NONE',  ( 2.121784821874999061, 16.95312500061451999, -33.67503911421598417 ) ) ;
#70822 = CARTESIAN_POINT ( 'NONE',  ( 17.13750000122903216, -4.330127018922194537, 2.499999999999995559 ) ) ;
#70823 = CARTESIAN_POINT ( 'NONE',  ( 13.19062500061451537, -3.027376345333614438, 5.243569643749998122 ) ) ;
#70824 = VERTEX_POINT ( 'NONE', #66342 ) ;
#70825 = CARTESIAN_POINT ( 'NONE',  ( 16.57499999999999929, -4.330127018922194537, 2.499999999999995559 ) ) ;
#70826 = CARTESIAN_POINT ( 'NONE',  ( 30.00000000000000000, 0.000000000000000000, 0.000000000000000000 ) ) ;
#70827 = CARTESIAN_POINT ( 'NONE',  ( 9.759375000614516793, -4.541064518000417216, -2.621784821875001281 ) ) ;
#70828 = CARTESIAN_POINT ( 'NONE',  ( 30.00000000000000000, 0.000000000000000000, 4.999999999999998224 ) ) ;
#70829 = CARTESIAN_POINT ( 'NONE',  ( 11.70000000122903216, -2.886751345948129988, 4.999999999999997335 ) ) ;
#70830 = CARTESIAN_POINT ( 'NONE',  ( 20.47500000122903074, 2.886751345948129099, -4.999999999999998224 ) ) ;
#70831 = CARTESIAN_POINT ( 'NONE',  ( 17.65312500061451573, 0.000000000000000000, 5.243569643749999010 ) ) ;
#70832 = CARTESIAN_POINT ( 'NONE',  ( 20.57812500061451644, 6.421520780324663323E-16, -5.243569643749999010 ) ) ;
#70833 = CARTESIAN_POINT ( 'NONE',  ( 27.93750000122903288, -4.330127018922194537, 2.499999999999995559 ) ) ;
#70834 = CARTESIAN_POINT ( 'NONE',  ( 3.628125000614518036, 4.541064518000418104, 2.621784821874999949 ) ) ;
#70835 = CARTESIAN_POINT ( 'NONE',  ( 25.34999999999999787, 4.330127018922192761, -2.499999999999997780 ) ) ;
#70836 = CARTESIAN_POINT ( 'NONE',  ( 7.734375000614517326, 4.119189519843966529, 2.378215178124999607 ) ) ;
#70837 = CARTESIAN_POINT ( 'NONE',  ( 28.54687500061451644, -3.027376345333614438, 5.243569643749998122 ) ) ;
#70838 = CARTESIAN_POINT ( 'NONE',  ( 1.071796769724493892, 17.61740381056766580, 26.00000000000000711 ) ) ;
#70839 = CARTESIAN_POINT ( 'NONE',  ( -3.000416591977282496E-16, 13.44687500061451857, -34.90005215228797653 ) ) ;
#70840 = CARTESIAN_POINT ( 'NONE',  ( 3.075000001229035718, 2.886751345948126879, 4.999999999999999112 ) ) ;
#70841 = CARTESIAN_POINT ( 'NONE',  ( 4.275000000000001243, 4.330127018922191873, 2.499999999999999556 ) ) ;
#70842 = EDGE_CURVE ( 'NONE', #31816, #51293, #20160, .T. ) ;
#70843 = B_SPLINE_CURVE_WITH_KNOTS ( 'NONE', 3,
 ( #22903, #5929, #44012, #39558, #21457, #66913, #62083, #27383, #11476, #28463 ),
 .UNSPECIFIED., .F., .F.,
 ( 4, 3, 3, 4 ),
 ( 2.022162326929778336E-16, 5.625099572120405517E-05, 9.274853646366114607E-05, 0.0001292481992272784394 ),
 .UNSPECIFIED. ) ;
#70844 = DIRECTION ( 'NONE',  ( 0.000000000000000000, 0.000000000000000000, -1.000000000000000000 ) ) ;
#70845 = CARTESIAN_POINT ( 'NONE',  ( 7.584375000614516082, 6.421520780324663323E-16, -5.243569643749999010 ) ) ;
#70846 = CARTESIAN_POINT ( 'NONE',  ( 26.35312500061451857, -4.541064518000417216, -2.621784821875001281 ) ) ;
#70847 = CARTESIAN_POINT ( 'NONE',  ( 3.999999999999998668, 16.96249999999999858, 32.30940107675850470 ) ) ;
#70848 = CARTESIAN_POINT ( 'NONE',  ( 5.512499999999997513, 2.886751345948062486, -5.000000000000113687 ) ) ;
#70849 = CARTESIAN_POINT ( 'NONE',  ( 8.175000000000002487, 6.123233995736764310E-16, -4.999999999999998224 ) ) ;
#70850 = CARTESIAN_POINT ( 'NONE',  ( 5.071875000614519458, 3.027376345333611329, 5.243569643749999010 ) ) ;
#70851 = CARTESIAN_POINT ( 'NONE',  ( 9.759375000614516793, -4.541064518000417216, -2.621784821875001281 ) ) ;
#70852 = CARTESIAN_POINT ( 'NONE',  ( 3.149999999999999911, -4.330127018922190985, -2.500000000000001332 ) ) ;
#70853 =( BOUNDED_CURVE ( )  B_SPLINE_CURVE ( 2, ( #38263, #60791, #30716, #52889, #28638, #51176, #56706, #39741, #943 ),
 .UNSPECIFIED., .F., .F. ) 
 B_SPLINE_CURVE_WITH_KNOTS ( ( 3, 2, 2, 2, 3 ),
 ( 0.8369565217391304879, 0.8405797101449274944, 0.8478260869565217295, 0.8550724637681159646, 0.8586956521739130821 ),
 .UNSPECIFIED. ) 
 CURVE ( )  GEOMETRIC_REPRESENTATION_ITEM ( )  RATIONAL_B_SPLINE_CURVE ( ( 0.9330127018922192983, 0.9330127018922202975, 1.000000000000000000, 0.8660254037844387076, 1.000000000000000000, 0.8660254037844387076, 1.000000000000000000, 0.9330127018922194093, 0.9330127018922194093 ) ) 
 REPRESENTATION_ITEM ( '' )  );
#70854 = CARTESIAN_POINT ( 'NONE',  ( -4.243569643749999898, 12.60312500061459495, 30.00000000000000000 ) ) ;
#70855 = CARTESIAN_POINT ( 'NONE',  ( 28.49999999999999645, 4.330127018922192761, -2.499999999999997780 ) ) ;
#70856 = CARTESIAN_POINT ( 'NONE',  ( 4.237500000000001599, 5.773502691896255534, 3.535250795749688894E-16 ) ) ;
#70857 = CARTESIAN_POINT ( 'NONE',  ( 15.38437500061451679, -2.746126346562646425, 4.756430356249996549 ) ) ;
#70858 = ORIENTED_EDGE ( 'NONE', *, *, #22395, .F. ) ;
#70859 = CARTESIAN_POINT ( 'NONE',  ( 20.01562500061451644, -6.054752690667223547, -1.112240025338166033E-15 ) ) ;
#70860 = CARTESIAN_POINT ( 'NONE',  ( 10.15312500061451750, -4.541064518000417216, -2.621784821875001281 ) ) ;
#70861 = CARTESIAN_POINT ( 'NONE',  ( 23.52187500061451431, -4.119189519843968306, 2.378215178124996054 ) ) ;
#70862 = CARTESIAN_POINT ( 'NONE',  ( 7.359375000614516438, 0.000000000000000000, 5.243569643749999010 ) ) ;
#70863 = CARTESIAN_POINT ( 'NONE',  ( 23.17500000000000071, 4.330127018922191873, 2.499999999999999556 ) ) ;
#70864 = CARTESIAN_POINT ( 'NONE',  ( 20.02500000122903145, 2.886751345948129099, -4.999999999999998224 ) ) ;
#70865 = CARTESIAN_POINT ( 'NONE',  ( 27.14062500061451644, -3.027376345333614438, 5.243569643749998122 ) ) ;
#70866 = CARTESIAN_POINT ( 'NONE',  ( 0.000000000000000000, 20.00000000000000000, -33.99999999999999289 ) ) ;
#70867 = CARTESIAN_POINT ( 'NONE',  ( 8.746875000614515727, -3.027376345333614438, 5.243569643749998122 ) ) ;
#70868 = CARTESIAN_POINT ( 'NONE',  ( 13.54687500061451999, 6.054752690667223547, 3.707466751127219781E-16 ) ) ;
#70869 = CARTESIAN_POINT ( 'NONE',  ( 24.45937500061451786, 0.000000000000000000, 5.243569643749999010 ) ) ;
#70870 = CARTESIAN_POINT ( 'NONE',  ( 23.28750000000000142, -2.886751345948130876, 4.999999999999996447 ) ) ;
#70871 = CARTESIAN_POINT ( 'NONE',  ( 13.31250000000000178, 2.886751345948126879, 4.999999999999999112 ) ) ;
#70872 = CARTESIAN_POINT ( 'NONE',  ( 20.25937500061451857, 4.541064518000418104, -2.621784821874998173 ) ) ;
#70873 = CARTESIAN_POINT ( 'NONE',  ( 8.821875000614518569, -6.054752690667223547, -1.112240025338166033E-15 ) ) ;
#70874 = CARTESIAN_POINT ( 'NONE',  ( 1.878215178124997609, 19.87812499938548072, 33.25316411605952993 ) ) ;
#70875 = CARTESIAN_POINT ( 'NONE',  ( 22.91249999999999432, -5.773502691896255534, -1.060575238724906372E-15 ) ) ;
#70876 = CARTESIAN_POINT ( 'NONE',  ( 1.999999999999997335, 16.02500000000000213, 33.46410161513775705 ) ) ;
#70877 = CARTESIAN_POINT ( 'NONE',  ( 4.243569643749999898, 11.94687500061451857, -27.54997392385601529 ) ) ;
#70878 = CARTESIAN_POINT ( 'NONE',  ( 24.64687500061451431, -2.746126346562642428, -4.756430356249999214 ) ) ;
#70879 = CARTESIAN_POINT ( 'NONE',  ( 13.79062500061451502, -3.027376345333610441, -5.243569643749999898 ) ) ;
#70880 = CARTESIAN_POINT ( 'NONE',  ( 5.775000000000002132, -4.330127018922194537, 2.499999999999995559 ) ) ;
#70881 = LINE ( 'NONE', #54990, #69098 ) ;
#70882 = DIRECTION ( 'NONE',  ( 0.000000000000000000, 0.000000000000000000, 1.000000000000000000 ) ) ;
#70883 = CARTESIAN_POINT ( 'NONE',  ( 12.63749999999999929, -2.886751345948125991, -5.000000000000000000 ) ) ;
#70884 = CARTESIAN_POINT ( 'NONE',  ( 8.484601909799253346E-16, 18.87500000122903643, 34.61880215351700230 ) ) ;
#70886 =( BOUNDED_CURVE ( )  B_SPLINE_CURVE ( 2, ( #58956, #60057, #14265, #37167, #31262, #70788, #19429, #65610, #19802 ),
 .UNSPECIFIED., .F., .F. ) 
 B_SPLINE_CURVE_WITH_KNOTS ( ( 3, 2, 2, 2, 3 ),
 ( 0.4673913043478261087, 0.4710144927536231707, 0.4782608695652174058, 0.4855072463768115854, 0.4891304347826087029 ),
 .UNSPECIFIED. ) 
 CURVE ( )  GEOMETRIC_REPRESENTATION_ITEM ( )  RATIONAL_B_SPLINE_CURVE ( ( 0.9330127018922194093, 0.9330127018922198534, 1.000000000000000000, 0.8660254037844387076, 1.000000000000000000, 0.8660254037844387076, 1.000000000000000000, 0.9330127018922194093, 0.9330127018922194093 ) ) 
 REPRESENTATION_ITEM ( '' )  );
#70885 = CARTESIAN_POINT ( 'NONE',  ( 11.02500000122903501, 2.886751345948129099, -4.999999999999998224 ) ) ;
#70887 = CARTESIAN_POINT ( 'NONE',  ( 23.18437500061451573, -4.541064518000419881, 2.621784821874995952 ) ) ;
#70888 = CARTESIAN_POINT ( 'NONE',  ( 15.75937500061451857, 4.541064518000418104, -2.621784821874998173 ) ) ;
#70889 = DIRECTION ( 'NONE',  ( 0.000000000000000000, 1.000000000000000000, 0.000000000000000000 ) ) ;
#70890 = ORIENTED_EDGE ( 'NONE', *, *, #17622, .F. ) ;
#70891 = CARTESIAN_POINT ( 'NONE',  ( 18.21562500061451573, -6.054752690667223547, -1.112240025338166033E-15 ) ) ;
#70892 = CARTESIAN_POINT ( 'NONE',  ( 2.878125000614517592, -4.541064518000419881, 2.621784821874995952 ) ) ;
#70893 = CARTESIAN_POINT ( 'NONE',  ( 18.53437500061451715, 4.541064518000418104, 2.621784821874999949 ) ) ;
#70894 = CARTESIAN_POINT ( 'NONE',  ( 28.62187500061451573, -6.054752690667223547, -1.112240025338166033E-15 ) ) ;
#70895 = CARTESIAN_POINT ( 'NONE',  ( 5.203125000614518214, -4.541064518000417216, -2.621784821875001281 ) ) ;
#70896 = CARTESIAN_POINT ( 'NONE',  ( 19.82812500061451644, 4.541064518000418104, 2.621784821874999949 ) ) ;
#70897 = EDGE_CURVE ( 'NONE', #53615, #13783, #42714, .T. ) ;
#70898 = CARTESIAN_POINT ( 'NONE',  ( -2.121784821874996840, 13.57812500061451644, 33.67503911421598417 ) ) ;
#70899 = CARTESIAN_POINT ( 'NONE',  ( 17.32500000122903216, 2.886751345948129099, -4.999999999999998224 ) ) ;
#70900 = CARTESIAN_POINT ( 'NONE',  ( 13.20937500061451786, 0.000000000000000000, 4.756430356249998326 ) ) ;
#70901 = CARTESIAN_POINT ( 'NONE',  ( 7.453125000614516438, -4.541064518000417216, -2.621784821875001281 ) ) ;
#70902 = CARTESIAN_POINT ( 'NONE',  ( 27.89062500061451289, 6.054752690667223547, 3.707466751127219781E-16 ) ) ;
#70903 = CARTESIAN_POINT ( 'NONE',  ( 9.637500001229033941, 6.123233995736764310E-16, -4.999999999999998224 ) ) ;
#70904 = CARTESIAN_POINT ( 'NONE',  ( 23.63437500061451502, -4.541064518000419881, 2.621784821874995952 ) ) ;
#70905 = CARTESIAN_POINT ( 'NONE',  ( 13.79062500061451502, -3.027376345333610441, -5.243569643749999898 ) ) ;
#70906 = CARTESIAN_POINT ( 'NONE',  ( 21.67500000122903359, -5.773502691896255534, -1.060575238724906372E-15 ) ) ;
#70907 = CARTESIAN_POINT ( 'NONE',  ( 23.76562500061451644, 3.027376345333613106, -5.243569643749998122 ) ) ;
#70908 = CARTESIAN_POINT ( 'NONE',  ( 18.79687500061451644, -3.027376345333610441, -5.243569643749999898 ) ) ;
#70909 = CARTESIAN_POINT ( 'NONE',  ( 15.47812500061451679, -4.541064518000419881, 2.621784821874995952 ) ) ;
#70910 = CARTESIAN_POINT ( 'NONE',  ( 2.121784821874999061, 13.85937500061451821, 26.32496088578401583 ) ) ;
#70911 =( BOUNDED_CURVE ( )  B_SPLINE_CURVE ( 2, ( #31688, #65661, #43138, #33141, #71581, #55679, #63652 ),
 .UNSPECIFIED., .F., .F. ) 
 B_SPLINE_CURVE_WITH_KNOTS ( ( 3, 2, 2, 3 ),
 ( 0.2666666666666666075, 0.2694444444444444309, 0.2722222222222221988, 0.2750000000000000777 ),
 .UNSPECIFIED. ) 
 CURVE ( )  GEOMETRIC_REPRESENTATION_ITEM ( )  RATIONAL_B_SPLINE_CURVE ( ( 1.000000000000002665, 0.8660254037844360431, 1.000000000000000000, 0.8660254037844387076, 1.000000000000000000, 0.8660254037844360431, 1.000000000000002665 ) ) 
 REPRESENTATION_ITEM ( '' )  );
#70912 = CARTESIAN_POINT ( 'NONE',  ( 18.85312500061451502, 4.541064518000418104, -2.621784821874998173 ) ) ;
#70913 = CARTESIAN_POINT ( 'NONE',  ( 29.76562500061451644, 3.027376345333611329, 5.243569643749999010 ) ) ;
#70914 = VERTEX_POINT ( 'NONE', #8725 ) ;
#70915 = ORIENTED_EDGE ( 'NONE', *, *, #21036, .T. ) ;
#70916 = CARTESIAN_POINT ( 'NONE',  ( 23.58749999999999858, 5.773502691896255534, 3.535250795749688894E-16 ) ) ;
#70917 = CARTESIAN_POINT ( 'NONE',  ( -2.000000000000000000, 10.02500000000000036, -33.46410161513775705 ) ) ;
#70918 = CARTESIAN_POINT ( 'NONE',  ( 3.794436392317134921, -3.256190485932382472, -3.923912810455655542 ) ) ;
#70919 = CARTESIAN_POINT ( 'NONE',  ( 25.86562500061451431, -6.054752690667223547, -1.112240025338166033E-15 ) ) ;
#70920 = CARTESIAN_POINT ( 'NONE',  ( 7.003125000614518036, -4.541064518000417216, -2.621784821875001281 ) ) ;
#70921 = CARTESIAN_POINT ( 'NONE',  ( 19.01250000122903216, -4.330127018922190985, -2.500000000000001332 ) ) ;
#70922 = CARTESIAN_POINT ( 'NONE',  ( 24.36562500061451786, 3.027376345333611329, 5.243569643749999010 ) ) ;
#70923 = CARTESIAN_POINT ( 'NONE',  ( 24.14999999999999858, 0.000000000000000000, 4.999999999999998224 ) ) ;
#70924 = CARTESIAN_POINT ( 'NONE',  ( 28.64062500061451289, -3.027376345333610441, -5.243569643749999898 ) ) ;
#70925 = CARTESIAN_POINT ( 'NONE',  ( 8.240625000614516082, -3.027376345333614438, 5.243569643749998122 ) ) ;
#70926 = ORIENTED_EDGE ( 'NONE', *, *, #8865, .T. ) ;
#70927 = CARTESIAN_POINT ( 'NONE',  ( 22.37812500061451360, 6.421520780324663323E-16, -5.243569643749999010 ) ) ;
#70928 = CARTESIAN_POINT ( 'NONE',  ( 5.390625000614518214, 6.054752690667223547, 3.707466751127219781E-16 ) ) ;
#70929 = CARTESIAN_POINT ( 'NONE',  ( 13.99687500061451928, 5.492252693125287522, 3.363034840372157021E-16 ) ) ;
#70930 = CARTESIAN_POINT ( 'NONE',  ( 3.440625000614518036, -3.027376345333610441, -5.243569643749999898 ) ) ;
#70931 = CARTESIAN_POINT ( 'NONE',  ( -3.999999999999999112, 13.36250000122903359, -30.00000000000000000 ) ) ;
#70932 = LINE ( 'NONE', #14768, #36172 ) ;
#70933 = ADVANCED_FACE ( 'NONE', ( #37164 ), #70784, .F. ) ;
#70934 = CARTESIAN_POINT ( 'NONE',  ( 11.62500000000000000, -4.330127018922194537, 2.499999999999995559 ) ) ;
#70935 = CARTESIAN_POINT ( 'NONE',  ( 11.44687500061451857, -3.027376345333614438, 5.243569643749998122 ) ) ;
#70936 = CARTESIAN_POINT ( 'NONE',  ( 7.950000001229033053, 5.773502691896255534, 3.535250795749688894E-16 ) ) ;
#70937 = CARTESIAN_POINT ( 'NONE',  ( 14.37187500061451928, 3.027376345333613106, -5.243569643749998122 ) ) ;
#70938 = CARTESIAN_POINT ( 'NONE',  ( 14.36249999999999893, -5.773502691896255534, -1.060575238724906372E-15 ) ) ;
#70939 = CARTESIAN_POINT ( 'NONE',  ( 7.134375000614516793, 6.421520780324663323E-16, -5.243569643749999010 ) ) ;
#70940 = DIRECTION ( 'NONE',  ( -1.000000000000000000, -0.000000000000000000, -0.000000000000000000 ) ) ;
#70941 = DIRECTION ( 'NONE',  ( -1.000000000000000000, -0.000000000000000000, -0.000000000000000000 ) ) ;
#70942 = CARTESIAN_POINT ( 'NONE',  ( 12.12187500061451573, 3.027376345333613106, -5.243569643749998122 ) ) ;
#70943 = CARTESIAN_POINT ( 'NONE',  ( 3.651773823418189124, 3.415340091791402966, 3.978752903393068863 ) ) ;
#70944 = CARTESIAN_POINT ( 'NONE',  ( 22.82812500061451644, 6.421520780324663323E-16, -5.243569643749999010 ) ) ;
#70945 = CARTESIAN_POINT ( 'NONE',  ( 4.243569643749999898, 11.08437500061451786, 30.00000000000000000 ) ) ;
#70946 = CARTESIAN_POINT ( 'NONE',  ( -4.243569643749998122, 19.39062500061459104, 32.45002607614398471 ) ) ;
#70947 = CARTESIAN_POINT ( 'NONE',  ( 27.00937500061451857, 4.541064518000418104, -2.621784821874998173 ) ) ;
#70948 = CARTESIAN_POINT ( 'NONE',  ( 29.62500000000000000, -4.330127018922194537, 2.499999999999995559 ) ) ;
#70949 = CARTESIAN_POINT ( 'NONE',  ( 5.165625000614518569, -6.054752690667223547, -1.112240025338166033E-15 ) ) ;
#70950 = CARTESIAN_POINT ( 'NONE',  ( 23.33437500061451786, 5.492252693125287522, 3.363034840372157021E-16 ) ) ;
#70951 = CARTESIAN_POINT ( 'NONE',  ( 17.44687500061451857, -3.027376345333610441, -5.243569643749999898 ) ) ;
#70952 = CARTESIAN_POINT ( 'NONE',  ( 9.234375000614514661, -2.746126346562641984, -4.756430356249999214 ) ) ;
#70953 = CARTESIAN_POINT ( 'NONE',  ( 26.32500000122903216, 2.886751345948129099, -4.999999999999998224 ) ) ;
#70954 = CARTESIAN_POINT ( 'NONE',  ( 5.296875000614518214, -3.027376345333610441, -5.243569643749999898 ) ) ;
#70955 = CARTESIAN_POINT ( 'NONE',  ( 16.02187500061451786, -6.054752690667223547, -1.112240025338166033E-15 ) ) ;
#70956 = CARTESIAN_POINT ( 'NONE',  ( 24.60000000000000142, 0.000000000000000000, 4.999999999999998224 ) ) ;
#70957 = CARTESIAN_POINT ( 'NONE',  ( 4.387500001229033053, 4.330127018922191873, 2.499999999999999556 ) ) ;
#70958 = CARTESIAN_POINT ( 'NONE',  ( 27.23437500061451644, -4.541064518000419881, 2.621784821874995952 ) ) ;
#70959 = CARTESIAN_POINT ( 'NONE',  ( 3.756430356250000546, 14.59062499938548463, 27.83122392262697886 ) ) ;
#70960 = CARTESIAN_POINT ( 'NONE',  ( 5.662500001229035185, 4.330127018922192761, -2.499999999999997780 ) ) ;
#70961 = CARTESIAN_POINT ( 'NONE',  ( 7.312500000000000000, 2.886751345948129099, -4.999999999999998224 ) ) ;
#70962 = CARTESIAN_POINT ( 'NONE',  ( 10.43437500061451395, -2.746126346562646425, 4.756430356249996549 ) ) ;
#70963 = CARTESIAN_POINT ( 'NONE',  ( 22.22812500061451502, -4.541064518000419881, 2.621784821874995952 ) ) ;
#70964 = CARTESIAN_POINT ( 'NONE',  ( 11.47499999999999964, 4.330127018922191873, 2.499999999999999556 ) ) ;
#70965 = CARTESIAN_POINT ( 'NONE',  ( 4.678125000614516971, -4.541064518000419881, 2.621784821874995952 ) ) ;
#70966 = CARTESIAN_POINT ( 'NONE',  ( 19.68750000000000355, -2.886751345948129988, 4.999999999999997335 ) ) ;
#70967 = CARTESIAN_POINT ( 'NONE',  ( 19.19062500061452070, -3.027376345333610441, -5.243569643749999898 ) ) ;
#70968 = CARTESIAN_POINT ( 'NONE',  ( -2.556497649636125342E-15, 18.87500000122903288, 34.00000000000000000 ) ) ;
#70969 = CARTESIAN_POINT ( 'NONE',  ( 23.10000000122903074, -2.886751345948125991, -5.000000000000000000 ) ) ;
#70970 = CARTESIAN_POINT ( 'NONE',  ( -3.756430356250000102, 19.16562499938548214, 30.00000000000000000 ) ) ;
#70971 = CARTESIAN_POINT ( 'NONE',  ( 3.712499999999999911, 2.886751345948129099, -4.999999999999998224 ) ) ;
#70972 = ORIENTED_EDGE ( 'NONE', *, *, #61389, .F. ) ;
#70973 = CARTESIAN_POINT ( 'NONE',  ( 20.05312500061451431, -4.541064518000417216, -2.621784821875001281 ) ) ;
#70974 = CARTESIAN_POINT ( 'NONE',  ( 25.37812500061451715, -4.541064518000419881, 2.621784821874995952 ) ) ;
#70975 = CARTESIAN_POINT ( 'NONE',  ( 23.93437500061451573, 4.541064518000418104, 2.621784821874999949 ) ) ;
#70976 = CARTESIAN_POINT ( 'NONE',  ( 9.600000000000001421, 4.330127018922192761, -2.499999999999997780 ) ) ;
#70977 = CARTESIAN_POINT ( 'NONE',  ( 12.89062500061451821, -3.027376345333610441, -5.243569643749999898 ) ) ;
#70978 = CARTESIAN_POINT ( 'NONE',  ( 25.82812500061451644, -4.541064518000419881, 2.621784821874995952 ) ) ;
#70979 = CARTESIAN_POINT ( 'NONE',  ( 16.39687500061451786, -3.027376345333614438, 5.243569643749998122 ) ) ;
#70980 = CARTESIAN_POINT ( 'NONE',  ( 8.240625000614516082, -3.027376345333614438, 5.243569643749998122 ) ) ;
#70981 = CARTESIAN_POINT ( 'NONE',  ( 1.071796769724491893, 14.60134618820329777, 34.00000000000000000 ) ) ;
#70982 = CARTESIAN_POINT ( 'NONE',  ( 4.243569643749999010, 11.57187500061451679, 27.54997392385601174 ) ) ;
#70983 = CARTESIAN_POINT ( 'NONE',  ( 24.67500000122903359, 2.886751345948126879, 4.999999999999999112 ) ) ;
#70984 = CARTESIAN_POINT ( 'NONE',  ( 18.72187500061451360, -5.492252693125287522, -1.008910452111647106E-15 ) ) ;
#70985 = CARTESIAN_POINT ( 'NONE',  ( 15.40312500061451573, 0.000000000000000000, 5.243569643749999010 ) ) ;
#70986 = CARTESIAN_POINT ( 'NONE',  ( 7.659375000614518036, 4.541064518000418104, -2.621784821874998173 ) ) ;
#70987 = CARTESIAN_POINT ( 'NONE',  ( 10.69687500061451679, -3.027376345333610441, -5.243569643749999898 ) ) ;
#70988 = ORIENTED_EDGE ( 'NONE', *, *, #39769, .F. ) ;
#70989 = CARTESIAN_POINT ( 'NONE',  ( 29.52187500061451431, -6.054752690667223547, -1.112240025338166033E-15 ) ) ;
#70990 = CARTESIAN_POINT ( 'NONE',  ( 20.72812500061451502, 4.541064518000418104, 2.621784821874999949 ) ) ;
#70991 = CARTESIAN_POINT ( 'NONE',  ( 17.63437500061451502, 4.541064518000418104, 2.621784821874999949 ) ) ;
#70992 = CARTESIAN_POINT ( 'NONE',  ( 21.96562500061451573, 3.027376345333613106, -5.243569643749998122 ) ) ;
#70993 = CARTESIAN_POINT ( 'NONE',  ( -2.000000000000000000, 12.27500000000000036, 26.53589838486224650 ) ) ;
#70994 = CARTESIAN_POINT ( 'NONE',  ( 26.87812500061451360, 6.421520780324663323E-16, -5.243569643749999010 ) ) ;
#70995 = CARTESIAN_POINT ( 'NONE',  ( 6.487500001229034474, 6.123233995736764310E-16, -4.999999999999998224 ) ) ;
#70996 = ORIENTED_EDGE ( 'NONE', *, *, #26195, .F. ) ;
#70997 = CARTESIAN_POINT ( 'NONE',  ( 45.00000000000000000, 6.123233995736764310E-16, -4.999999999999998224 ) ) ;
#70998 = CARTESIAN_POINT ( 'NONE',  ( -3.999999999999999112, 17.30000000000000071, -30.00000000000000000 ) ) ;
#70999 = CARTESIAN_POINT ( 'NONE',  ( 25.76250000122903216, -4.330127018922190985, -2.500000000000001332 ) ) ;
#71000 = CARTESIAN_POINT ( 'NONE',  ( 2.655984681222220721E-16, 15.56562499938548250, 25.66244784525396483 ) ) ;
#71001 = CARTESIAN_POINT ( 'NONE',  ( 7.846875000614518036, -3.027376345333614438, 5.243569643749998122 ) ) ;
#71002 = CARTESIAN_POINT ( 'NONE',  ( 4.352828865414680948, 2.460460882526558812, -4.510749027574212811 ) ) ;
#71003 = CARTESIAN_POINT ( 'NONE',  ( 14.57812500061451644, -4.541064518000419881, 2.621784821874995952 ) ) ;
#71004 = CARTESIAN_POINT ( 'NONE',  ( 8.446875000614518569, -3.027376345333610441, -5.243569643749999898 ) ) ;
#71005 = CARTESIAN_POINT ( 'NONE',  ( 27.67500000122903359, 2.886751345948129099, -4.999999999999998224 ) ) ;
#71006 = CARTESIAN_POINT ( 'NONE',  ( 17.18437500061451573, 4.541064518000418104, 2.621784821874999949 ) ) ;
#71007 = CARTESIAN_POINT ( 'NONE',  ( 5.184375000614516615, -4.541064518000419881, 2.621784821874995952 ) ) ;
#71008 = CARTESIAN_POINT ( 'NONE',  ( -1.999999999999997113, 11.07500000000000107, 33.46410161513775705 ) ) ;
#71009 = CARTESIAN_POINT ( 'NONE',  ( 5.053125000614517859, 0.000000000000000000, 5.243569643749999010 ) ) ;
#71010 = CARTESIAN_POINT ( 'NONE',  ( 14.99062500061451786, -3.027376345333614438, 5.243569643749998122 ) ) ;
#71011 = ORIENTED_EDGE ( 'NONE', *, *, #35290, .T. ) ;
#71012 = CARTESIAN_POINT ( 'NONE',  ( 13.37812500061451715, 6.421520780324663323E-16, -5.243569643749999010 ) ) ;
#71013 = CARTESIAN_POINT ( 'NONE',  ( 6.075000001229034829, 2.886751345948129099, -4.999999999999998224 ) ) ;
#71014 = CARTESIAN_POINT ( 'NONE',  ( 9.815625000614518925, 3.027376345333613106, -5.243569643749998122 ) ) ;
#71015 = CARTESIAN_POINT ( 'NONE',  ( 20.74687500061451573, 5.492252693125287522, 3.363034840372157021E-16 ) ) ;
#71016 = CARTESIAN_POINT ( 'NONE',  ( 10.80000000000000071, -4.330127018922190985, -2.500000000000001332 ) ) ;
#71017 = CARTESIAN_POINT ( 'NONE',  ( 4.762500001229033941, 4.330127018922192761, -2.499999999999997780 ) ) ;
#71018 = CARTESIAN_POINT ( 'NONE',  ( 17.73750000000000071, 5.773502691896255534, 3.535250795749688894E-16 ) ) ;
#71019 = EDGE_CURVE ( 'NONE', #31243, #44627, #72252, .T. ) ;
#71020 = CARTESIAN_POINT ( 'NONE',  ( 17.67187500061451644, 3.027376345333611329, 5.243569643749999010 ) ) ;
#71021 = CARTESIAN_POINT ( 'NONE',  ( 17.21250000122903145, -4.330127018922190985, -2.500000000000001332 ) ) ;
#71022 = CARTESIAN_POINT ( 'NONE',  ( 21.26249999999999574, 2.886751345948129099, -4.999999999999998224 ) ) ;
#71023 = CARTESIAN_POINT ( 'NONE',  ( -2.121784821874996840, 17.62812500061451715, -26.32496088578401583 ) ) ;
#71024 = LINE ( 'NONE', #25212, #21774 ) ;
#71025 = CARTESIAN_POINT ( 'NONE',  ( 2.737500001229034474, -4.330127018922194537, 2.499999999999995559 ) ) ;
#71026 = LINE ( 'NONE', #65480, #58364 ) ;
#71027 = CARTESIAN_POINT ( 'NONE',  ( 28.71562500061451573, 3.027376345333613106, -5.243569643749998122 ) ) ;
#71028 = CARTESIAN_POINT ( 'NONE',  ( 3.507483327083503521, -3.563363679198468859, 3.507483327083555924 ) ) ;
#71029 = CARTESIAN_POINT ( 'NONE',  ( 3.939080010846523372, -3.079553322829319928, -4.243980907203444453 ) ) ;
#71030 = CARTESIAN_POINT ( 'NONE',  ( 17.18437500061451573, 4.541064518000418104, 2.621784821874999949 ) ) ;
#71031 = EDGE_CURVE ( 'NONE', #4525, #66981, #60787, .T. ) ;
#71032 =( BOUNDED_SURFACE ( )  B_SPLINE_SURFACE ( 1, 2, ( 
 ( #62579, #68494, #23414, #57027, #68140, #19215, #52857, #7789, #25134, #51506, #6433, #23051, #17504, #40065, #30327, #53586, #31049, #63931, #45961, #70210, #2981, #35855, #47315, #11976, #906, #34499, #69848, #28968, #17858, #41769, #36592, #58746, #64298, #41415, #51141, #19585, #540, #45606, #13316, #58378, #14052, #2256, #8519, #24771, #13686, #36230, #2613, #8156, #30685, #53216, #47675, #42141, #64667, #59113, #21853, #69021, #5606, #23576, #29849, #23934, #44416, #27413, #46121, #61381, #18384, #28142, #63098, #33669, #22222, #39227, #44777, #46483, #72468, #66565, #56213, #66943, #1066, #44042, #16669, #29488, #10416, #49944, #12499, #57555, #50670, #67311, #63466, #15945, #35386, #40951, #16311, #68658, #40578, #18022, #61739, #10777, #35027, #12853, #38493, #6957, #52025, #1427, #57909, #7318, #27778, #52385, #33310, #61018, #1791, #32947, #11140, #38865, #55485, #55848, #4877, #5237, #50317, #72840, #50654, #71735, #4861, #21105, #65814, #61723, #11124, #33651, #56196, #43658, #28126, #58, #21472, #10761, #27397, #66180, #49927, #55469, #38476, #15558, #72452, #61000, #16295, #10399, #21836, #32931, #22564, #5589, #38101, #33294, #49201, #55832, #49566, #66547, #38849, #60623, #27035, #32568, #10033, #32201, #44400, #66926, #61364, #72823, #55106, #4506, #60254, #54735, #4137, #5219, #15196, #37734, #44025, #72088, #44760, #9668, #15926, #27761, #26668, #50301, #22206, #67295, #16653, #39211, #46191, #12923, #63171, #68732, #68007, #52458, #24006, #12566, #68369, #11848, #29918, #51736, #45474, #17379, #39937, #56548, #28475, #5942, #23646, #62450, #18457, #29201, #35100, #34731, #23283, #40289, #45832, #46554, #408, #67647, #57260, #22917, #1136, #45112, #17730, #29559, #11489, #51012, #57625, #7029, #6673, #62811, #63537, #17013, #35457, #41021, #34367, #18090, #40651, #52096, #12203, #56900, #1501, #69095, #39571, #57980, #7390, #1865, #62095, #34011, #28833, #6305, #51372, #775, #37288, #41378, #70172, #69812, #59074, #41731, #19549, #19178, #2576, #14015, #42471, #42106, #25470, #58340, #3318, #64629, #8478, #59440, #14746, #36190, #58708, #2941, #53179, #8119, #30647, #31383, #63889, #36919, #48381, #8847, #64994, #64259, #13279, #35818, #25095, #19917, #2221, #31012, #36554, #14384, #53923, #7750, #30287, #53545, #13646, #52819, #25844, #48016, #47639, #70908, #70542, #20280, #42834, #31753, #65356, #24371, #59811, #9216, #69457, #54290, #46919, #18815, #24734, #47278, #5136, #32843, #27671, #9580, #9943, #50209, #72366, #10311, #37648, #38014, #4774, #44675, #21746, #27308, #26576, #11036, #55742, #39119, #33561, #72733, #38761, #32481, #55380, #26948, #44308, #3683, #61634, #20648, #43937, #4419, #55014, #16567, #72006, #15111, #32112, #54646, #22120, #38384, #49841, #26207, #67206, #4050, #60171, #48746, #71644, #49116, #66091, #66837, #16208, #21017, #49474, #60536, #71270, #43205, #21381, #61280, #43570, #66461, #65725, #15838, #15470, #60907, #10673, #33203, #22833, #23565, #22477, #56466, #28389, #69011, #12843, #50927, #5857, #12122, #40942, #62003, #68287, #11405, #56110, #52016, #1417, #23923, #46473, #33924, #18374, #63456, #11765, #1054, #17647, #324, #40207, #45750, #28748, #45385, #62729, #51288, #6590, #689, #34648, #23197, #5500, #28039, #67921, #46110, #39481, #68647, #39855, #56813, #29119, #17292, #62367, #34281, #6220, #45027, #57176, #51653, #18011, #63088, #40568, #12489, #50568, #67562, #16927, #35016, #73095, #57545, #6947, #29478, #14298, #65269, #36105, #19462, #24290, #30203, #46838, #30568, #29838, #41651, #42748, #8033, #35739, #58626, #2139, #2856, #1779, #58258, #7664, #48294, #35376, #52734, #24650, #64541, #20194, #41297, #47556, #63807, #57899, #31295, #53836, #3231, #25758, #13199, #70820, #7308, #64172, #53465, #70085, #47196, #42020, #25014, #53094, #69727, #13934, #2490, #58989, #36471, #8395, #30924, #52373, #69378, #19096, #25386, #18733, #47930, #13560, #70459, #19834, #42386, #64908, #36836, #59350, #8761, #22307, #55931, #61467, #22664, #9497, #65639, #9130, #54200, #3597, #33395, #514, #23025, #44501, #26487, #67748, #45581, #16394, #72925, #26119, #32026, #48658, #44859, #71183, #49029, #16757, #56651, #33755, #39315, #37564, #14656, #17120, #51117, #37199, #39679, #50755, #67034, #67395, #38949, #56300, #59722, #31667, #20556, #5327, #10862, #27868, #28580, #50400, #43114, #15027, #60088, #62199, #61827, #11232, #54562, #11595, #3965, #71558, #34112, #20933, #5690, #28225, #158, #45214, #6046, #18189, #51835, #24833, #58444, #23744, #63634, #23387, #18557, #1598, #18917, #52560, #1239, #52197, #57365, #68113, #7855, #11949, #40759, #40390, #29660, #12303, #63274, #62909, #46292, #57725, #13022, #12666, #69197, #28941, #47021, #35203, #24109, #30017, #30391, #6773, #29305, #46657, #68833, #7130, #41122, #1966, #34474, #7488, #41476, #24475, #35560, #34839, #57002, #6409, #58080, #69556, #45936, #63996, #13377, #35920, #52920, #51479, #880, #2318, #17479, #68467, #40039, #62553, #17829, #9320, #31486, #8953, #70638, #54751, #3423, #47381, #71377, #65094, #19279, #14484, #59542, #9684, #69911, #31853, #37390, #41832, #48115, #54028, #36295, #42205, #58809, #25943, #8220, #8583, #48483, #15212, #65459, #71007, #70278, #4153, #26309, #32217, #64363, #48847, #54389, #3044, #20383, #20013, #14851, #13753, #30748, #53280, #37018, #42566, #25575, #60270, #42934, #2679, #25195, #47740, #20752, #59914, #3785, #19649, #43310, #64729, #14115, #65830, #36654, #59175, #31112, #37752, #53651, #4521, #49942, #10413, #56561, #17027, #55483, #22220, #27050, #10775, #44414, #67309, #61737, #60638, #38117, #33308, #15943, #10051, #11138, #38863, #4875, #33667, #55846, #61379, #72466, #34024, #5234, #26685 ),
 ( #44774, #50315, #49581, #49218, #5604, #62109, #71752, #28140, #56211, #27411, #27776, #21851, #16667, #21121, #11502, #43674, #66941, #16309, #72838, #39585, #39225, #32584, #55123, #72103, #50668, #72, #22578, #66197, #45127, #21488, #44040, #67661, #66563, #38491, #61016, #15575, #32945, #56913, #29213, #62823, #35829, #69470, #34744, #1513, #34381, #1150, #422, #12215, #13292, #51749, #6318, #6685, #45846, #46566, #45489, #28847, #51385, #18827, #5956, #787, #23296, #35113, #63902, #11861, #18102, #68381, #28488, #1878, #24384, #46932, #41390, #17742, #51026, #22930, #57276, #24017, #40664, #40301, #63183, #68744, #23659, #46203, #12579, #57636, #29572, #7042, #52108, #62463, #63549, #69110, #18470, #41034, #12935, #35471, #57992, #68020, #7402, #17393, #29930, #52470, #39950, #25483, #70555, #20662, #58352, #48029, #65369, #14757, #37301, #64271, #64642, #31766, #53936, #3332, #8492, #25107, #43219, #65007, #58720, #30659, #8133, #69824, #41743, #19190, #36933, #2588, #54303, #42484, #25857, #19930, #36567, #53558, #59087, #59824, #13660, #7763, #14395, #36202, #59453, #30300, #31024, #42847, #24747, #53192, #48394, #70922, #8860, #2955, #3695, #52833, #48759, #26220, #47651, #31396, #20292, #9230, #71283, #70183, #65739, #15124, #2233, #47290, #19561, #42117, #14027, #22130, #21393, #21757, #26959, #37661, #50579, #54659, #10322, #9956, #72377, #55027, #32855, #32492, #15849, #27319, #55752, #55391, #38771, #71657, #16577, #4785, #44318, #72745, #28051, #49486, #72017, #16218, #66472, #43949, #38395, #44685, #4062, #50219, #61644, #67216, #5146, #4431, #26588, #49129, #60919, #33213, #15483, #66848, #49851, #27681, #39129, #21030, #43583, #61291, #10683, #66104, #11046, #33572, #56120, #5512, #73106, #22488, #45038, #32125, #67573, #60184, #9593, #38026, #60549, #700, #1068, #6231, #16938, #29850, #33934, #62740, #62378, #51664, #34292, #12132, #11777, #68298, #6601, #35028, #34659, #18023, #50938, #69022, #57188, #23577, #52026, #7319, #28759, #51299, #68659, #45762, #23209, #17658, #23935, #56477, #29489, #40952, #1428, #57556, #56824, #5868, #28400, #40219, #12500, #67932, #46122, #29131, #6958, #46484, #334, #22844, #40579, #63099, #45396, #18385, #63467, #12854, #35387, #57910, #52386, #1792, #24302, #46850, #39493, #62015, #11417, #17305, #39866, #8406, #31678, #69390, #36481, #3241, #25769, #48307, #2151, #2503, #42760, #64919, #14310, #19474, #36118, #54211, #2868, #69739, #41663, #19108, #7678, #52746, #30214, #47941, #13573, #65280, #53476, #36846, #59000, #47568, #64555, #70098, #70831, #24662, #18745, #30935, #47208, #25398, #41309, #42032, #53847, #35750, #64185, #59361, #8773, #70470, #13945, #14668, #63819, #59733, #37211, #58638, #31307, #20205, #19847, #42397, #9141, #13211, #3609, #26130, #8045, #58271, #30580, #53106, #25026, #66021, #66763, #27600, #43126, #38687, #72295, #55309, #72664, #33130, #32402, #32772, #37942, #48669, #61561, #65649, #21310, #20944, #10239, #15400, #43863, #43495, #26873, #38305, #16135, #66388, #49770, #9508, #50132, #15765, #4703, #10602, #39047, #60461, #9870, #27233, #4347, #54942, #49403, #55667, #15038, #61207, #22043, #5064, #44603, #71934, #37575, #60099, #60833, #44231, #26500, #21674, #67134, #16491, #10963, #32040, #54573, #33484, #56034, #3976, #5426, #71195, #20569, #49041, #71570, #62653, #51217, #35300, #57102, #27965, #51940, #45681, #73022, #68215, #40138, #63380, #50496, #17576, #34942, #57469, #6874, #33853, #34210, #1337, #23490, #46037, #618, #67849, #12764, #34574, #28318, #254, #50855, #39411, #11336, #61930, #6512, #45314, #23849, #12050, #68573, #29046, #6148, #23125, #28677, #29406, #56397, #22407, #51582, #5787, #981, #44954, #17932, #12408, #67492, #57821, #22762, #17221, #40495, #16855, #39782, #63011, #62298, #11694, #46397, #68933, #18290, #40863, #56744, #42668, #65192, #36024, #25300, #19378, #35661, #41936, #70008, #53018, #7586, #64461, #2412, #30847, #24933, #13852, #47477, #14582, #25678, #58182, #47848, #63730, #70376, #64092, #7953, #53382, #13120, #41574, #47118, #30122, #46762, #36394, #58908, #8318, #14218, #2063, #52655, #1698, #69297, #18659, #2777, #37115, #7231, #19013, #42302, #19754, #29760, #30490, #64828, #41221, #24573, #69650, #36753, #13475, #58541, #59273, #48214, #8681, #31213, #53754, #52297, #3150, #24210, #70735, #20113, #21588, #15312, #66297, #9780, #27147, #16406, #44512, #3520, #26782, #60371, #37852, #72569, #54848, #71107, #65562, #37490, #10516, #21220, #38213, #67046, #38593, #60010, #43034, #33043, #54486, #9421, #48950, #4617, #72210, #31950, #32314, #43408, #59642, #50044, #4257, #55223, #14951, #49315, #54125, #65933, #9055, #71848, #3887, #43772, #26407, #49681, #26041, #71479, #20855, #21955, #55583, #44141, #66668, #15676, #48580, #20480, #60741, #16045, #10151, #32683, #61119, #4976, #27510, #31586, #50412, #23037, #28236, #22318, #23399, #51129, #67759, #892, #45593, #526, #62211, #46305, #68126, #38960, #62921, #56663, #10873, #6058, #17492, #1252, #61478, #28592, #45949, #68479, #17841, #44871, #45226, #12316, #34486, #57016, #11606, #5700, #23756, #40053, #39326, #11244, #61839, #72937, #67407, #16768, #62565, #56311, #34851, #11962, #6421, #28953, #17131, #34123, #39692, #40402, #33768, #33406, #51492, #50766, #57378, #55943, #6785, #29317, #5340, #171, #51848, #68844, #27879, #22675, #37670, #18201, #9602, #15132, #1610, #25865, #14766, #53945, #36941, #36576, #37310, #71291, #12679, #9239, #42855, #48404, #43228, #3703, #2963, #3342, #8502, #40772, #32134, #35215, #65016, #64651, #70930, #59096, #14404, #14035, #70564, #8869, #59832, #59461, #20301, #52209, #20670, #31405, #65377, #54312, #54667, #31032, #53568, #31775 ) ),
 .UNSPECIFIED., .F., .F., .F. ) 
 B_SPLINE_SURFACE_WITH_KNOTS ( ( 2, 2 ),
 ( 3, 2, 2, 2, 2, 2, 2, 2, 2, 2, 2, 2, 2, 2, 2, 2, 2, 2, 2, 2, 2, 2, 2, 2, 2, 2, 2, 2, 2, 2, 2, 2, 2, 2, 2, 2, 2, 2, 2, 2, 2, 2, 2, 2, 2, 2, 2, 2, 2, 2, 2, 2, 2, 2, 2, 2, 2, 2, 2, 2, 2, 2, 2, 2, 2, 2, 2, 2, 2, 2, 2, 2, 2, 2, 2, 2, 2, 2, 2, 2, 2, 2, 2, 2, 2, 2, 2, 2, 2, 2, 2, 2, 2, 2, 2, 2, 2, 2, 2, 2, 2, 2, 2, 2, 2, 2, 2, 2, 2, 2, 2, 2, 2, 2, 2, 2, 2, 2, 2, 2, 2, 2, 2, 2, 2, 2, 2, 2, 2, 2, 2, 2, 2, 2, 2, 2, 2, 2, 2, 2, 2, 2, 2, 2, 2, 2, 2, 2, 2, 2, 2, 2, 2, 2, 2, 2, 2, 2, 2, 2, 2, 2, 2, 2, 2, 2, 2, 2, 2, 2, 2, 2, 2, 2, 2, 2, 2, 2, 2, 2, 2, 2, 2, 2, 2, 2, 2, 2, 2, 2, 2, 2, 2, 2, 2, 2, 2, 2, 2, 2, 2, 2, 2, 2, 2, 2, 2, 2, 2, 2, 2, 2, 2, 2, 2, 2, 2, 2, 2, 2, 2, 2, 2, 2, 2, 2, 2, 2, 2, 2, 2, 2, 2, 2, 2, 2, 2, 2, 2, 2, 2, 2, 2, 2, 2, 2, 2, 2, 2, 2, 2, 2, 2, 2, 2, 2, 2, 2, 2, 2, 2, 2, 2, 2, 2, 2, 2, 2, 2, 2, 2, 2, 2, 2, 2, 2, 2, 2, 2, 2, 2, 2, 2, 2, 2, 2, 2, 2, 2, 2, 2, 2, 2, 2, 2, 2, 2, 2, 2, 2, 2, 2, 2, 2, 2, 2, 2, 2, 2, 2, 2, 2, 2, 2, 2, 2, 2, 2, 2, 2, 2, 2, 2, 2, 2, 2, 2, 2, 2, 2, 2, 2, 2, 2, 2, 2, 2, 2, 2, 2, 2, 2, 2, 2, 2, 2, 2, 2, 2, 2, 2, 2, 2, 2, 2, 2, 2, 2, 2, 2, 3 ),
 ( 0.000000000000000000, 1.000000000000000000 ),
 ( 0.000000000000000000, 0.002777777777777777884, 0.005555555555555555768, 0.008333333333333333218, 0.01111111111111111154, 0.01388888888888888812, 0.01666666666666666644, 0.01944444444444444475, 0.02222222222222222307, 0.02500000000000000139, 0.02777777777777777624, 0.03055555555555555455, 0.03333333333333333287, 0.03611111111111110772, 0.03888888888888888951, 0.04166666666666666435, 0.04444444444444444614, 0.04722222222222222099, 0.05000000000000000278, 0.05277777777777777762, 0.05555555555555555247, 0.05833333333333333426, 0.06111111111111110911, 0.06388888888888888395, 0.06666666666666666574, 0.06944444444444444753, 0.07222222222222221544, 0.07499999999999999722, 0.07777777777777777901, 0.08055555555555556080, 0.08333333333333332871, 0.08611111111111111049, 0.08888888888888889228, 0.09166666666666666019, 0.09444444444444444198, 0.09722222222222222376, 0.1000000000000000056, 0.1027777777777777735, 0.1055555555555555552, 0.1083333333333333370, 0.1111111111111111049, 0.1138888888888888867, 0.1166666666666666685, 0.1194444444444444503, 0.1222222222222222182, 0.1250000000000000000, 0.1277777777777777679, 0.1305555555555555636, 0.1333333333333333315, 0.1361111111111110994, 0.1388888888888888951, 0.1416666666666666630, 0.1444444444444444309, 0.1472222222222222265, 0.1499999999999999944, 0.1527777777777777901, 0.1555555555555555580, 0.1583333333333333259, 0.1611111111111111216, 0.1638888888888888895, 0.1666666666666666574, 0.1694444444444444531, 0.1722222222222222210, 0.1749999999999999889, 0.1777777777777777846, 0.1805555555555555525, 0.1833333333333333204, 0.1861111111111111160, 0.1888888888888888840, 0.1916666666666666796, 0.1944444444444444475, 0.1972222222222222154, 0.2000000000000000111, 0.2027777777777777790, 0.2055555555555555469, 0.2083333333333333426, 0.2111111111111111105, 0.2138888888888888784, 0.2166666666666666741, 0.2194444444444444420, 0.2222222222222222099, 0.2250000000000000056, 0.2277777777777777735, 0.2305555555555555691, 0.2333333333333333370, 0.2361111111111111049, 0.2388888888888889006, 0.2416666666666666685, 0.2444444444444444364, 0.2472222222222222321, 0.2500000000000000000, 0.2527777777777777679, 0.2555555555555555358, 0.2583333333333333592, 0.2611111111111111271, 0.2638888888888888951, 0.2666666666666666630, 0.2694444444444444309, 0.2722222222222221988, 0.2750000000000000222, 0.2777777777777777901, 0.2805555555555555580, 0.2833333333333333259, 0.2861111111111110938, 0.2888888888888888618, 0.2916666666666666852, 0.2944444444444444531, 0.2972222222222222210, 0.2999999999999999889, 0.3027777777777777568, 0.3055555555555555802, 0.3083333333333333481, 0.3111111111111111160, 0.3138888888888888840, 0.3166666666666666519, 0.3194444444444444198, 0.3222222222222222432, 0.3250000000000000111, 0.3277777777777777790, 0.3305555555555555469, 0.3333333333333333148, 0.3361111111111111382, 0.3388888888888889062, 0.3416666666666666741, 0.3444444444444444420, 0.3472222222222222099, 0.3499999999999999778, 0.3527777777777778012, 0.3555555555555555691, 0.3583333333333333370, 0.3611111111111111049, 0.3638888888888888729, 0.3666666666666666408, 0.3694444444444444642, 0.3722222222222222321, 0.3750000000000000000, 0.3777777777777777679, 0.3805555555555555358, 0.3833333333333333592, 0.3861111111111111271, 0.3888888888888888951, 0.3916666666666666630, 0.3944444444444444309, 0.3972222222222221988, 0.4000000000000000222, 0.4027777777777777901, 0.4055555555555555580, 0.4083333333333333259, 0.4111111111111110938, 0.4138888888888888618, 0.4166666666666666852, 0.4194444444444444531, 0.4222222222222222210, 0.4249999999999999889, 0.4277777777777777568, 0.4305555555555555802, 0.4333333333333333481, 0.4361111111111111160, 0.4388888888888888840, 0.4416666666666666519, 0.4444444444444444198, 0.4472222222222222432, 0.4500000000000000111, 0.4527777777777777790, 0.4555555555555555469, 0.4583333333333333148, 0.4611111111111111382, 0.4638888888888889062, 0.4666666666666666741, 0.4694444444444444420, 0.4722222222222222099, 0.4749999999999999778, 0.4777777777777778012, 0.4805555555555555691, 0.4833333333333333370, 0.4861111111111111049, 0.4888888888888888729, 0.4916666666666666408, 0.4944444444444444642, 0.4972222222222222321, 0.5000000000000000000, 0.5027777777777777679, 0.5055555555555555358, 0.5083333333333333037, 0.5111111111111110716, 0.5138888888888888395, 0.5166666666666667185, 0.5194444444444444864, 0.5222222222222222543, 0.5250000000000000222, 0.5277777777777777901, 0.5305555555555555580, 0.5333333333333333259, 0.5361111111111110938, 0.5388888888888888618, 0.5416666666666666297, 0.5444444444444443976, 0.5472222222222222765, 0.5500000000000000444, 0.5527777777777778123, 0.5555555555555555802, 0.5583333333333333481, 0.5611111111111111160, 0.5638888888888888840, 0.5666666666666666519, 0.5694444444444444198, 0.5722222222222221877, 0.5749999999999999556, 0.5777777777777777235, 0.5805555555555556024, 0.5833333333333333703, 0.5861111111111111382, 0.5888888888888889062, 0.5916666666666666741, 0.5944444444444444420, 0.5972222222222222099, 0.5999999999999999778, 0.6027777777777777457, 0.6055555555555555136, 0.6083333333333332815, 0.6111111111111111605, 0.6138888888888889284, 0.6166666666666666963, 0.6194444444444444642, 0.6222222222222222321, 0.6250000000000000000, 0.6277777777777777679, 0.6305555555555555358, 0.6333333333333333037, 0.6361111111111110716, 0.6388888888888888395, 0.6416666666666667185, 0.6444444444444444864, 0.6472222222222222543, 0.6500000000000000222, 0.6527777777777777901, 0.6555555555555555580, 0.6583333333333333259, 0.6611111111111110938, 0.6638888888888888618, 0.6666666666666666297, 0.6694444444444443976, 0.6722222222222222765, 0.6750000000000000444, 0.6777777777777778123, 0.6805555555555555802, 0.6833333333333333481, 0.6861111111111111160, 0.6888888888888888840, 0.6916666666666666519, 0.6944444444444444198, 0.6972222222222221877, 0.6999999999999999556, 0.7027777777777777235, 0.7055555555555556024, 0.7083333333333333703, 0.7111111111111111382, 0.7138888888888889062, 0.7166666666666666741, 0.7194444444444444420, 0.7222222222222222099, 0.7249999999999999778, 0.7277777777777777457, 0.7305555555555555136, 0.7333333333333332815, 0.7361111111111111605, 0.7388888888888889284, 0.7416666666666666963, 0.7444444444444444642, 0.7472222222222222321, 0.7500000000000000000, 0.7527777777777777679, 0.7555555555555555358, 0.7583333333333333037, 0.7611111111111110716, 0.7638888888888888395, 0.7666666666666667185, 0.7694444444444444864, 0.7722222222222222543, 0.7750000000000000222, 0.7777777777777777901, 0.7805555555555555580, 0.7833333333333333259, 0.7861111111111110938, 0.7888888888888888618, 0.7916666666666666297, 0.7944444444444443976, 0.7972222222222222765, 0.8000000000000000444, 0.8027777777777778123, 0.8055555555555555802, 0.8083333333333333481, 0.8111111111111111160, 0.8138888888888888840, 0.8166666666666666519, 0.8194444444444444198, 0.8222222222222221877, 0.8249999999999999556, 0.8277777777777777235, 0.8305555555555556024, 0.8333333333333333703, 0.8361111111111111382, 0.8388888888888889062, 0.8416666666666666741, 0.8444444444444444420, 0.8472222222222222099, 0.8499999999999999778, 0.8527777777777777457, 0.8555555555555555136, 0.8583333333333332815, 0.8611111111111111605, 0.8638888888888889284, 0.8666666666666666963, 0.8694444444444444642, 0.8722222222222222321, 0.8750000000000000000, 0.8777777777777777679, 0.8805555555555555358, 0.8833333333333333037, 0.8861111111111110716, 0.8888888888888888395, 0.8916666666666667185, 0.8944444444444444864, 0.8972222222222222543, 0.9000000000000000222, 0.9027777777777777901, 0.9055555555555555580, 0.9083333333333333259, 0.9111111111111110938, 0.9138888888888888618, 0.9166666666666666297, 0.9194444444444443976, 0.9222222222222222765, 0.9250000000000000444, 0.9277777777777778123, 0.9305555555555555802, 0.9333333333333333481, 0.9361111111111111160, 0.9388888888888888840, 0.9416666666666666519, 0.9444444444444444198, 0.9472222222222221877, 0.9499999999999999556, 0.9527777777777777235, 0.9555555555555556024, 0.9583333333333333703, 0.9611111111111111382, 0.9638888888888889062, 0.9666666666666666741, 0.9694444444444444420, 0.9722222222222222099, 0.9749999999999999778, 0.9777777777777777457, 0.9805555555555555136, 0.9833333333333332815, 0.9861111111111111605, 0.9888888888888889284, 0.9916666666666666963, 0.9944444444444444642, 0.9972222222222222321, 1.000000000000000000 ),
 .UNSPECIFIED. ) 
 GEOMETRIC_REPRESENTATION_ITEM ( )  RATIONAL_B_SPLINE_SURFACE ( (
 ( 1.000000000000000000, 0.8660254037844387076, 1.000000000000000000, 0.8660254037844387076, 1.000000000000000000, 0.8660254037844387076, 1.000000000000000000, 0.8660254037844387076, 1.000000000000000000, 0.8660254037844387076, 1.000000000000000000, 0.8660254037844387076, 1.000000000000000000, 0.8660254037844387076, 1.000000000000000000, 0.8660254037844387076, 1.000000000000000000, 0.8660254037844387076, 1.000000000000000000, 0.8660254037844387076, 1.000000000000000000, 0.8660254037844387076, 1.000000000000000000, 0.8660254037844387076, 1.000000000000000000, 0.8660254037844387076, 1.000000000000000000, 0.8660254037844387076, 1.000000000000000000, 0.8660254037844387076, 1.000000000000000000, 0.8660254037844387076, 1.000000000000000000, 0.8660254037844387076, 1.000000000000000000, 0.8660254037844387076, 1.000000000000000000, 0.8660254037844387076, 1.000000000000000000, 0.8660254037844387076, 1.000000000000000000, 0.8660254037844387076, 1.000000000000000000, 0.8660254037844387076, 1.000000000000000000, 0.8660254037844387076, 1.000000000000000000, 0.8660254037844387076, 1.000000000000000000, 0.8660254037844387076, 1.000000000000000000, 0.8660254037844387076, 1.000000000000000000, 0.8660254037844387076, 1.000000000000000000, 0.8660254037844387076, 1.000000000000000000, 0.8660254037844387076, 1.000000000000000000, 0.8660254037844387076, 1.000000000000000000, 0.8660254037844387076, 1.000000000000000000, 0.8660254037844387076, 1.000000000000000000, 0.8660254037844387076, 1.000000000000000000, 0.8660254037844387076, 1.000000000000000000, 0.8660254037844387076, 1.000000000000000000, 0.8660254037844387076, 1.000000000000000000, 0.8660254037844387076, 1.000000000000000000, 0.8660254037844387076, 1.000000000000000000, 0.8660254037844387076, 1.000000000000000000, 0.8660254037844387076, 1.000000000000000000, 0.8660254037844387076, 1.000000000000000000, 0.8660254037844387076, 1.000000000000000000, 0.8660254037844387076, 1.000000000000000000, 0.8660254037844387076, 1.000000000000000000, 0.8660254037844387076, 1.000000000000000000, 0.8660254037844387076, 1.000000000000000000, 0.8660254037844387076, 1.000000000000000000, 0.8660254037844387076, 1.000000000000000000, 0.8660254037844387076, 1.000000000000000000, 0.8660254037844387076, 1.000000000000000000, 0.8660254037844387076, 1.000000000000000000, 0.8660254037844387076, 1.000000000000000000, 0.8660254037844387076, 1.000000000000000000, 0.8660254037844387076, 1.000000000000000000, 0.8660254037844387076, 1.000000000000000000, 0.8660254037844387076, 1.000000000000000000, 0.8660254037844387076, 1.000000000000000000, 0.8660254037844387076, 1.000000000000000000, 0.8660254037844387076, 1.000000000000000000, 0.8660254037844387076, 1.000000000000000000, 0.8660254037844387076, 1.000000000000000000, 0.8660254037844387076, 1.000000000000000000, 0.8660254037844387076, 1.000000000000000000, 0.8660254037844387076, 1.000000000000000000, 0.8660254037844387076, 1.000000000000000000, 0.8660254037844387076, 1.000000000000000000, 0.8660254037844387076, 1.000000000000000000, 0.8660254037844387076, 1.000000000000000000, 0.8660254037844387076, 1.000000000000000000, 0.8660254037844387076, 1.000000000000000000, 0.8660254037844387076, 1.000000000000000000, 0.8660254037844387076, 1.000000000000000000, 0.8660254037844387076, 1.000000000000000000, 0.8660254037844387076, 1.000000000000000000, 0.8660254037844387076, 1.000000000000000000, 0.8660254037844387076, 1.000000000000000000, 0.8660254037844387076, 1.000000000000000000, 0.8660254037844387076, 1.000000000000000000, 0.8660254037844387076, 1.000000000000000000, 0.8660254037844387076, 1.000000000000000000, 0.8660254037844387076, 1.000000000000000000, 0.8660254037844387076, 1.000000000000000000, 0.8660254037844387076, 1.000000000000000000, 0.8660254037844387076, 1.000000000000000000, 0.8660254037844387076, 1.000000000000000000, 0.8660254037844387076, 1.000000000000000000, 0.8660254037844387076, 1.000000000000000000, 0.8660254037844387076, 1.000000000000000000, 0.8660254037844387076, 1.000000000000000000, 0.8660254037844387076, 1.000000000000000000, 0.8660254037844387076, 1.000000000000000000, 0.8660254037844387076, 1.000000000000000000, 0.8660254037844387076, 1.000000000000000000, 0.8660254037844387076, 1.000000000000000000, 0.8660254037844387076, 1.000000000000000000, 0.8660254037844387076, 1.000000000000000000, 0.8660254037844387076, 1.000000000000000000, 0.8660254037844387076, 1.000000000000000000, 0.8660254037844387076, 1.000000000000000000, 0.8660254037844387076, 1.000000000000000000, 0.8660254037844387076, 1.000000000000000000, 0.8660254037844387076, 1.000000000000000000, 0.8660254037844387076, 1.000000000000000000, 0.8660254037844387076, 1.000000000000000000, 0.8660254037844387076, 1.000000000000000000, 0.8660254037844387076, 1.000000000000000000, 0.8660254037844387076, 1.000000000000000000, 0.8660254037844387076, 1.000000000000000000, 0.8660254037844387076, 1.000000000000000000, 0.8660254037844387076, 1.000000000000000000, 0.8660254037844387076, 1.000000000000000000, 0.8660254037844387076, 1.000000000000000000, 0.8660254037844387076, 1.000000000000000000, 0.8660254037844387076, 1.000000000000000000, 0.8660254037844387076, 1.000000000000000000, 0.8660254037844387076, 1.000000000000000000, 0.8660254037844387076, 1.000000000000000000, 0.8660254037844387076, 1.000000000000000000, 0.8660254037844387076, 1.000000000000000000, 0.8660254037844387076, 1.000000000000000000, 0.8660254037844387076, 1.000000000000000000, 0.8660254037844387076, 1.000000000000000000, 0.8660254037844387076, 1.000000000000000000, 0.8660254037844387076, 1.000000000000000000, 0.8660254037844387076, 1.000000000000000000, 0.8660254037844387076, 1.000000000000000000, 0.8660254037844387076, 1.000000000000000000, 0.8660254037844387076, 1.000000000000000000, 0.8660254037844387076, 1.000000000000000000, 0.8660254037844387076, 1.000000000000000000, 0.8660254037844387076, 1.000000000000000000, 0.8660254037844387076, 1.000000000000000000, 0.8660254037844387076, 1.000000000000000000, 0.8660254037844387076, 1.000000000000000000, 0.8660254037844387076, 1.000000000000000000, 0.8660254037844387076, 1.000000000000000000, 0.8660254037844387076, 1.000000000000000000, 0.8660254037844387076, 1.000000000000000000, 0.8660254037844387076, 1.000000000000000000, 0.8660254037844387076, 1.000000000000000000, 0.8660254037844387076, 1.000000000000000000, 0.8660254037844387076, 1.000000000000000000, 0.8660254037844387076, 1.000000000000000000, 0.8660254037844387076, 1.000000000000000000, 0.8660254037844387076, 1.000000000000000000, 0.8660254037844387076, 1.000000000000000000, 0.8660254037844387076, 1.000000000000000000, 0.8660254037844387076, 1.000000000000000000, 0.8660254037844387076, 1.000000000000000000, 0.8660254037844387076, 1.000000000000000000, 0.8660254037844387076, 1.000000000000000000, 0.8660254037844387076, 1.000000000000000000, 0.8660254037844387076, 1.000000000000000000, 0.8660254037844387076, 1.000000000000000000, 0.8660254037844387076, 1.000000000000000000, 0.8660254037844387076, 1.000000000000000000, 0.8660254037844387076, 1.000000000000000000, 0.8660254037844387076, 1.000000000000000000, 0.8660254037844387076, 1.000000000000000000, 0.8660254037844387076, 1.000000000000000000, 0.8660254037844387076, 1.000000000000000000, 0.8660254037844387076, 1.000000000000000000, 0.8660254037844387076, 1.000000000000000000, 0.8660254037844387076, 1.000000000000000000, 0.8660254037844387076, 1.000000000000000000, 0.8660254037844387076, 1.000000000000000000, 0.8660254037844387076, 1.000000000000000000, 0.8660254037844387076, 1.000000000000000000, 0.8660254037844387076, 1.000000000000000000, 0.8660254037844387076, 1.000000000000000000, 0.8660254037844387076, 1.000000000000000000, 0.8660254037844387076, 1.000000000000000000, 0.8660254037844387076, 1.000000000000000000, 0.8660254037844387076, 1.000000000000000000, 0.8660254037844387076, 1.000000000000000000, 0.8660254037844387076, 1.000000000000000000, 0.8660254037844387076, 1.000000000000000000, 0.8660254037844387076, 1.000000000000000000, 0.8660254037844387076, 1.000000000000000000, 0.8660254037844387076, 1.000000000000000000, 0.8660254037844387076, 1.000000000000000000, 0.8660254037844387076, 1.000000000000000000, 0.8660254037844387076, 1.000000000000000000, 0.8660254037844387076, 1.000000000000000000, 0.8660254037844387076, 1.000000000000000000, 0.8660254037844387076, 1.000000000000000000, 0.8660254037844387076, 1.000000000000000000, 0.8660254037844387076, 1.000000000000000000, 0.8660254037844387076, 1.000000000000000000, 0.8660254037844387076, 1.000000000000000000, 0.8660254037844387076, 1.000000000000000000, 0.8660254037844387076, 1.000000000000000000, 0.8660254037844387076, 1.000000000000000000, 0.8660254037844387076, 1.000000000000000000, 0.8660254037844387076, 1.000000000000000000, 0.8660254037844387076, 1.000000000000000000, 0.8660254037844387076, 1.000000000000000000, 0.8660254037844387076, 1.000000000000000000, 0.8660254037844387076, 1.000000000000000000, 0.8660254037844387076, 1.000000000000000000, 0.8660254037844387076, 1.000000000000000000, 0.8660254037844387076, 1.000000000000000000, 0.8660254037844387076, 1.000000000000000000, 0.8660254037844387076, 1.000000000000000000, 0.8660254037844387076, 1.000000000000000000, 0.8660254037844387076, 1.000000000000000000, 0.8660254037844387076, 1.000000000000000000, 0.8660254037844387076, 1.000000000000000000, 0.8660254037844387076, 1.000000000000000000, 0.8660254037844387076, 1.000000000000000000, 0.8660254037844387076, 1.000000000000000000, 0.8660254037844387076, 1.000000000000000000, 0.8660254037844387076, 1.000000000000000000, 0.8660254037844387076, 1.000000000000000000, 0.8660254037844387076, 1.000000000000000000, 0.8660254037844387076, 1.000000000000000000, 0.8660254037844387076, 1.000000000000000000, 0.8660254037844387076, 1.000000000000000000, 0.8660254037844387076, 1.000000000000000000, 0.8660254037844387076, 1.000000000000000000, 0.8660254037844387076, 1.000000000000000000, 0.8660254037844387076, 1.000000000000000000, 0.8660254037844387076, 1.000000000000000000, 0.8660254037844387076, 1.000000000000000000, 0.8660254037844387076, 1.000000000000000000, 0.8660254037844387076, 1.000000000000000000, 0.8660254037844387076, 1.000000000000000000, 0.8660254037844387076, 1.000000000000000000, 0.8660254037844387076, 1.000000000000000000, 0.8660254037844387076, 1.000000000000000000, 0.8660254037844387076, 1.000000000000000000, 0.8660254037844387076, 1.000000000000000000, 0.8660254037844387076, 1.000000000000000000, 0.8660254037844387076, 1.000000000000000000, 0.8660254037844387076, 1.000000000000000000, 0.8660254037844387076, 1.000000000000000000, 0.8660254037844387076, 1.000000000000000000, 0.8660254037844387076, 1.000000000000000000, 0.8660254037844387076, 1.000000000000000000, 0.8660254037844387076, 1.000000000000000000, 0.8660254037844387076, 1.000000000000000000, 0.8660254037844387076, 1.000000000000000000, 0.8660254037844387076, 1.000000000000000000, 0.8660254037844387076, 1.000000000000000000, 0.8660254037844387076, 1.000000000000000000, 0.8660254037844387076, 1.000000000000000000, 0.8660254037844387076, 1.000000000000000000, 0.8660254037844387076, 1.000000000000000000, 0.8660254037844387076, 1.000000000000000000, 0.8660254037844387076, 1.000000000000000000, 0.8660254037844387076, 1.000000000000000000, 0.8660254037844387076, 1.000000000000000000, 0.8660254037844387076, 1.000000000000000000, 0.8660254037844387076, 1.000000000000000000, 0.8660254037844387076, 1.000000000000000000, 0.8660254037844387076, 1.000000000000000000, 0.8660254037844387076, 1.000000000000000000, 0.8660254037844387076, 1.000000000000000000, 0.8660254037844387076, 1.000000000000000000, 0.8660254037844387076, 1.000000000000000000, 0.8660254037844387076, 1.000000000000000000, 0.8660254037844387076, 1.000000000000000000, 0.8660254037844387076, 1.000000000000000000, 0.8660254037844387076, 1.000000000000000000, 0.8660254037844387076, 1.000000000000000000, 0.8660254037844387076, 1.000000000000000000, 0.8660254037844387076, 1.000000000000000000, 0.8660254037844387076, 1.000000000000000000, 0.8660254037844387076, 1.000000000000000000, 0.8660254037844387076, 1.000000000000000000, 0.8660254037844387076, 1.000000000000000000, 0.8660254037844387076, 1.000000000000000000, 0.8660254037844387076, 1.000000000000000000, 0.8660254037844387076, 1.000000000000000000, 0.8660254037844387076, 1.000000000000000000, 0.8660254037844387076, 1.000000000000000000, 0.8660254037844387076, 1.000000000000000000, 0.8660254037844387076, 1.000000000000000000, 0.8660254037844387076, 1.000000000000000000, 0.8660254037844387076, 1.000000000000000000, 0.8660254037844387076, 1.000000000000000000, 0.8660254037844387076, 1.000000000000000000, 0.8660254037844387076, 1.000000000000000000, 0.8660254037844387076, 1.000000000000000000, 0.8660254037844387076, 1.000000000000000000, 0.8660254037844387076, 1.000000000000000000, 0.8660254037844387076, 1.000000000000000000, 0.8660254037844387076, 1.000000000000000000, 0.8660254037844387076, 1.000000000000000000, 0.8660254037844387076, 1.000000000000000000, 0.8660254037844387076, 1.000000000000000000, 0.8660254037844387076, 1.000000000000000000, 0.8660254037844387076, 1.000000000000000000, 0.8660254037844387076, 1.000000000000000000, 0.8660254037844387076, 1.000000000000000000, 0.8660254037844387076, 1.000000000000000000, 0.8660254037844387076, 1.000000000000000000, 0.8660254037844387076, 1.000000000000000000, 0.8660254037844387076, 1.000000000000000000, 0.8660254037844387076, 1.000000000000000000, 0.8660254037844387076, 1.000000000000000000, 0.8660254037844387076, 1.000000000000000000, 0.8660254037844387076, 1.000000000000000000, 0.8660254037844387076, 1.000000000000000000, 0.8660254037844387076, 1.000000000000000000, 0.8660254037844387076, 1.000000000000000000, 0.8660254037844387076, 1.000000000000000000, 0.8660254037844387076, 1.000000000000000000, 0.8660254037844387076, 1.000000000000000000, 0.8660254037844387076, 1.000000000000000000, 0.8660254037844387076, 1.000000000000000000, 0.8660254037844387076, 1.000000000000000000, 0.8660254037844387076, 1.000000000000000000, 0.8660254037844387076, 1.000000000000000000, 0.8660254037844387076, 1.000000000000000000, 0.8660254037844387076, 1.000000000000000000, 0.8660254037844387076, 1.000000000000000000, 0.8660254037844387076, 1.000000000000000000, 0.8660254037844387076, 1.000000000000000000, 0.8660254037844387076, 1.000000000000000000, 0.8660254037844387076, 1.000000000000000000, 0.8660254037844387076, 1.000000000000000000, 0.8660254037844387076, 1.000000000000000000, 0.8660254037844387076, 1.000000000000000000, 0.8660254037844387076, 1.000000000000000000, 0.8660254037844387076, 1.000000000000000000, 0.8660254037844387076, 1.000000000000000000, 0.8660254037844387076, 1.000000000000000000, 0.8660254037844387076, 1.000000000000000000, 0.8660254037844387076, 1.000000000000000000, 0.8660254037844387076, 1.000000000000000000, 0.8660254037844387076, 1.000000000000000000, 0.8660254037844387076, 1.000000000000000000, 0.8660254037844387076, 1.000000000000000000, 0.8660254037844387076, 1.000000000000000000, 0.8660254037844387076, 1.000000000000000000, 0.8660254037844387076, 1.000000000000000000, 0.8660254037844387076, 1.000000000000000000, 0.8660254037844387076, 1.000000000000000000, 0.8660254037844387076, 1.000000000000000000, 0.8660254037844387076, 1.000000000000000000, 0.8660254037844387076, 1.000000000000000000, 0.8660254037844387076, 1.000000000000000000, 0.8660254037844387076, 1.000000000000000000, 0.8660254037844387076, 1.000000000000000000, 0.8660254037844387076, 1.000000000000000000, 0.8660254037844387076, 1.000000000000000000, 0.8660254037844387076, 1.000000000000000000, 0.8660254037844387076, 1.000000000000000000, 0.8660254037844387076, 1.000000000000000000, 0.8660254037844387076, 1.000000000000000000, 0.8660254037844387076, 1.000000000000000000, 0.8660254037844387076, 1.000000000000000000, 0.8660254037844387076, 1.000000000000000000, 0.8660254037844387076, 1.000000000000000000, 0.8660254037844387076, 1.000000000000000000, 0.8660254037844387076, 1.000000000000000000, 0.8660254037844387076, 1.000000000000000000, 0.8660254037844387076, 1.000000000000000000, 0.8660254037844387076, 1.000000000000000000),
 ( 1.000000000000000000, 0.8660254037844387076, 1.000000000000000000, 0.8660254037844387076, 1.000000000000000000, 0.8660254037844387076, 1.000000000000000000, 0.8660254037844387076, 1.000000000000000000, 0.8660254037844387076, 1.000000000000000000, 0.8660254037844387076, 1.000000000000000000, 0.8660254037844387076, 1.000000000000000000, 0.8660254037844387076, 1.000000000000000000, 0.8660254037844387076, 1.000000000000000000, 0.8660254037844387076, 1.000000000000000000, 0.8660254037844387076, 1.000000000000000000, 0.8660254037844387076, 1.000000000000000000, 0.8660254037844387076, 1.000000000000000000, 0.8660254037844387076, 1.000000000000000000, 0.8660254037844387076, 1.000000000000000000, 0.8660254037844387076, 1.000000000000000000, 0.8660254037844387076, 1.000000000000000000, 0.8660254037844387076, 1.000000000000000000, 0.8660254037844387076, 1.000000000000000000, 0.8660254037844387076, 1.000000000000000000, 0.8660254037844387076, 1.000000000000000000, 0.8660254037844387076, 1.000000000000000000, 0.8660254037844387076, 1.000000000000000000, 0.8660254037844387076, 1.000000000000000000, 0.8660254037844387076, 1.000000000000000000, 0.8660254037844387076, 1.000000000000000000, 0.8660254037844387076, 1.000000000000000000, 0.8660254037844387076, 1.000000000000000000, 0.8660254037844387076, 1.000000000000000000, 0.8660254037844387076, 1.000000000000000000, 0.8660254037844387076, 1.000000000000000000, 0.8660254037844387076, 1.000000000000000000, 0.8660254037844387076, 1.000000000000000000, 0.8660254037844387076, 1.000000000000000000, 0.8660254037844387076, 1.000000000000000000, 0.8660254037844387076, 1.000000000000000000, 0.8660254037844387076, 1.000000000000000000, 0.8660254037844387076, 1.000000000000000000, 0.8660254037844387076, 1.000000000000000000, 0.8660254037844387076, 1.000000000000000000, 0.8660254037844387076, 1.000000000000000000, 0.8660254037844387076, 1.000000000000000000, 0.8660254037844387076, 1.000000000000000000, 0.8660254037844387076, 1.000000000000000000, 0.8660254037844387076, 1.000000000000000000, 0.8660254037844387076, 1.000000000000000000, 0.8660254037844387076, 1.000000000000000000, 0.8660254037844387076, 1.000000000000000000, 0.8660254037844387076, 1.000000000000000000, 0.8660254037844387076, 1.000000000000000000, 0.8660254037844387076, 1.000000000000000000, 0.8660254037844387076, 1.000000000000000000, 0.8660254037844387076, 1.000000000000000000, 0.8660254037844387076, 1.000000000000000000, 0.8660254037844387076, 1.000000000000000000, 0.8660254037844387076, 1.000000000000000000, 0.8660254037844387076, 1.000000000000000000, 0.8660254037844387076, 1.000000000000000000, 0.8660254037844387076, 1.000000000000000000, 0.8660254037844387076, 1.000000000000000000, 0.8660254037844387076, 1.000000000000000000, 0.8660254037844387076, 1.000000000000000000, 0.8660254037844387076, 1.000000000000000000, 0.8660254037844387076, 1.000000000000000000, 0.8660254037844387076, 1.000000000000000000, 0.8660254037844387076, 1.000000000000000000, 0.8660254037844387076, 1.000000000000000000, 0.8660254037844387076, 1.000000000000000000, 0.8660254037844387076, 1.000000000000000000, 0.8660254037844387076, 1.000000000000000000, 0.8660254037844387076, 1.000000000000000000, 0.8660254037844387076, 1.000000000000000000, 0.8660254037844387076, 1.000000000000000000, 0.8660254037844387076, 1.000000000000000000, 0.8660254037844387076, 1.000000000000000000, 0.8660254037844387076, 1.000000000000000000, 0.8660254037844387076, 1.000000000000000000, 0.8660254037844387076, 1.000000000000000000, 0.8660254037844387076, 1.000000000000000000, 0.8660254037844387076, 1.000000000000000000, 0.8660254037844387076, 1.000000000000000000, 0.8660254037844387076, 1.000000000000000000, 0.8660254037844387076, 1.000000000000000000, 0.8660254037844387076, 1.000000000000000000, 0.8660254037844387076, 1.000000000000000000, 0.8660254037844387076, 1.000000000000000000, 0.8660254037844387076, 1.000000000000000000, 0.8660254037844387076, 1.000000000000000000, 0.8660254037844387076, 1.000000000000000000, 0.8660254037844387076, 1.000000000000000000, 0.8660254037844387076, 1.000000000000000000, 0.8660254037844387076, 1.000000000000000000, 0.8660254037844387076, 1.000000000000000000, 0.8660254037844387076, 1.000000000000000000, 0.8660254037844387076, 1.000000000000000000, 0.8660254037844387076, 1.000000000000000000, 0.8660254037844387076, 1.000000000000000000, 0.8660254037844387076, 1.000000000000000000, 0.8660254037844387076, 1.000000000000000000, 0.8660254037844387076, 1.000000000000000000, 0.8660254037844387076, 1.000000000000000000, 0.8660254037844387076, 1.000000000000000000, 0.8660254037844387076, 1.000000000000000000, 0.8660254037844387076, 1.000000000000000000, 0.8660254037844387076, 1.000000000000000000, 0.8660254037844387076, 1.000000000000000000, 0.8660254037844387076, 1.000000000000000000, 0.8660254037844387076, 1.000000000000000000, 0.8660254037844387076, 1.000000000000000000, 0.8660254037844387076, 1.000000000000000000, 0.8660254037844387076, 1.000000000000000000, 0.8660254037844387076, 1.000000000000000000, 0.8660254037844387076, 1.000000000000000000, 0.8660254037844387076, 1.000000000000000000, 0.8660254037844387076, 1.000000000000000000, 0.8660254037844387076, 1.000000000000000000, 0.8660254037844387076, 1.000000000000000000, 0.8660254037844387076, 1.000000000000000000, 0.8660254037844387076, 1.000000000000000000, 0.8660254037844387076, 1.000000000000000000, 0.8660254037844387076, 1.000000000000000000, 0.8660254037844387076, 1.000000000000000000, 0.8660254037844387076, 1.000000000000000000, 0.8660254037844387076, 1.000000000000000000, 0.8660254037844387076, 1.000000000000000000, 0.8660254037844387076, 1.000000000000000000, 0.8660254037844387076, 1.000000000000000000, 0.8660254037844387076, 1.000000000000000000, 0.8660254037844387076, 1.000000000000000000, 0.8660254037844387076, 1.000000000000000000, 0.8660254037844387076, 1.000000000000000000, 0.8660254037844387076, 1.000000000000000000, 0.8660254037844387076, 1.000000000000000000, 0.8660254037844387076, 1.000000000000000000, 0.8660254037844387076, 1.000000000000000000, 0.8660254037844387076, 1.000000000000000000, 0.8660254037844387076, 1.000000000000000000, 0.8660254037844387076, 1.000000000000000000, 0.8660254037844387076, 1.000000000000000000, 0.8660254037844387076, 1.000000000000000000, 0.8660254037844387076, 1.000000000000000000, 0.8660254037844387076, 1.000000000000000000, 0.8660254037844387076, 1.000000000000000000, 0.8660254037844387076, 1.000000000000000000, 0.8660254037844387076, 1.000000000000000000, 0.8660254037844387076, 1.000000000000000000, 0.8660254037844387076, 1.000000000000000000, 0.8660254037844387076, 1.000000000000000000, 0.8660254037844387076, 1.000000000000000000, 0.8660254037844387076, 1.000000000000000000, 0.8660254037844387076, 1.000000000000000000, 0.8660254037844387076, 1.000000000000000000, 0.8660254037844387076, 1.000000000000000000, 0.8660254037844387076, 1.000000000000000000, 0.8660254037844387076, 1.000000000000000000, 0.8660254037844387076, 1.000000000000000000, 0.8660254037844387076, 1.000000000000000000, 0.8660254037844387076, 1.000000000000000000, 0.8660254037844387076, 1.000000000000000000, 0.8660254037844387076, 1.000000000000000000, 0.8660254037844387076, 1.000000000000000000, 0.8660254037844387076, 1.000000000000000000, 0.8660254037844387076, 1.000000000000000000, 0.8660254037844387076, 1.000000000000000000, 0.8660254037844387076, 1.000000000000000000, 0.8660254037844387076, 1.000000000000000000, 0.8660254037844387076, 1.000000000000000000, 0.8660254037844387076, 1.000000000000000000, 0.8660254037844387076, 1.000000000000000000, 0.8660254037844387076, 1.000000000000000000, 0.8660254037844387076, 1.000000000000000000, 0.8660254037844387076, 1.000000000000000000, 0.8660254037844387076, 1.000000000000000000, 0.8660254037844387076, 1.000000000000000000, 0.8660254037844387076, 1.000000000000000000, 0.8660254037844387076, 1.000000000000000000, 0.8660254037844387076, 1.000000000000000000, 0.8660254037844387076, 1.000000000000000000, 0.8660254037844387076, 1.000000000000000000, 0.8660254037844387076, 1.000000000000000000, 0.8660254037844387076, 1.000000000000000000, 0.8660254037844387076, 1.000000000000000000, 0.8660254037844387076, 1.000000000000000000, 0.8660254037844387076, 1.000000000000000000, 0.8660254037844387076, 1.000000000000000000, 0.8660254037844387076, 1.000000000000000000, 0.8660254037844387076, 1.000000000000000000, 0.8660254037844387076, 1.000000000000000000, 0.8660254037844387076, 1.000000000000000000, 0.8660254037844387076, 1.000000000000000000, 0.8660254037844387076, 1.000000000000000000, 0.8660254037844387076, 1.000000000000000000, 0.8660254037844387076, 1.000000000000000000, 0.8660254037844387076, 1.000000000000000000, 0.8660254037844387076, 1.000000000000000000, 0.8660254037844387076, 1.000000000000000000, 0.8660254037844387076, 1.000000000000000000, 0.8660254037844387076, 1.000000000000000000, 0.8660254037844387076, 1.000000000000000000, 0.8660254037844387076, 1.000000000000000000, 0.8660254037844387076, 1.000000000000000000, 0.8660254037844387076, 1.000000000000000000, 0.8660254037844387076, 1.000000000000000000, 0.8660254037844387076, 1.000000000000000000, 0.8660254037844387076, 1.000000000000000000, 0.8660254037844387076, 1.000000000000000000, 0.8660254037844387076, 1.000000000000000000, 0.8660254037844387076, 1.000000000000000000, 0.8660254037844387076, 1.000000000000000000, 0.8660254037844387076, 1.000000000000000000, 0.8660254037844387076, 1.000000000000000000, 0.8660254037844387076, 1.000000000000000000, 0.8660254037844387076, 1.000000000000000000, 0.8660254037844387076, 1.000000000000000000, 0.8660254037844387076, 1.000000000000000000, 0.8660254037844387076, 1.000000000000000000, 0.8660254037844387076, 1.000000000000000000, 0.8660254037844387076, 1.000000000000000000, 0.8660254037844387076, 1.000000000000000000, 0.8660254037844387076, 1.000000000000000000, 0.8660254037844387076, 1.000000000000000000, 0.8660254037844387076, 1.000000000000000000, 0.8660254037844387076, 1.000000000000000000, 0.8660254037844387076, 1.000000000000000000, 0.8660254037844387076, 1.000000000000000000, 0.8660254037844387076, 1.000000000000000000, 0.8660254037844387076, 1.000000000000000000, 0.8660254037844387076, 1.000000000000000000, 0.8660254037844387076, 1.000000000000000000, 0.8660254037844387076, 1.000000000000000000, 0.8660254037844387076, 1.000000000000000000, 0.8660254037844387076, 1.000000000000000000, 0.8660254037844387076, 1.000000000000000000, 0.8660254037844387076, 1.000000000000000000, 0.8660254037844387076, 1.000000000000000000, 0.8660254037844387076, 1.000000000000000000, 0.8660254037844387076, 1.000000000000000000, 0.8660254037844387076, 1.000000000000000000, 0.8660254037844387076, 1.000000000000000000, 0.8660254037844387076, 1.000000000000000000, 0.8660254037844387076, 1.000000000000000000, 0.8660254037844387076, 1.000000000000000000, 0.8660254037844387076, 1.000000000000000000, 0.8660254037844387076, 1.000000000000000000, 0.8660254037844387076, 1.000000000000000000, 0.8660254037844387076, 1.000000000000000000, 0.8660254037844387076, 1.000000000000000000, 0.8660254037844387076, 1.000000000000000000, 0.8660254037844387076, 1.000000000000000000, 0.8660254037844387076, 1.000000000000000000, 0.8660254037844387076, 1.000000000000000000, 0.8660254037844387076, 1.000000000000000000, 0.8660254037844387076, 1.000000000000000000, 0.8660254037844387076, 1.000000000000000000, 0.8660254037844387076, 1.000000000000000000, 0.8660254037844387076, 1.000000000000000000, 0.8660254037844387076, 1.000000000000000000, 0.8660254037844387076, 1.000000000000000000, 0.8660254037844387076, 1.000000000000000000, 0.8660254037844387076, 1.000000000000000000, 0.8660254037844387076, 1.000000000000000000, 0.8660254037844387076, 1.000000000000000000, 0.8660254037844387076, 1.000000000000000000, 0.8660254037844387076, 1.000000000000000000, 0.8660254037844387076, 1.000000000000000000, 0.8660254037844387076, 1.000000000000000000, 0.8660254037844387076, 1.000000000000000000, 0.8660254037844387076, 1.000000000000000000, 0.8660254037844387076, 1.000000000000000000, 0.8660254037844387076, 1.000000000000000000, 0.8660254037844387076, 1.000000000000000000, 0.8660254037844387076, 1.000000000000000000, 0.8660254037844387076, 1.000000000000000000, 0.8660254037844387076, 1.000000000000000000, 0.8660254037844387076, 1.000000000000000000, 0.8660254037844387076, 1.000000000000000000, 0.8660254037844387076, 1.000000000000000000, 0.8660254037844387076, 1.000000000000000000, 0.8660254037844387076, 1.000000000000000000, 0.8660254037844387076, 1.000000000000000000, 0.8660254037844387076, 1.000000000000000000, 0.8660254037844387076, 1.000000000000000000, 0.8660254037844387076, 1.000000000000000000, 0.8660254037844387076, 1.000000000000000000, 0.8660254037844387076, 1.000000000000000000, 0.8660254037844387076, 1.000000000000000000, 0.8660254037844387076, 1.000000000000000000, 0.8660254037844387076, 1.000000000000000000, 0.8660254037844387076, 1.000000000000000000, 0.8660254037844387076, 1.000000000000000000, 0.8660254037844387076, 1.000000000000000000, 0.8660254037844387076, 1.000000000000000000, 0.8660254037844387076, 1.000000000000000000, 0.8660254037844387076, 1.000000000000000000, 0.8660254037844387076, 1.000000000000000000, 0.8660254037844387076, 1.000000000000000000, 0.8660254037844387076, 1.000000000000000000, 0.8660254037844387076, 1.000000000000000000, 0.8660254037844387076, 1.000000000000000000, 0.8660254037844387076, 1.000000000000000000, 0.8660254037844387076, 1.000000000000000000, 0.8660254037844387076, 1.000000000000000000, 0.8660254037844387076, 1.000000000000000000, 0.8660254037844387076, 1.000000000000000000, 0.8660254037844387076, 1.000000000000000000, 0.8660254037844387076, 1.000000000000000000, 0.8660254037844387076, 1.000000000000000000, 0.8660254037844387076, 1.000000000000000000, 0.8660254037844387076, 1.000000000000000000, 0.8660254037844387076, 1.000000000000000000, 0.8660254037844387076, 1.000000000000000000, 0.8660254037844387076, 1.000000000000000000, 0.8660254037844387076, 1.000000000000000000, 0.8660254037844387076, 1.000000000000000000, 0.8660254037844387076, 1.000000000000000000, 0.8660254037844387076, 1.000000000000000000, 0.8660254037844387076, 1.000000000000000000, 0.8660254037844387076, 1.000000000000000000, 0.8660254037844387076, 1.000000000000000000, 0.8660254037844387076, 1.000000000000000000, 0.8660254037844387076, 1.000000000000000000, 0.8660254037844387076, 1.000000000000000000, 0.8660254037844387076, 1.000000000000000000, 0.8660254037844387076, 1.000000000000000000, 0.8660254037844387076, 1.000000000000000000, 0.8660254037844387076, 1.000000000000000000, 0.8660254037844387076, 1.000000000000000000, 0.8660254037844387076, 1.000000000000000000, 0.8660254037844387076, 1.000000000000000000, 0.8660254037844387076, 1.000000000000000000, 0.8660254037844387076, 1.000000000000000000, 0.8660254037844387076, 1.000000000000000000, 0.8660254037844387076, 1.000000000000000000, 0.8660254037844387076, 1.000000000000000000, 0.8660254037844387076, 1.000000000000000000, 0.8660254037844387076, 1.000000000000000000, 0.8660254037844387076, 1.000000000000000000, 0.8660254037844387076, 1.000000000000000000, 0.8660254037844387076, 1.000000000000000000, 0.8660254037844387076, 1.000000000000000000, 0.8660254037844387076, 1.000000000000000000, 0.8660254037844387076, 1.000000000000000000, 0.8660254037844387076, 1.000000000000000000, 0.8660254037844387076, 1.000000000000000000, 0.8660254037844387076, 1.000000000000000000, 0.8660254037844387076, 1.000000000000000000, 0.8660254037844387076, 1.000000000000000000, 0.8660254037844387076, 1.000000000000000000, 0.8660254037844387076, 1.000000000000000000, 0.8660254037844387076, 1.000000000000000000, 0.8660254037844387076, 1.000000000000000000, 0.8660254037844387076, 1.000000000000000000, 0.8660254037844387076, 1.000000000000000000, 0.8660254037844387076, 1.000000000000000000, 0.8660254037844387076, 1.000000000000000000, 0.8660254037844387076, 1.000000000000000000, 0.8660254037844387076, 1.000000000000000000, 0.8660254037844387076, 1.000000000000000000, 0.8660254037844387076, 1.000000000000000000, 0.8660254037844387076, 1.000000000000000000) ) ) 
 REPRESENTATION_ITEM ( '' )  SURFACE ( )  );
#71033 = CARTESIAN_POINT ( 'NONE',  ( 28.61249999999999716, 2.886751345948126879, 4.999999999999999112 ) ) ;
#71034 = CARTESIAN_POINT ( 'NONE',  ( 11.12812500061451715, 6.421520780324663323E-16, -5.243569643749999010 ) ) ;
#71035 = CARTESIAN_POINT ( 'NONE',  ( 29.59687500061451360, 4.119189519843966529, -2.378215178124998275 ) ) ;
#71036 = CARTESIAN_POINT ( 'NONE',  ( 24.68437500061451573, 6.421520780324663323E-16, -5.243569643749999010 ) ) ;
#71037 = CARTESIAN_POINT ( 'NONE',  ( 16.80937500061451573, -5.492252693125287522, -1.008910452111647106E-15 ) ) ;
#71038 = CARTESIAN_POINT ( 'NONE',  ( 7.828125000614517326, -4.541064518000419881, 2.621784821874995952 ) ) ;
#71039 = CARTESIAN_POINT ( 'NONE',  ( 12.42187500061451821, -6.054752690667223547, -1.112240025338166033E-15 ) ) ;
#71040 = VERTEX_POINT ( 'NONE', #31634 ) ;
#71041 = CARTESIAN_POINT ( 'NONE',  ( 23.10937500061451644, 0.000000000000000000, 5.243569643749999010 ) ) ;
#71042 = CARTESIAN_POINT ( 'NONE',  ( 27.36562500061451786, 3.027376345333613106, -5.243569643749998122 ) ) ;
#71043 = PLANE ( 'NONE',  #14832 ) ;
#71044 = CARTESIAN_POINT ( 'NONE',  ( 7.124999999999999112, -4.330127018922194537, 2.499999999999995559 ) ) ;
#71045 = CARTESIAN_POINT ( 'NONE',  ( 15.90000000122903501, -2.886751345948125991, -5.000000000000000000 ) ) ;
#71046 = CARTESIAN_POINT ( 'NONE',  ( -2.000000000000000000, 17.78750000122903430, -33.46410161513775705 ) ) ;
#71047 = CARTESIAN_POINT ( 'NONE',  ( 7.396875000614516082, -4.119189519843965641, -2.378215178125001383 ) ) ;
#71048 = EDGE_LOOP ( 'NONE', ( #54295, #52949, #67727, #1632 ) ) ;
#71049 = CARTESIAN_POINT ( 'NONE',  ( 15.26249999999999929, -5.773502691896255534, -1.060575238724906372E-15 ) ) ;
#71050 = CARTESIAN_POINT ( 'NONE',  ( 18.18750000000000000, 5.773502691896255534, 3.535250795749688894E-16 ) ) ;
#71051 = CARTESIAN_POINT ( 'NONE',  ( 11.05312500061451608, -4.541064518000417216, -2.621784821875001281 ) ) ;
#71052 = ORIENTED_EDGE ( 'NONE', *, *, #37057, .F. ) ;
#71053 = DIRECTION ( 'NONE',  ( 0.000000000000000000, -1.000000000000000000, 8.673617379884035472E-17 ) ) ;
#71054 = CARTESIAN_POINT ( 'NONE',  ( 2.121784821874999061, 17.90937500061451715, -33.67503911421598417 ) ) ;
#71055 = CARTESIAN_POINT ( 'NONE',  ( 3.290625000614516793, -3.027376345333614438, 5.243569643749998122 ) ) ;
#71056 = CARTESIAN_POINT ( 'NONE',  ( 10.42500000000000071, 6.123233995736764310E-16, -4.999999999999998224 ) ) ;
#71057 = CARTESIAN_POINT ( 'NONE',  ( 9.187500000000001776, 5.773502691896255534, 3.535250795749688894E-16 ) ) ;
#71058 = CARTESIAN_POINT ( 'NONE',  ( 3.850967645426020436, 3.886246437104829088, -3.268823720200904503 ) ) ;
#71059 = ORIENTED_EDGE ( 'NONE', *, *, #18452, .F. ) ;
#71060 = CARTESIAN_POINT ( 'NONE',  ( -4.243569643749999898, 15.71562500061451573, 27.54997392385601529 ) ) ;
#71061 = CARTESIAN_POINT ( 'NONE',  ( 26.01562500061451289, 3.027376345333613106, -5.243569643749998122 ) ) ;
#71062 = CARTESIAN_POINT ( 'NONE',  ( 8.925000000000002487, -4.330127018922194537, 2.499999999999995559 ) ) ;
#71063 = FACE_OUTER_BOUND ( 'NONE', #27755, .T. ) ;
#71064 = CARTESIAN_POINT ( 'NONE',  ( 23.70937500061451786, -4.541064518000417216, -2.621784821875001281 ) ) ;
#71065 = CARTESIAN_POINT ( 'NONE',  ( 17.95312500061451644, 4.541064518000418104, -2.621784821874998173 ) ) ;
#71066 = CARTESIAN_POINT ( 'NONE',  ( -3.000416591977282496E-16, 12.94062500061459176, -34.90005215228797653 ) ) ;
#71067 = CARTESIAN_POINT ( 'NONE',  ( 23.06250000122903288, -4.330127018922190985, -2.500000000000001332 ) ) ;
#71068 = CARTESIAN_POINT ( 'NONE',  ( 3.665625000614517681, 3.027376345333611329, 5.243569643749999010 ) ) ;
#71069 = CARTESIAN_POINT ( 'NONE',  ( 27.75937500061451502, -4.119189519843965641, -2.378215178125001383 ) ) ;
#71070 = CARTESIAN_POINT ( 'NONE',  ( 22.00312500061451360, 4.541064518000418104, -2.621784821874998173 ) ) ;
#71071 = CARTESIAN_POINT ( 'NONE',  ( 7.359375000614516438, 0.000000000000000000, 4.756430356249998326 ) ) ;
#71072 = CARTESIAN_POINT ( 'NONE',  ( 3.756430356250000546, 16.72812499938548214, 27.83122392262697886 ) ) ;
#71073 = CARTESIAN_POINT ( 'NONE',  ( 16.39687500061451786, -3.027376345333614438, 5.243569643749998122 ) ) ;
#71074 = CARTESIAN_POINT ( 'NONE',  ( 16.47187500061452070, -6.054752690667223547, -1.112240025338166033E-15 ) ) ;
#71075 = CARTESIAN_POINT ( 'NONE',  ( 25.50937500061451502, -4.541064518000417216, -2.621784821875001281 ) ) ;
#71076 = CARTESIAN_POINT ( 'NONE',  ( 4.243569643749999010, 15.17187500061451644, 27.54997392385601174 ) ) ;
#71077 = CARTESIAN_POINT ( 'NONE',  ( 4.678125000614516971, -4.541064518000419881, 2.621784821874995952 ) ) ;
#71078 = CARTESIAN_POINT ( 'NONE',  ( 29.12812500061451715, 6.421520780324663323E-16, -5.243569643749999010 ) ) ;
#71079 = CARTESIAN_POINT ( 'NONE',  ( 28.86562500061451786, 3.027376345333611329, 5.243569643749999010 ) ) ;
#71080 = CARTESIAN_POINT ( 'NONE',  ( 1.999999999999998668, 16.36250000122903359, -33.46410161513775705 ) ) ;
#71081 = CARTESIAN_POINT ( 'NONE',  ( -1.999999999999997113, 19.62500000000000000, 33.46410161513775705 ) ) ;
#71082 = CARTESIAN_POINT ( 'NONE',  ( 8.184375000614515727, 4.541064518000418104, 2.621784821874999949 ) ) ;
#71083 = CARTESIAN_POINT ( 'NONE',  ( 14.13750000122903394, 6.123233995736764310E-16, -4.999999999999998224 ) ) ;
#71084 = CARTESIAN_POINT ( 'NONE',  ( 8.737500001229033586, 6.123233995736764310E-16, -4.999999999999998224 ) ) ;
#71085 = CARTESIAN_POINT ( 'NONE',  ( 6.178125000614518747, 6.421520780324663323E-16, -5.243569643749999010 ) ) ;
#71086 = CARTESIAN_POINT ( 'NONE',  ( -4.000000000000000888, 17.20624999877096428, 32.30940107675850470 ) ) ;
#71087 = CARTESIAN_POINT ( 'NONE',  ( 22.03125000122903288, -4.330127018922194537, 2.499999999999995559 ) ) ;
#71088 = CARTESIAN_POINT ( 'NONE',  ( 15.38437500061451679, 4.541064518000418104, 2.621784821874999949 ) ) ;
#71089 = CARTESIAN_POINT ( 'NONE',  ( 7.724999999999999645, 6.123233995736764310E-16, -4.999999999999998224 ) ) ;
#71090 = ORIENTED_EDGE ( 'NONE', *, *, #19403, .F. ) ;
#71091 = CARTESIAN_POINT ( 'NONE',  ( 21.85312500061451502, -4.541064518000417216, -2.621784821875001281 ) ) ;
#71092 = CARTESIAN_POINT ( 'NONE',  ( 7.865625000614516971, -6.054752690667223547, -1.112240025338166033E-15 ) ) ;
#71093 = CARTESIAN_POINT ( 'NONE',  ( 24.64687500061451431, -3.027376345333610441, -5.243569643749999898 ) ) ;
#71094 = CARTESIAN_POINT ( 'NONE',  ( 8.390625000614518214, -3.027376345333610441, -5.243569643749999898 ) ) ;
#71095 = CARTESIAN_POINT ( 'NONE',  ( 7.931250001229031454, 4.330127018922191873, 2.499999999999999556 ) ) ;
#71096 = CARTESIAN_POINT ( 'NONE',  ( 7.650000001229034119, -2.886751345948129988, 4.999999999999997335 ) ) ;
#71097 =( BOUNDED_CURVE ( )  B_SPLINE_CURVE ( 2, ( #12250, #34781, #57314, #29251, #40702, #47683, #2621 ),
 .UNSPECIFIED., .F., .F. ) 
 B_SPLINE_CURVE_WITH_KNOTS ( ( 3, 2, 2, 3 ),
 ( 0.5833333333333334814, 0.5861111111111112493, 0.5888888888888890172, 0.5916666666666667851 ),
 .UNSPECIFIED. ) 
 CURVE ( )  GEOMETRIC_REPRESENTATION_ITEM ( )  RATIONAL_B_SPLINE_CURVE ( ( 0.9999999999999946709, 0.8660254037844440367, 1.000000000000000000, 0.8660254037844387076, 1.000000000000000000, 0.8660254037844333785, 1.000000000000005329 ) ) 
 REPRESENTATION_ITEM ( '' )  );
#71098 = CARTESIAN_POINT ( 'NONE',  ( 23.05312500061451431, 0.000000000000000000, 5.243569643749999010 ) ) ;
#71099 = VECTOR ( 'NONE', #29987, 1000.000000000000000 ) ;
#71100 = CARTESIAN_POINT ( 'NONE',  ( 2.121784821874999061, 11.10312500061451679, -33.67503911421598417 ) ) ;
#71101 = CARTESIAN_POINT ( 'NONE',  ( 9.412500001229034297, 0.000000000000000000, 4.999999999999998224 ) ) ;
#71102 = CARTESIAN_POINT ( 'NONE',  ( 19.11562500061451431, -6.054752690667223547, -1.112240025338166033E-15 ) ) ;
#71103 = CARTESIAN_POINT ( 'NONE',  ( 16.97812500061451502, 6.421520780324663323E-16, -5.243569643749999010 ) ) ;
#71104 = CARTESIAN_POINT ( 'NONE',  ( 28.35937500061451289, 4.119189519843966529, -2.378215178124998275 ) ) ;
#71105 = CARTESIAN_POINT ( 'NONE',  ( 18.07499999999999929, 6.123233995736764310E-16, -4.999999999999998224 ) ) ;
#71106 = CARTESIAN_POINT ( 'NONE',  ( 10.53750000122903252, 6.123233995736764310E-16, -4.999999999999998224 ) ) ;
#71107 = CARTESIAN_POINT ( 'NONE',  ( 8.728125000614518569, -4.541064518000419881, 2.621784821874995952 ) ) ;
#71108 = CARTESIAN_POINT ( 'NONE',  ( 13.11562500061451786, 3.027376345333611329, 5.243569643749999010 ) ) ;
#71109 = EDGE_CURVE ( 'NONE', #27542, #40431, #35841, .T. ) ;
#71110 = CARTESIAN_POINT ( 'NONE',  ( 23.73750000122903359, 4.330127018922191873, 2.499999999999999556 ) ) ;
#71111 = CARTESIAN_POINT ( 'NONE',  ( 22.77187500061451786, -6.054752690667223547, -1.112240025338166033E-15 ) ) ;
#71112 = CARTESIAN_POINT ( 'NONE',  ( 21.95625000122903003, 0.000000000000000000, 4.999999999999998224 ) ) ;
#71113 = CARTESIAN_POINT ( 'NONE',  ( 6.000000001229033764, -2.886751345948125991, -5.000000000000000000 ) ) ;
#71114 = CARTESIAN_POINT ( 'NONE',  ( 6.046875000614519102, -3.027376345333614438, 5.243569643749998122 ) ) ;
#71115 = CARTESIAN_POINT ( 'NONE',  ( 22.69687500061451857, -3.027376345333614438, 5.243569643749998122 ) ) ;
#71116 = CARTESIAN_POINT ( 'NONE',  ( 4.492467025342753217, 2.195141042190226877, -4.710191972078852984 ) ) ;
#71117 = CARTESIAN_POINT ( 'NONE',  ( 19.52812500061451573, -4.541064518000419881, 2.621784821874995952 ) ) ;
#71118 = CARTESIAN_POINT ( 'NONE',  ( 25.13437500061451502, 6.421520780324663323E-16, -5.243569643749999010 ) ) ;
#71119 = CARTESIAN_POINT ( 'NONE',  ( 2.655984681222220721E-16, 20.51562499938548356, 25.66244784525396483 ) ) ;
#71120 = CARTESIAN_POINT ( 'NONE',  ( 30.00000000000000000, 0.000000000000000000, 0.000000000000000000 ) ) ;
#71121 = CARTESIAN_POINT ( 'NONE',  ( 16.51875000122903003, 2.886751345948182834, 4.999999999999902300 ) ) ;
#71122 = CARTESIAN_POINT ( 'NONE',  ( 5.784375000614517148, 6.421520780324663323E-16, -5.243569643749999010 ) ) ;
#71123 = CARTESIAN_POINT ( 'NONE',  ( 14.99062500061451786, -3.027376345333614438, 5.243569643749998122 ) ) ;
#71124 = CARTESIAN_POINT ( 'NONE',  ( 14.18437500061451750, -4.541064518000419881, 2.621784821874995952 ) ) ;
#71125 = ORIENTED_EDGE ( 'NONE', *, *, #36482, .F. ) ;
#71126 = CARTESIAN_POINT ( 'NONE',  ( 24.51562500061451289, -6.054752690667223547, -1.112240025338166033E-15 ) ) ;
#71127 = LINE ( 'NONE', #71869, #3878 ) ;
#71128 = CARTESIAN_POINT ( 'NONE',  ( -1.071796769724502107, 20.28259618943232923, 26.00000000000000711 ) ) ;
#71129 = CARTESIAN_POINT ( 'NONE',  ( 15.82499999999999929, 6.123233995736764310E-16, -4.999999999999998224 ) ) ;
#71130 = CARTESIAN_POINT ( 'NONE',  ( 23.51250000122903216, -4.330127018922190985, -2.500000000000001332 ) ) ;
#71131 = CARTESIAN_POINT ( 'NONE',  ( 17.39062500061451644, -3.027376345333610441, -5.243569643749999898 ) ) ;
#71132 = VERTEX_POINT ( 'NONE', #10193 ) ;
#71133 = CARTESIAN_POINT ( 'NONE',  ( 22.87500000000000000, -4.330127018922194537, 2.499999999999995559 ) ) ;
#71134 = CARTESIAN_POINT ( 'NONE',  ( 24.08437500061451786, -4.541064518000419881, 2.621784821874995952 ) ) ;
#71135 = VERTEX_POINT ( 'NONE', #60054 ) ;
#71136 = CARTESIAN_POINT ( 'NONE',  ( 13.23750000122903359, 6.123233995736764310E-16, -4.999999999999998224 ) ) ;
#71137 = CARTESIAN_POINT ( 'NONE',  ( 11.09062500061451573, -3.027376345333610441, -5.243569643749999898 ) ) ;
#71138 = CARTESIAN_POINT ( 'NONE',  ( 4.378125000614518925, 6.421520780324663323E-16, -5.243569643749999010 ) ) ;
#71139 = CARTESIAN_POINT ( 'NONE',  ( 15.19687500061451502, 4.119189519843966529, -2.378215178124998275 ) ) ;
#71140 = CARTESIAN_POINT ( 'NONE',  ( 27.77812500061451573, 6.421520780324663323E-16, -5.243569643749999010 ) ) ;
#71141 = CARTESIAN_POINT ( 'NONE',  ( 18.37500000000000355, -4.330127018922194537, 2.499999999999995559 ) ) ;
#71142 = CARTESIAN_POINT ( 'NONE',  ( 27.41250000000000142, -5.773502691896255534, -1.060575238724906372E-15 ) ) ;
#71143 = CARTESIAN_POINT ( 'NONE',  ( 45.00000000000000000, 6.123233995736764310E-16, -4.999999999999998224 ) ) ;
#71144 = CARTESIAN_POINT ( 'NONE',  ( 6.871875000614517504, 3.027376345333611329, 5.243569643749999010 ) ) ;
#71145 = CARTESIAN_POINT ( 'NONE',  ( 17.44687500061451857, -3.027376345333610441, -5.243569643749999898 ) ) ;
#71146 = CYLINDRICAL_SURFACE ( 'NONE', #25385, 4.999999999999998224 ) ;
#71147 = VERTEX_POINT ( 'NONE', #43818 ) ;
#71148 = CARTESIAN_POINT ( 'NONE',  ( 26.31562500061451715, -6.054752690667223547, -1.112240025338166033E-15 ) ) ;
#71149 = CARTESIAN_POINT ( 'NONE',  ( 27.04687500061451644, 6.054752690667223547, 3.707466751127219781E-16 ) ) ;
#71150 = DIRECTION ( 'NONE',  ( -1.000000000000000000, -0.000000000000000000, -0.000000000000000000 ) ) ;
#71151 = CARTESIAN_POINT ( 'NONE',  ( 12.93750000000000178, -2.886751345948129988, 4.999999999999997335 ) ) ;
#71152 = CARTESIAN_POINT ( 'NONE',  ( 11.39062500061451644, -3.027376345333614438, 5.243569643749998122 ) ) ;
#71153 = CARTESIAN_POINT ( 'NONE',  ( 1.071796769724479237, 18.44240381056765798, 25.99999999999999645 ) ) ;
#71154 = CARTESIAN_POINT ( 'NONE',  ( -1.071796769724492115, 18.16115380933862866, 34.00000000000000000 ) ) ;
#71155 = CARTESIAN_POINT ( 'NONE',  ( 29.80312500061451431, 0.000000000000000000, 5.243569643749999010 ) ) ;
#71156 = CARTESIAN_POINT ( 'NONE',  ( 18.63750000122903216, 6.123233995736764310E-16, -4.999999999999998224 ) ) ;
#71157 = CARTESIAN_POINT ( 'NONE',  ( 0.000000000000000000, 27.50000000000000000, 26.00000000000000000 ) ) ;
#71158 = CARTESIAN_POINT ( 'NONE',  ( 16.80937500061451573, 0.000000000000000000, 4.756430356249998326 ) ) ;
#71159 = CARTESIAN_POINT ( 'NONE',  ( 4.865625000614517859, 3.027376345333613106, -5.243569643749998122 ) ) ;
#71160 = CARTESIAN_POINT ( 'NONE',  ( 21.30937500061451573, 0.000000000000000000, 5.243569643749999010 ) ) ;
#71161 = CARTESIAN_POINT ( 'NONE',  ( -4.243569643749999898, 17.60937500061451999, 30.00000000000000000 ) ) ;
#71162 = CARTESIAN_POINT ( 'NONE',  ( 23.44687500061451502, 6.054752690667223547, 3.707466751127219781E-16 ) ) ;
#71163 = CARTESIAN_POINT ( 'NONE',  ( 4.425000000000001599, -4.330127018922194537, 2.499999999999995559 ) ) ;
#71164 = CARTESIAN_POINT ( 'NONE',  ( -3.999999999999999556, 11.07500000122903394, 27.69059892324149530 ) ) ;
#71165 = CARTESIAN_POINT ( 'NONE',  ( 11.57812500061451644, 6.421520780324663323E-16, -5.243569643749999010 ) ) ;
#71166 = CARTESIAN_POINT ( 'NONE',  ( 3.525000001229034119, 2.886751345948126879, 4.999999999999999112 ) ) ;
#71167 = EDGE_CURVE ( 'NONE', #15981, #16013, #65976, .T. ) ;
#71168 = CARTESIAN_POINT ( 'NONE',  ( 10.39687500061451786, 6.054752690667223547, 3.707466751127219781E-16 ) ) ;
#71169 = CARTESIAN_POINT ( 'NONE',  ( 1.592000809091587073E-14, 15.05000000122903714, 26.00000000000000000 ) ) ;
#71170 = CARTESIAN_POINT ( 'NONE',  ( 9.515625000614518214, 3.027376345333611329, 5.243569643749999010 ) ) ;
#71171 = CARTESIAN_POINT ( 'NONE',  ( 13.77187500061451786, -6.054752690667223547, -1.112240025338166033E-15 ) ) ;
#71172 = CARTESIAN_POINT ( 'NONE',  ( 21.50625000122903074, 0.000000000000000000, 4.999999999999998224 ) ) ;
#71173 = CARTESIAN_POINT ( 'NONE',  ( 20.66250000122903074, 0.000000000000000000, 4.999999999999998224 ) ) ;
#71174 = CARTESIAN_POINT ( 'NONE',  ( 10.20937500061451786, -4.541064518000417216, -2.621784821875001281 ) ) ;
#71175 = CARTESIAN_POINT ( 'NONE',  ( 12.47812500061451502, 6.421520780324663323E-16, -5.243569643749999010 ) ) ;
#71176 = CARTESIAN_POINT ( 'NONE',  ( 28.78125000122903288, -4.330127018922194537, 2.499999999999995559 ) ) ;
#71177 = CARTESIAN_POINT ( 'NONE',  ( 20.40937500061451715, 0.000000000000000000, 5.243569643749999010 ) ) ;
#71178 = CYLINDRICAL_SURFACE ( 'NONE', #45521, 4.999999999999998224 ) ;
#71179 = CARTESIAN_POINT ( 'NONE',  ( -2.506492529888153964, 4.347006505069262339, 26.84353589692258879 ) ) ;
#71180 = CARTESIAN_POINT ( 'NONE',  ( 2.964777361493091679, -4.026176250088806086, -3.359304602455296607 ) ) ;
#71181 = CARTESIAN_POINT ( 'NONE',  ( -4.243569643749999898, 14.90937500061451715, -30.00000000000000000 ) ) ;
#71182 = CARTESIAN_POINT ( 'NONE',  ( 15.56250000122903465, 4.330127018922192761, -2.499999999999997780 ) ) ;
#71183 = CARTESIAN_POINT ( 'NONE',  ( 10.20937500061451786, -4.541064518000417216, -2.621784821875001281 ) ) ;
#71184 = CARTESIAN_POINT ( 'NONE',  ( -4.243569643749999898, 17.96562500061451573, -32.45002607614398471 ) ) ;
#71185 = CARTESIAN_POINT ( 'NONE',  ( 18.41250000122903430, 0.000000000000000000, 4.999999999999998224 ) ) ;
#71186 = CARTESIAN_POINT ( 'NONE',  ( 9.440625000614517148, 6.054752690667223547, 3.707466751127219781E-16 ) ) ;
#71187 = ORIENTED_EDGE ( 'NONE', *, *, #32834, .T. ) ;
#71188 = CARTESIAN_POINT ( 'NONE',  ( 15.97499999999999964, 4.330127018922191873, 2.499999999999999556 ) ) ;
#71189 = CARTESIAN_POINT ( 'NONE',  ( 4.987500001229032698, -4.330127018922194537, 2.499999999999995559 ) ) ;
#71190 = CARTESIAN_POINT ( 'NONE',  ( 9.309375000614517504, -4.541064518000417216, -2.621784821875001281 ) ) ;
#71191 = EDGE_CURVE ( 'NONE', #38944, #1656, #50961, .T. ) ;
#71192 = CARTESIAN_POINT ( 'NONE',  ( 5.137500001229033941, 6.123233995736764310E-16, -4.999999999999998224 ) ) ;
#71193 = CARTESIAN_POINT ( 'NONE',  ( 10.95000000122903394, -2.886751345948125991, -5.000000000000000000 ) ) ;
#71194 = CARTESIAN_POINT ( 'NONE',  ( 17.81250000122903288, 4.330127018922192761, -2.499999999999997780 ) ) ;
#71195 = CARTESIAN_POINT ( 'NONE',  ( 14.16562500061451679, -6.054752690667223547, -1.112240025338166033E-15 ) ) ;
#71196 = CARTESIAN_POINT ( 'NONE',  ( 21.10312500061451502, 4.541064518000418104, -2.621784821874998173 ) ) ;
#71197 = CARTESIAN_POINT ( 'NONE',  ( 27.82500000122903572, 2.886751345948126879, 4.999999999999999112 ) ) ;
#71198 = CARTESIAN_POINT ( 'NONE',  ( 3.253125000614518036, 0.000000000000000000, 5.243569643749999010 ) ) ;
#71199 = CARTESIAN_POINT ( 'NONE',  ( 24.44999999999999929, 4.330127018922192761, -2.499999999999997780 ) ) ;
#71200 = CARTESIAN_POINT ( 'NONE',  ( 4.898587196589411843E-16, 20.00000000000000000, 33.99999999999999289 ) ) ;
#71201 = CARTESIAN_POINT ( 'NONE',  ( 27.18750000000000000, 5.773502691896255534, 3.535250795749688894E-16 ) ) ;
#71202 = CARTESIAN_POINT ( 'NONE',  ( 29.25937500061451502, 4.541064518000418104, -2.621784821874998173 ) ) ;
#71203 = CARTESIAN_POINT ( 'NONE',  ( 26.49375000122903145, -2.886751345948130876, 4.999999999999996447 ) ) ;
#71204 = CARTESIAN_POINT ( 'NONE',  ( 13.01250000122903394, 0.000000000000000000, 4.999999999999998224 ) ) ;
#71205 = CARTESIAN_POINT ( 'NONE',  ( 29.25937500061451502, 4.541064518000418104, -2.621784821874998173 ) ) ;
#71206 = ADVANCED_FACE ( 'NONE', ( #71525 ), #15720, .F. ) ;
#71207 = CARTESIAN_POINT ( 'NONE',  ( 8.109375000614518214, 4.541064518000418104, -2.621784821874998173 ) ) ;
#71208 = CARTESIAN_POINT ( 'NONE',  ( 26.76562500061451644, -6.054752690667223547, -1.112240025338166033E-15 ) ) ;
#71209 = CARTESIAN_POINT ( 'NONE',  ( -3.756430356250000102, 13.42812499938548321, 30.00000000000000000 ) ) ;
#71210 = CARTESIAN_POINT ( 'NONE',  ( 11.58750000122903501, 4.330127018922191873, 2.499999999999999556 ) ) ;
#71211 = CARTESIAN_POINT ( 'NONE',  ( 3.752440054025286909, -3.304420318444254878, 4.071342403668507082 ) ) ;
#71212 = CARTESIAN_POINT ( 'NONE',  ( 6.534375000614517148, -4.541064518000419881, 2.621784821874995952 ) ) ;
#71213 = CARTESIAN_POINT ( 'NONE',  ( 8.371875000614515727, -6.054752690667223547, -1.112240025338166033E-15 ) ) ;
#71214 = CARTESIAN_POINT ( 'NONE',  ( 3.000000000000002665, 0.000000000000000000, 4.999999999999998224 ) ) ;
#71215 = CARTESIAN_POINT ( 'NONE',  ( 4.243569643749999010, 13.31562500061459353, 27.54997392385601174 ) ) ;
#71216 = CARTESIAN_POINT ( 'NONE',  ( 22.94999999999999929, -4.330127018922190985, -2.500000000000001332 ) ) ;
#71217 = CARTESIAN_POINT ( 'NONE',  ( 29.69999999999999574, -4.330127018922190985, -2.500000000000001332 ) ) ;
#71218 = CARTESIAN_POINT ( 'NONE',  ( 4.500000000000000888, -4.330127018922190985, -2.500000000000001332 ) ) ;
#71219 = CARTESIAN_POINT ( 'NONE',  ( 12.72187500061451537, -4.119189519843968306, 2.378215178124996054 ) ) ;
#71220 = VERTEX_POINT ( 'NONE', #33445 ) ;
#71221 = CARTESIAN_POINT ( 'NONE',  ( 18.70312500061451644, -4.541064518000417216, -2.621784821875001281 ) ) ;
#71222 = CARTESIAN_POINT ( 'NONE',  ( 11.50312500061451892, -4.541064518000417216, -2.621784821875001281 ) ) ;
#71223 = CARTESIAN_POINT ( 'NONE',  ( 24.30937500061451573, 2.746126346562643317, 4.756430356249998326 ) ) ;
#71224 = CARTESIAN_POINT ( 'NONE',  ( 6.084375000614518747, -4.541064518000419881, 2.621784821874995952 ) ) ;
#71225 = CARTESIAN_POINT ( 'NONE',  ( 23.88749999999999929, -2.886751345948125991, -5.000000000000000000 ) ) ;
#71226 = CARTESIAN_POINT ( 'NONE',  ( 19.80000000122903359, -2.886751345948129988, 4.999999999999997335 ) ) ;
#71227 = CARTESIAN_POINT ( 'NONE',  ( 27.02812500061451573, 4.541064518000418104, 2.621784821874999949 ) ) ;
#71228 = FACE_OUTER_BOUND ( 'NONE', #66972, .T. ) ;
#71229 = CARTESIAN_POINT ( 'NONE',  ( 8.896875000614517859, -3.027376345333610441, -5.243569643749999898 ) ) ;
#71230 = CARTESIAN_POINT ( 'NONE',  ( 14.52187500061451608, 3.027376345333611329, 5.243569643749999010 ) ) ;
#71231 = CARTESIAN_POINT ( 'NONE',  ( 23.74687500061451573, -3.027376345333610441, -5.243569643749999898 ) ) ;
#71232 = CARTESIAN_POINT ( 'NONE',  ( 45.00000000000000000, 0.000000000000000000, 0.000000000000000000 ) ) ;
#71233 = CARTESIAN_POINT ( 'NONE',  ( 12.18750000000000000, -2.886751345948125991, -5.000000000000000000 ) ) ;
#71234 = CARTESIAN_POINT ( 'NONE',  ( 18.72187500061451360, -6.054752690667223547, -1.112240025338166033E-15 ) ) ;
#71235 = CARTESIAN_POINT ( 'NONE',  ( 9.721875000614517148, -6.054752690667223547, -1.112240025338166033E-15 ) ) ;
#71236 = CARTESIAN_POINT ( 'NONE',  ( 2.655984681222220721E-16, 13.20312499938548534, 25.66244784525396483 ) ) ;
#71237 = CARTESIAN_POINT ( 'NONE',  ( 23.47499999999999787, 6.123233995736764310E-16, -4.999999999999998224 ) ) ;
#71238 = CARTESIAN_POINT ( 'NONE',  ( 2.828200636599751609E-16, 14.86250000000000071, 25.38119784648299415 ) ) ;
#71239 = CARTESIAN_POINT ( 'NONE',  ( -1.389182545231912203, 9.676047173952133207, -33.81675723707382275 ) ) ;
#71240 = CARTESIAN_POINT ( 'NONE',  ( 24.87187500061451573, 2.746126346562643317, 4.756430356249998326 ) ) ;
#71241 = CARTESIAN_POINT ( 'NONE',  ( 12.06562500061451537, 3.027376345333613106, -5.243569643749998122 ) ) ;
#71242 = CARTESIAN_POINT ( 'NONE',  ( 29.78437500061451715, 4.541064518000418104, 2.621784821874999949 ) ) ;
#71243 =( LENGTH_UNIT ( ) NAMED_UNIT ( * ) SI_UNIT ( .MILLI., .METRE. ) );
#71244 = CARTESIAN_POINT ( 'NONE',  ( 1.999999999999998668, 10.06250000122903465, -33.46410161513775705 ) ) ;
#71245 = CARTESIAN_POINT ( 'NONE',  ( 12.37500000000000000, 4.330127018922191873, 2.499999999999999556 ) ) ;
#71246 = CARTESIAN_POINT ( 'NONE',  ( -3.999999999999999556, 18.72500000122903074, 27.69059892324149530 ) ) ;
#71247 = CARTESIAN_POINT ( 'NONE',  ( 12.00000000122903465, 5.773502691896255534, 3.535250795749688894E-16 ) ) ;
#71248 = CARTESIAN_POINT ( 'NONE',  ( 21.90937500061451715, -4.541064518000417216, -2.621784821875001281 ) ) ;
#71249 = CARTESIAN_POINT ( 'NONE',  ( 17.18437500061451573, 4.541064518000418104, 2.621784821874999949 ) ) ;
#71250 = CARTESIAN_POINT ( 'NONE',  ( -3.999999999999999112, 16.40000000000000213, -30.00000000000000000 ) ) ;
#71251 = VERTEX_POINT ( 'NONE', #39005 ) ;
#71252 = CARTESIAN_POINT ( 'NONE',  ( 18.10312500061451502, 0.000000000000000000, 5.243569643749999010 ) ) ;
#71253 = CARTESIAN_POINT ( 'NONE',  ( 28.20000000122903216, 5.773502691896255534, 3.535250795749688894E-16 ) ) ;
#71254 = CARTESIAN_POINT ( 'NONE',  ( 18.57187500061451857, 3.027376345333611329, 5.243569643749999010 ) ) ;
#71255 = CARTESIAN_POINT ( 'NONE',  ( 29.52187500061451431, -6.054752690667223547, -1.112240025338166033E-15 ) ) ;
#71256 = CARTESIAN_POINT ( 'NONE',  ( 5.353125000614515905, 4.541064518000418104, -2.621784821874998173 ) ) ;
#71257 = CARTESIAN_POINT ( 'NONE',  ( 19.94062500061451715, -3.027376345333614438, 5.243569643749998122 ) ) ;
#71258 = CARTESIAN_POINT ( 'NONE',  ( 27.98437500061451289, 4.541064518000418104, 2.621784821874999949 ) ) ;
#71259 = CARTESIAN_POINT ( 'NONE',  ( -2.121784821874999949, 12.52812500061451573, 26.32496088578401938 ) ) ;
#71260 = CARTESIAN_POINT ( 'NONE',  ( 17.77500000122903145, 2.886751345948129099, -4.999999999999998224 ) ) ;
#71261 = CARTESIAN_POINT ( 'NONE',  ( 11.03437500061451715, -4.119189519843968306, 2.378215178124996054 ) ) ;
#71262 = CARTESIAN_POINT ( 'NONE',  ( 7.153125000614518392, 4.541064518000418104, -2.621784821874998173 ) ) ;
#71263 = CARTESIAN_POINT ( 'NONE',  ( 27.59062500061451573, -3.027376345333614438, 5.243569643749998122 ) ) ;
#71264 = DIRECTION ( 'NONE',  ( -0.000000000000000000, -1.000000000000000000, -0.000000000000000000 ) ) ;
#71265 = EDGE_CURVE ( 'NONE', #23627, #8722, #2853, .T. ) ;
#71266 = CARTESIAN_POINT ( 'NONE',  ( 22.73437500061451644, -4.541064518000419881, 2.621784821874995952 ) ) ;
#71267 = CARTESIAN_POINT ( 'NONE',  ( 12.14062500061451821, 6.054752690667223547, 3.707466751127219781E-16 ) ) ;
#71268 = CARTESIAN_POINT ( 'NONE',  ( 23.58750000122903145, 6.123233995736764310E-16, -4.999999999999998224 ) ) ;
#71269 = CARTESIAN_POINT ( 'NONE',  ( 22.97812500061451857, 4.541064518000418104, 2.621784821874999949 ) ) ;
#71270 = CARTESIAN_POINT ( 'NONE',  ( 16.28437500061452070, 4.541064518000418104, 2.621784821874999949 ) ) ;
#71271 = CARTESIAN_POINT ( 'NONE',  ( 13.41562500061451502, 3.027376345333613106, -5.243569643749998122 ) ) ;
#71272 = CARTESIAN_POINT ( 'NONE',  ( -2.121784821874999949, 14.38437500061451679, 26.32496088578401938 ) ) ;
#71273 = CARTESIAN_POINT ( 'NONE',  ( 19.71562500061451928, 3.027376345333613106, -5.243569643749998122 ) ) ;
#71274 = CARTESIAN_POINT ( 'NONE',  ( 29.57812500061451644, 6.421520780324663323E-16, -5.243569643749999010 ) ) ;
#71275 = EDGE_LOOP ( 'NONE', ( #1061, #64504, #21894, #33313 ) ) ;
#71276 = ORIENTED_EDGE ( 'NONE', *, *, #60032, .F. ) ;
#71277 = CARTESIAN_POINT ( 'NONE',  ( 22.83749999999999858, -2.886751345948129988, 4.999999999999997335 ) ) ;
#71278 = CARTESIAN_POINT ( 'NONE',  ( -4.243569643749999898, 18.50937500061451857, -30.00000000000000000 ) ) ;
#71279 = CARTESIAN_POINT ( 'NONE',  ( 13.01250000122903394, 0.000000000000000000, 4.999999999999998224 ) ) ;
#71280 = CARTESIAN_POINT ( 'NONE',  ( 25.79062500061451502, -3.027376345333614438, 5.243569643749998122 ) ) ;
#71281 = CARTESIAN_POINT ( 'NONE',  ( 5.615625000614517859, -6.054752690667223547, -1.112240025338166033E-15 ) ) ;
#71282 = CARTESIAN_POINT ( 'NONE',  ( 20.47500000122903074, 2.886751345948129099, -4.999999999999998224 ) ) ;
#71283 = CARTESIAN_POINT ( 'NONE',  ( 23.95312500061451289, 0.000000000000000000, 5.243569643749999010 ) ) ;
#71284 = CARTESIAN_POINT ( 'NONE',  ( 23.62500000000000000, 4.330127018922191873, 2.499999999999999556 ) ) ;
#71285 = CARTESIAN_POINT ( 'NONE',  ( 27.51562500061451644, 3.027376345333611329, 5.243569643749999010 ) ) ;
#71286 = CARTESIAN_POINT ( 'NONE',  ( 7.078125000614516438, 6.421520780324663323E-16, -5.243569643749999010 ) ) ;
#71287 = ORIENTED_EDGE ( 'NONE', *, *, #16220, .F. ) ;
#71288 = CARTESIAN_POINT ( 'NONE',  ( 24.44062500061451715, -3.027376345333614438, 5.243569643749998122 ) ) ;
#71289 = CARTESIAN_POINT ( 'NONE',  ( 5.840625000614516615, 6.054752690667223547, 3.707466751127219781E-16 ) ) ;
#71290 = CARTESIAN_POINT ( 'NONE',  ( 14.52187500061451608, 2.746126346562643317, 4.756430356249998326 ) ) ;
#71291 = CARTESIAN_POINT ( 'NONE',  ( 4.003125000614518925, 4.541064518000418104, -2.621784821874998173 ) ) ;
#71292 = CARTESIAN_POINT ( 'NONE',  ( -2.000000000000000000, 13.28750000122903430, -33.46410161513775705 ) ) ;
#71293 = DIRECTION ( 'NONE',  ( 0.000000000000000000, 0.000000000000000000, -1.000000000000000000 ) ) ;
#71294 =( BOUNDED_CURVE ( )  B_SPLINE_CURVE ( 2, ( #2116, #24265, #24991, #17985, #41628, #41998, #30179 ),
 .UNSPECIFIED., .F., .F. ) 
 B_SPLINE_CURVE_WITH_KNOTS ( ( 3, 2, 2, 3 ),
 ( 0.09166666666666660468, 0.09444444444444442810, 0.09722222222222223764, 0.1000000000000000611 ),
 .UNSPECIFIED. ) 
 CURVE ( )  GEOMETRIC_REPRESENTATION_ITEM ( )  RATIONAL_B_SPLINE_CURVE ( ( 1.000000000000002665, 0.8660254037844360431, 1.000000000000000000, 0.8660254037844387076, 1.000000000000000000, 0.8660254037844360431, 1.000000000000002665 ) ) 
 REPRESENTATION_ITEM ( '' )  );
#71295 = CARTESIAN_POINT ( 'NONE',  ( 9.937500000000001776, -2.886751345948125991, -5.000000000000000000 ) ) ;
#71296 = CARTESIAN_POINT ( 'NONE',  ( 11.97187500061451892, -6.054752690667223547, -1.112240025338166033E-15 ) ) ;
#71297 = CARTESIAN_POINT ( 'NONE',  ( 7.462500001229035007, 4.330127018922192761, -2.499999999999997780 ) ) ;
#71298 = CARTESIAN_POINT ( 'NONE',  ( 13.58437500061451786, 4.541064518000418104, 2.621784821874999949 ) ) ;
#71299 = CARTESIAN_POINT ( 'NONE',  ( 14.62500000000000000, 4.330127018922191873, 2.499999999999999556 ) ) ;
#71300 = CARTESIAN_POINT ( 'NONE',  ( 6.684375000614518392, 6.421520780324663323E-16, -5.243569643749999010 ) ) ;
#71301 = CARTESIAN_POINT ( 'NONE',  ( 4.243569643749999898, 10.12812500061451715, -30.00000000000000000 ) ) ;
#71302 = DIRECTION ( 'NONE',  ( -0.000000000000000000, -1.000000000000000000, -0.000000000000000000 ) ) ;
#71303 = CARTESIAN_POINT ( 'NONE',  ( 12.04687500061451821, -3.027376345333610441, -5.243569643749999898 ) ) ;
#71304 = CARTESIAN_POINT ( 'NONE',  ( 22.01250000122903216, 0.000000000000000000, 4.999999999999998224 ) ) ;
#71305 = EDGE_CURVE ( 'NONE', #5101, #57768, #849, .T. ) ;
#71306 = CARTESIAN_POINT ( 'NONE',  ( 21.17812500061451431, 4.541064518000418104, 2.621784821874999949 ) ) ;
#71307 = CARTESIAN_POINT ( 'NONE',  ( 4.898587196589411843E-16, 20.00000000000000000, -26.00000000000000000 ) ) ;
#71308 = CARTESIAN_POINT ( 'NONE',  ( -2.121784821874996840, 19.42812500061459602, 33.67503911421598417 ) ) ;
#71309 = CARTESIAN_POINT ( 'NONE',  ( 24.87187500061451573, 3.027376345333611329, 5.243569643749999010 ) ) ;
#71310 =( BOUNDED_CURVE ( )  B_SPLINE_CURVE ( 2, ( #10464, #43359, #71800, #32994, #38543, #71058, #44091 ),
 .UNSPECIFIED., .F., .F. ) 
 B_SPLINE_CURVE_WITH_KNOTS ( ( 3, 2, 2, 3 ),
 ( 0.9517299907128293768, 0.9527777777777777235, 0.9555555555555556024, 0.9564971600366024562 ),
 .UNSPECIFIED. ) 
 CURVE ( )  GEOMETRIC_REPRESENTATION_ITEM ( )  RATIONAL_B_SPLINE_CURVE ( ( 0.9370531128228860585, 0.9494643343793163215, 1.000000000000000000, 0.8660254037844387076, 1.000000000000000000, 0.9545856111485142570, 0.9399601445705541014 ) ) 
 REPRESENTATION_ITEM ( '' )  );
#71311 = CARTESIAN_POINT ( 'NONE',  ( 5.053125000614517859, 0.000000000000000000, 5.243569643749999010 ) ) ;
#71312 = AXIS2_PLACEMENT_3D ( 'NONE', #31534, #3094, #54436 ) ;
#71313 = CARTESIAN_POINT ( 'NONE',  ( 22.84687500061451360, 4.119189519843966529, -2.378215178124998275 ) ) ;
#71314 = CARTESIAN_POINT ( 'NONE',  ( 17.95312500061451644, 4.541064518000418104, -2.621784821874998173 ) ) ;
#71315 = CARTESIAN_POINT ( 'NONE',  ( 15.34687500061451537, 6.054752690667223547, 3.707466751127219781E-16 ) ) ;
#71316 = CARTESIAN_POINT ( 'NONE',  ( 29.84999999999999787, 4.330127018922192761, -2.499999999999997780 ) ) ;
#71317 = CARTESIAN_POINT ( 'NONE',  ( 26.25000000122903288, -2.886751345948125991, -5.000000000000000000 ) ) ;
#71318 = CARTESIAN_POINT ( 'NONE',  ( 6.984375000614516438, -4.541064518000419881, 2.621784821874995952 ) ) ;
#71319 = AXIS2_PLACEMENT_3D ( 'NONE', #45144, #10069, #5621 ) ;
#71320 = CARTESIAN_POINT ( 'NONE',  ( 17.03437500061451715, 6.421520780324663323E-16, -5.243569643749999010 ) ) ;
#71321 = DIRECTION ( 'NONE',  ( -1.000000000000000000, -0.000000000000000000, -0.000000000000000000 ) ) ;
#71322 = CARTESIAN_POINT ( 'NONE',  ( 25.08749999999999858, -2.886751345948129988, 4.999999999999997335 ) ) ;
#71323 = CARTESIAN_POINT ( 'NONE',  ( 3.750000001229034652, -2.886751345948125991, -5.000000000000000000 ) ) ;
#71324 = CARTESIAN_POINT ( 'NONE',  ( 28.24687500061451573, -3.027376345333610441, -5.243569643749999898 ) ) ;
#71325 = CARTESIAN_POINT ( 'NONE',  ( 15.57187500061451679, -6.054752690667223547, -1.112240025338166033E-15 ) ) ;
#71326 = CARTESIAN_POINT ( 'NONE',  ( 3.756430356250000546, 13.24062499938548321, 27.83122392262697886 ) ) ;
#71327 = LINE ( 'NONE', #2993, #69296 ) ;
#71328 = CARTESIAN_POINT ( 'NONE',  ( 9.150000000000002132, 4.330127018922192761, -2.499999999999997780 ) ) ;
#71329 = CARTESIAN_POINT ( 'NONE',  ( 10.35937500061451644, 2.746126346562643317, 4.756430356249998326 ) ) ;
#71330 = CARTESIAN_POINT ( 'NONE',  ( 20.31562500061451715, 3.027376345333611329, 5.243569643749999010 ) ) ;
#71331 = CARTESIAN_POINT ( 'NONE',  ( 12.44999999999999929, 0.000000000000000000, 4.999999999999998224 ) ) ;
#71332 = CARTESIAN_POINT ( 'NONE',  ( 3.515625000614516882, 3.027376345333613106, -5.243569643749998122 ) ) ;
#71333 = CARTESIAN_POINT ( 'NONE',  ( 18.67500000000000071, 4.330127018922191873, 2.499999999999999556 ) ) ;
#71334 = CARTESIAN_POINT ( 'NONE',  ( 18.74062500061451431, -3.027376345333610441, -5.243569643749999898 ) ) ;
#71335 = CARTESIAN_POINT ( 'NONE',  ( 23.02499999999999858, 6.123233995736764310E-16, -4.999999999999998224 ) ) ;
#71336 = CARTESIAN_POINT ( 'NONE',  ( 22.53750000122903430, -4.330127018922194537, 2.499999999999995559 ) ) ;
#71337 = CARTESIAN_POINT ( 'NONE',  ( 3.756430356249998770, 20.25312499938547717, 32.16877607737301759 ) ) ;
#71338 =( BOUNDED_CURVE ( )  B_SPLINE_CURVE ( 2, ( #3959, #14292, #54557, #26855, #49387, #48653, #37193 ),
 .UNSPECIFIED., .F., .F. ) 
 B_SPLINE_CURVE_WITH_KNOTS ( ( 3, 2, 2, 3 ),
 ( 0.1200000000000000788, 0.1233333333333334059, 0.1266666666666667329, 0.1300000000000000322 ),
 .UNSPECIFIED. ) 
 CURVE ( )  GEOMETRIC_REPRESENTATION_ITEM ( )  RATIONAL_B_SPLINE_CURVE ( ( 0.9999999999999966693, 0.8660254037844420383, 1.000000000000000000, 0.8660254037844387076, 1.000000000000000000, 0.8660254037844375974, 1.000000000000001110 ) ) 
 REPRESENTATION_ITEM ( '' )  );
#71339 = CARTESIAN_POINT ( 'NONE',  ( 29.18437500061451573, 6.421520780324663323E-16, -5.243569643749999010 ) ) ;
#71340 = ORIENTED_EDGE ( 'NONE', *, *, #56383, .F. ) ;
#71341 = CARTESIAN_POINT ( 'NONE',  ( 17.57812500061451644, 4.541064518000418104, 2.621784821874999949 ) ) ;
#71342 = CARTESIAN_POINT ( 'NONE',  ( 25.07812500061451644, 6.421520780324663323E-16, -5.243569643749999010 ) ) ;
#71343 = CARTESIAN_POINT ( 'NONE',  ( 25.54687500061451644, -3.027376345333610441, -5.243569643749999898 ) ) ;
#71344 = CARTESIAN_POINT ( 'NONE',  ( 8.699999999999999289, 4.330127018922192761, -2.499999999999997780 ) ) ;
#71345 = CARTESIAN_POINT ( 'NONE',  ( 11.09062500061451573, -3.027376345333610441, -5.243569643749999898 ) ) ;
#71346 = CARTESIAN_POINT ( 'NONE',  ( 26.24062500061451431, -3.027376345333614438, 5.243569643749998122 ) ) ;
#71347 = CARTESIAN_POINT ( 'NONE',  ( 17.82187500061451502, -6.054752690667223547, -1.112240025338166033E-15 ) ) ;
#71348 = CARTESIAN_POINT ( 'NONE',  ( 9.740625000614516082, -3.027376345333610441, -5.243569643749999898 ) ) ;
#71349 = CARTESIAN_POINT ( 'NONE',  ( 7.162500001229032520, 0.000000000000000000, 4.999999999999998224 ) ) ;
#71350 = CARTESIAN_POINT ( 'NONE',  ( 2.121784821875001281, 19.50312500061451360, 33.67503911421598417 ) ) ;
#71351 = EDGE_CURVE ( 'NONE', #23511, #16810, #3290, .T. ) ;
#71352 = CARTESIAN_POINT ( 'NONE',  ( 24.18750000122903288, 4.330127018922191873, 2.499999999999999556 ) ) ;
#71353 = CARTESIAN_POINT ( 'NONE',  ( 17.67187500061451999, 2.746126346562643317, 4.756430356249998326 ) ) ;
#71354 = CARTESIAN_POINT ( 'NONE',  ( 14.50312500061451537, 0.000000000000000000, 5.243569643749999010 ) ) ;
#71355 = CARTESIAN_POINT ( 'NONE',  ( 8.034375000614518925, 6.421520780324663323E-16, -5.243569643749999010 ) ) ;
#71356 = CARTESIAN_POINT ( 'NONE',  ( 6.084375000614518747, -4.541064518000419881, 2.621784821874995952 ) ) ;
#71357 = ORIENTED_EDGE ( 'NONE', *, *, #8966, .F. ) ;
#71358 = CARTESIAN_POINT ( 'NONE',  ( 3.999999999999998668, 13.51250000000000107, 27.69059892324149530 ) ) ;
#71359 = CARTESIAN_POINT ( 'NONE',  ( 22.49062500061451431, 6.054752690667223547, 3.707466751127219781E-16 ) ) ;
#71360 = CARTESIAN_POINT ( 'NONE',  ( 15.64687500061451608, -3.027376345333610441, -5.243569643749999898 ) ) ;
#71361 = CARTESIAN_POINT ( 'NONE',  ( 19.52812500061451573, -4.541064518000419881, 2.621784821874995952 ) ) ;
#71362 = CARTESIAN_POINT ( 'NONE',  ( 3.999999999999999112, 13.02500000000000213, 30.00000000000000000 ) ) ;
#71363 = AXIS2_PLACEMENT_3D ( 'NONE', #64747, #36673, #58099 ) ;
#71364 = CARTESIAN_POINT ( 'NONE',  ( 26.12812500061451360, 4.541064518000418104, 2.621784821874999949 ) ) ;
#71365 = CARTESIAN_POINT ( 'NONE',  ( 7.012500001229035718, 4.330127018922192761, -2.499999999999997780 ) ) ;
#71366 = ORIENTED_EDGE ( 'NONE', *, *, #431, .T. ) ;
#71367 = CARTESIAN_POINT ( 'NONE',  ( 2.850000001229036073, -2.886751345948125991, -5.000000000000000000 ) ) ;
#71368 = CARTESIAN_POINT ( 'NONE',  ( -2.828200636599751609E-16, 18.53750000000000142, -34.61880215351700230 ) ) ;
#71369 = CARTESIAN_POINT ( 'NONE',  ( 21.86250000122903003, 4.330127018922192761, -2.499999999999997780 ) ) ;
#71370 = CARTESIAN_POINT ( 'NONE',  ( 1.878215178125000495, 15.52812499938548285, 26.74683588394047007 ) ) ;
#71371 = CARTESIAN_POINT ( 'NONE',  ( 6.534375000614517148, -4.541064518000419881, 2.621784821874995952 ) ) ;
#71372 = LINE ( 'NONE', #19644, #59680 ) ;
#71373 = CARTESIAN_POINT ( 'NONE',  ( 13.22812500061451502, -4.541064518000419881, 2.621784821874995952 ) ) ;
#71374 = CARTESIAN_POINT ( 'NONE',  ( 8.784375000614518925, -4.541064518000419881, 2.621784821874995952 ) ) ;
#71375 = CARTESIAN_POINT ( 'NONE',  ( 26.40000000122902790, 5.773502691896255534, 3.535250795749688894E-16 ) ) ;
#71376 = CARTESIAN_POINT ( 'NONE',  ( 16.50937500061451502, -4.541064518000417216, -2.621784821875001281 ) ) ;
#71377 = CARTESIAN_POINT ( 'NONE',  ( 5.971875000614516260, 3.027376345333611329, 5.243569643749999010 ) ) ;
#71378 = CARTESIAN_POINT ( 'NONE',  ( 29.62500000000000000, -4.330127018922194537, 2.499999999999995559 ) ) ;
#71379 = CARTESIAN_POINT ( 'NONE',  ( 5.278125000614516615, 6.421520780324663323E-16, -5.243569643749999010 ) ) ;
#71380 = CARTESIAN_POINT ( 'NONE',  ( 14.61562500061451608, -6.054752690667223547, -1.112240025338166033E-15 ) ) ;
#71381 = EDGE_LOOP ( 'NONE', ( #26452, #32987, #43290, #65973 ) ) ;
#71382 = AXIS2_PLACEMENT_3D ( 'NONE', #40904, #12449, #63771 ) ;
#71383 = CARTESIAN_POINT ( 'NONE',  ( 11.42812500061451608, -4.541064518000419881, 2.621784821874995952 ) ) ;
#71384 = CARTESIAN_POINT ( 'NONE',  ( 6.487500001229034474, 6.123233995736764310E-16, -4.999999999999998224 ) ) ;
#71385 = VECTOR ( 'NONE', #69266, 1000.000000000000000 ) ;
#71386 = CARTESIAN_POINT ( 'NONE',  ( 8.803125000614517859, -4.541064518000417216, -2.621784821875001281 ) ) ;
#71387 = CARTESIAN_POINT ( 'NONE',  ( 22.28437500061451715, -4.119189519843968306, 2.378215178124996054 ) ) ;
#71388 = CARTESIAN_POINT ( 'NONE',  ( 9.187500000000001776, 5.773502691896255534, 3.535250795749688894E-16 ) ) ;
#71389 = CARTESIAN_POINT ( 'NONE',  ( 4.800000001229032698, 5.773502691896255534, 3.535250795749688894E-16 ) ) ;
#71390 = CARTESIAN_POINT ( 'NONE',  ( 16.98750000000000426, -2.886751345948129988, 4.999999999999997335 ) ) ;
#71391 = CARTESIAN_POINT ( 'NONE',  ( 17.40937500061451715, -4.541064518000417216, -2.621784821875001281 ) ) ;
#71392 = CARTESIAN_POINT ( 'NONE',  ( 13.68750000122903288, 6.123233995736764310E-16, -4.999999999999998224 ) ) ;
#71393 = B_SPLINE_CURVE_WITH_KNOTS ( 'NONE', 1,
 ( #9044, #58170 ),
 .UNSPECIFIED., .F., .F.,
 ( 2, 2 ),
 ( 0.000000000000000000, 1.000000000000000000 ),
 .UNSPECIFIED. ) ;
#71394 = CARTESIAN_POINT ( 'NONE',  ( 22.64999999999999858, 4.330127018922192761, -2.499999999999997780 ) ) ;
#71395 = CARTESIAN_POINT ( 'NONE',  ( -2.121784821874996840, 16.27812500061451573, -26.32496088578401583 ) ) ;
#71396 = CARTESIAN_POINT ( 'NONE',  ( 22.80000000000000071, 0.000000000000000000, 4.999999999999998224 ) ) ;
#71397 = CARTESIAN_POINT ( 'NONE',  ( 3.544807824988736478, -3.526624500747946200, 3.544807824988736478 ) ) ;
#71398 = CARTESIAN_POINT ( 'NONE',  ( 28.07812500061451289, -4.541064518000419881, 2.621784821874995952 ) ) ;
#71399 = CARTESIAN_POINT ( 'NONE',  ( 1.626862140677534273E-15, 12.12500000122903465, 34.00000000000000000 ) ) ;
#71400 = DIRECTION ( 'NONE',  ( -1.000000000000000000, -0.000000000000000000, -0.000000000000000000 ) ) ;
#71401 = CARTESIAN_POINT ( 'NONE',  ( 14.97187500061451892, 3.027376345333611329, 5.243569643749999010 ) ) ;
#71402 = CARTESIAN_POINT ( 'NONE',  ( 27.11249999999999716, 2.886751345948129099, -4.999999999999998224 ) ) ;
#71403 = CARTESIAN_POINT ( 'NONE',  ( 12.02812500061451573, 6.421520780324663323E-16, -5.243569643749999010 ) ) ;
#71404 = CARTESIAN_POINT ( 'NONE',  ( 29.44687500061451146, -4.119189519843965641, -2.378215178125001383 ) ) ;
#71405 = CARTESIAN_POINT ( 'NONE',  ( 21.15937500061451715, 4.541064518000418104, -2.621784821874998173 ) ) ;
#71406 = CARTESIAN_POINT ( 'NONE',  ( 14.33437500061451608, 5.492252693125287522, 3.363034840372157021E-16 ) ) ;
#71407 = CARTESIAN_POINT ( 'NONE',  ( 6.665625000614515905, 3.027376345333613106, -5.243569643749998122 ) ) ;
#71408 = CARTESIAN_POINT ( 'NONE',  ( 12.04687500061451821, -3.027376345333610441, -5.243569643749999898 ) ) ;
#71409 = VERTEX_POINT ( 'NONE', #23357 ) ;
#71410 = CARTESIAN_POINT ( 'NONE',  ( 24.98437500061451644, -4.541064518000419881, 2.621784821874995952 ) ) ;
#71411 = CARTESIAN_POINT ( 'NONE',  ( 28.22812500061451502, 6.421520780324663323E-16, -5.243569643749999010 ) ) ;
#71412 = DIRECTION ( 'NONE',  ( 0.000000000000000000, -0.000000000000000000, 1.000000000000000000 ) ) ;
#71413 = CARTESIAN_POINT ( 'NONE',  ( 8.250000000000000000, 4.330127018922192761, -2.499999999999997780 ) ) ;
#71414 = CARTESIAN_POINT ( 'NONE',  ( 17.58750000122903145, -4.330127018922194537, 2.499999999999995559 ) ) ;
#71415 = CARTESIAN_POINT ( 'NONE',  ( -1.071796769724492338, 17.95490381179670081, -26.00000000000000711 ) ) ;
#71416 = CARTESIAN_POINT ( 'NONE',  ( 8.259375000614515017, -5.492252693125287522, -1.008910452111647106E-15 ) ) ;
#71417 = VERTEX_POINT ( 'NONE', #57338 ) ;
#71418 = CARTESIAN_POINT ( 'NONE',  ( 15.93750000000000000, 5.773502691896255534, 3.535250795749688894E-16 ) ) ;
#71419 = CARTESIAN_POINT ( 'NONE',  ( 17.96250000000000213, -5.773502691896255534, -1.060575238724906372E-15 ) ) ;
#71420 = CARTESIAN_POINT ( 'NONE',  ( 10.56562500061451715, -6.054752690667223547, -1.112240025338166033E-15 ) ) ;
#71421 = ORIENTED_EDGE ( 'NONE', *, *, #40580, .F. ) ;
#71422 = CARTESIAN_POINT ( 'NONE',  ( -5.810221930991193690E-16, 10.88749999999999929, -34.00000000000000000 ) ) ;
#71423 = CARTESIAN_POINT ( 'NONE',  ( 4.243569643749999010, 16.97187500061451360, -32.45002607614398471 ) ) ;
#71424 = CARTESIAN_POINT ( 'NONE',  ( 4.528125000614516615, 4.541064518000418104, 2.621784821874999949 ) ) ;
#71425 = CARTESIAN_POINT ( 'NONE',  ( -1.878215178124999163, 12.79062499938548392, 26.74683588394047007 ) ) ;
#71426 = CARTESIAN_POINT ( 'NONE',  ( 9.712500000000002132, 2.886751345948126879, 4.999999999999999112 ) ) ;
#71427 = DIRECTION ( 'NONE',  ( -1.000000000000000000, -0.000000000000000000, -0.000000000000000000 ) ) ;
#71428 = ORIENTED_EDGE ( 'NONE', *, *, #45249, .F. ) ;
#71429 = CARTESIAN_POINT ( 'NONE',  ( -3.000416591977282496E-16, 13.39062500061451644, 25.09994784771203058 ) ) ;
#71430 = CARTESIAN_POINT ( 'NONE',  ( 25.79062500061451502, -3.027376345333614438, 5.243569643749998122 ) ) ;
#71431 = DIRECTION ( 'NONE',  ( 0.000000000000000000, 1.000000000000000000, -1.040834085586083941E-14 ) ) ;
#71432 = VECTOR ( 'NONE', #8258, 1000.000000000000000 ) ;
#71433 = CYLINDRICAL_SURFACE ( 'NONE', #52548, 4.999999999999998224 ) ;
#71434 = CARTESIAN_POINT ( 'NONE',  ( 20.33437500061451786, 4.541064518000418104, 2.621784821874999949 ) ) ;
#71435 = CARTESIAN_POINT ( 'NONE',  ( 19.45312500061451644, 0.000000000000000000, 5.243569643749999010 ) ) ;
#71436 = EDGE_CURVE ( 'NONE', #69475, #18169, #17933, .T. ) ;
#71437 = CARTESIAN_POINT ( 'NONE',  ( 9.001249775931846008E-16, 14.96562500061459744, -25.09994784771203058 ) ) ;
#71438 = CARTESIAN_POINT ( 'NONE',  ( 23.62500000122902932, 2.886751345948129099, -4.999999999999998224 ) ) ;
#71439 = CARTESIAN_POINT ( 'NONE',  ( 3.065625000614517592, 3.027376345333613106, -5.243569643749998122 ) ) ;
#71440 = CARTESIAN_POINT ( 'NONE',  ( 27.15937500061451360, 0.000000000000000000, 4.756430356249998326 ) ) ;
#71441 = CARTESIAN_POINT ( 'NONE',  ( 21.21562500061451573, 3.027376345333611329, 5.243569643749999010 ) ) ;
#71442 = CARTESIAN_POINT ( 'NONE',  ( 8.559375000614515727, 4.119189519843966529, -2.378215178124998275 ) ) ;
#71443 = CARTESIAN_POINT ( 'NONE',  ( -3.756430356250000102, 16.46562499938548285, 30.00000000000000000 ) ) ;
#71444 = CARTESIAN_POINT ( 'NONE',  ( 14.55937500061451573, 0.000000000000000000, 5.243569643749999010 ) ) ;
#71445 = CARTESIAN_POINT ( 'NONE',  ( 15.00937500061451679, 0.000000000000000000, 5.243569643749999010 ) ) ;
#71446 = CARTESIAN_POINT ( 'NONE',  ( 24.49687500061451573, -3.027376345333614438, 5.243569643749998122 ) ) ;
#71447 = CARTESIAN_POINT ( 'NONE',  ( -2.121784821874996840, 14.98437500061451644, 33.67503911421598417 ) ) ;
#71448 = CARTESIAN_POINT ( 'NONE',  ( 4.190625000614518925, -3.027376345333614438, 5.243569643749998122 ) ) ;
#71449 = CARTESIAN_POINT ( 'NONE',  ( 28.79062500061451502, 6.054752690667223547, 3.707466751127219781E-16 ) ) ;
#71450 = ADVANCED_FACE ( 'NONE', ( #62879, #63966 ), #1571, .T. ) ;
#71451 = ADVANCED_FACE ( 'NONE', ( #29276 ), #64332, .T. ) ;
#71452 = CARTESIAN_POINT ( 'NONE',  ( 28.00312500061451715, 0.000000000000000000, 5.243569643749999010 ) ) ;
#71453 = CARTESIAN_POINT ( 'NONE',  ( 4.000000000000000000, 16.25000000122903643, -27.69059892324149885 ) ) ;
#71454 = CARTESIAN_POINT ( 'NONE',  ( -3.999999999999997335, 19.58749999999999858, 32.30940107675850470 ) ) ;
#71455 = CARTESIAN_POINT ( 'NONE',  ( 6.271875000614517859, 3.027376345333613106, -5.243569643749998122 ) ) ;
#71456 = CARTESIAN_POINT ( 'NONE',  ( 14.55000000122903181, -2.886751345948125991, -5.000000000000000000 ) ) ;
#71457 = CARTESIAN_POINT ( 'NONE',  ( 9.525000001229033231, -5.773502691896255534, -1.060575238724906372E-15 ) ) ;
#71458 = CARTESIAN_POINT ( 'NONE',  ( 4.415625000614518569, 3.027376345333613106, -5.243569643749998122 ) ) ;
#71459 = CARTESIAN_POINT ( 'NONE',  ( -2.000000000000001776, 15.44374999877096677, 33.46410161513775705 ) ) ;
#71460 = CARTESIAN_POINT ( 'NONE',  ( 18.76875000122903359, 2.886751345948126879, 4.999999999999999112 ) ) ;
#71461 = CARTESIAN_POINT ( 'NONE',  ( 13.54687500061451999, 6.054752690667223547, 3.707466751127219781E-16 ) ) ;
#71462 = CARTESIAN_POINT ( 'NONE',  ( 1.071796769724491893, 17.54509619066136850, 33.99999999999999289 ) ) ;
#71463 = ORIENTED_EDGE ( 'NONE', *, *, #6663, .F. ) ;
#71464 = CARTESIAN_POINT ( 'NONE',  ( 21.36562500061451431, -6.054752690667223547, -1.112240025338166033E-15 ) ) ;
#71465 = CARTESIAN_POINT ( 'NONE',  ( 6.290625000614517681, 6.054752690667223547, 3.707466751127219781E-16 ) ) ;
#71466 = CARTESIAN_POINT ( 'NONE',  ( 25.62187500061451928, 3.027376345333612662, -5.243569643749998122 ) ) ;
#71467 = CARTESIAN_POINT ( 'NONE',  ( 6.665625000614515905, 3.027376345333613106, -5.243569643749998122 ) ) ;
#71468 = DIRECTION ( 'NONE',  ( -1.000000000000000000, -0.000000000000000000, -0.000000000000000000 ) ) ;
#71469 = CARTESIAN_POINT ( 'NONE',  ( 8.550000001229031810, -2.886751345948129988, 4.999999999999997335 ) ) ;
#71470 = CARTESIAN_POINT ( 'NONE',  ( 23.09062500061451573, -3.027376345333614438, 5.243569643749998122 ) ) ;
#71471 = CARTESIAN_POINT ( 'NONE',  ( 2.121784821874999061, 10.20312500061451821, -33.67503911421598417 ) ) ;
#71472 = CARTESIAN_POINT ( 'NONE',  ( 11.06250000122903288, 4.330127018922192761, -2.499999999999997780 ) ) ;
#71473 = CARTESIAN_POINT ( 'NONE',  ( 18.55312500061451431, 0.000000000000000000, 5.243569643749999010 ) ) ;
#71474 = AXIS2_PLACEMENT_3D ( 'NONE', #2849, #58252, #42014 ) ;
#71475 = CARTESIAN_POINT ( 'NONE',  ( 14.54062500061451679, -3.027376345333614438, 5.243569643749998122 ) ) ;
#71476 = CARTESIAN_POINT ( 'NONE',  ( 28.05937500061451573, 0.000000000000000000, 4.756430356249998326 ) ) ;
#71477 = CARTESIAN_POINT ( 'NONE',  ( 14.81250000000000000, -5.773502691896255534, -1.060575238724906372E-15 ) ) ;
#71478 = CARTESIAN_POINT ( 'NONE',  ( 12.30000000122903181, -2.886751345948125991, -5.000000000000000000 ) ) ;
#71479 = CARTESIAN_POINT ( 'NONE',  ( 7.453125000614516438, -4.541064518000417216, -2.621784821875001281 ) ) ;
#71480 = CARTESIAN_POINT ( 'NONE',  ( 11.39062500061451644, -3.027376345333614438, 5.243569643749998122 ) ) ;
#71481 =( BOUNDED_CURVE ( )  B_SPLINE_CURVE ( 3, ( #69179, #52179, #40019, #30373 ),
 .UNSPECIFIED., .F., .F. ) 
 B_SPLINE_CURVE_WITH_KNOTS ( ( 4, 4 ),
 ( 1.570796326794896558, 2.225934242759671111 ),
 .UNSPECIFIED. ) 
 CURVE ( )  GEOMETRIC_REPRESENTATION_ITEM ( )  RATIONAL_B_SPLINE_CURVE ( ( 1.000000000000000000, 0.9645515396217719806, 0.9645515396217719806, 1.000000000000000000 ) ) 
 REPRESENTATION_ITEM ( '' )  );
#71482 = VECTOR ( 'NONE', #65866, 1000.000000000000000 ) ;
#71483 = CARTESIAN_POINT ( 'NONE',  ( 24.26250000122903216, 0.000000000000000000, 4.999999999999998224 ) ) ;
#71484 = CARTESIAN_POINT ( 'NONE',  ( 18.75937500061451857, -4.541064518000417216, -2.621784821875001281 ) ) ;
#71485 = CARTESIAN_POINT ( 'NONE',  ( -1.071796769724480347, 18.66740381056766651, 34.00000000000000711 ) ) ;
#71486 = CARTESIAN_POINT ( 'NONE',  ( 4.275000001229035895, 2.886751345948129099, -4.999999999999998224 ) ) ;
#71487 = CARTESIAN_POINT ( 'NONE',  ( 4.959375000614516971, 4.541064518000418104, -2.621784821874998173 ) ) ;
#71488 = CARTESIAN_POINT ( 'NONE',  ( 22.28437500061451715, -4.541064518000419881, 2.621784821874995952 ) ) ;
#71489 = CARTESIAN_POINT ( 'NONE',  ( 10.61249999999999893, 2.886751345948193936, 4.999999999999883649 ) ) ;
#71490 = CARTESIAN_POINT ( 'NONE',  ( 19.37812500061451715, 4.541064518000418104, 2.621784821874999949 ) ) ;
#71491 = CARTESIAN_POINT ( 'NONE',  ( 24.27187500061452141, 3.027376345333613106, -5.243569643749998122 ) ) ;
#71492 = CARTESIAN_POINT ( 'NONE',  ( -3.756430356249999214, 20.59062499938548640, 27.83122392262697176 ) ) ;
#71493 = CARTESIAN_POINT ( 'NONE',  ( 12.41250000122903430, 4.330127018922192761, -2.499999999999997780 ) ) ;
#71494 = DIRECTION ( 'NONE',  ( -0.000000000000000000, -1.000000000000000000, -0.000000000000000000 ) ) ;
#71495 = CARTESIAN_POINT ( 'NONE',  ( 4.434375000614519280, 6.421520780324663323E-16, -5.243569643749999010 ) ) ;
#71496 = CARTESIAN_POINT ( 'NONE',  ( 14.16562500061451679, -6.054752690667223547, -1.112240025338166033E-15 ) ) ;
#71497 = CARTESIAN_POINT ( 'NONE',  ( 13.09687500061451892, 6.054752690667223547, 3.707466751127219781E-16 ) ) ;
#71498 = ORIENTED_EDGE ( 'NONE', *, *, #15666, .T. ) ;
#71499 = CARTESIAN_POINT ( 'NONE',  ( 1.071796769724497445, 17.16740381056766651, -33.99999999999998579 ) ) ;
#71500 = CARTESIAN_POINT ( 'NONE',  ( 26.01562500061451289, 3.027376345333613106, -5.243569643749998122 ) ) ;
#71501 = CARTESIAN_POINT ( 'NONE',  ( -2.000000000000000000, 10.58750000122903323, -33.46410161513775705 ) ) ;
#71502 = DIRECTION ( 'NONE',  ( -1.000000000000000000, -0.000000000000000000, -0.000000000000000000 ) ) ;
#71503 = CARTESIAN_POINT ( 'NONE',  ( 14.21249999999999858, 2.886751345948126879, 4.999999999999999112 ) ) ;
#71504 = CARTESIAN_POINT ( 'NONE',  ( 24.78750000122903074, -4.330127018922194537, 2.499999999999995559 ) ) ;
#71505 = CARTESIAN_POINT ( 'NONE',  ( 19.07812500061451644, -4.541064518000419881, 2.621784821874995952 ) ) ;
#71506 = ORIENTED_EDGE ( 'NONE', *, *, #58401, .F. ) ;
#71507 = CARTESIAN_POINT ( 'NONE',  ( 22.80000000000000071, 0.000000000000000000, 4.999999999999998224 ) ) ;
#71508 = CARTESIAN_POINT ( 'NONE',  ( 24.38437500061451502, 4.541064518000418104, 2.621784821874999949 ) ) ;
#71509 = VERTEX_POINT ( 'NONE', #24080 ) ;
#71510 = CARTESIAN_POINT ( 'NONE',  ( 19.01249999999999929, 2.886751345948073588, -5.000000000000094147 ) ) ;
#71511 = CARTESIAN_POINT ( 'NONE',  ( 11.50312500061451892, -4.541064518000417216, -2.621784821875001281 ) ) ;
#71512 = CARTESIAN_POINT ( 'NONE',  ( 4.490625000614516971, 6.054752690667223547, 3.707466751127219781E-16 ) ) ;
#71513 = CARTESIAN_POINT ( 'NONE',  ( 14.18437500061451573, -2.746126346562642428, -4.756430356249999214 ) ) ;
#71514 = CARTESIAN_POINT ( 'NONE',  ( 26.69062500061451715, -3.027376345333614438, 5.243569643749998122 ) ) ;
#71515 = AXIS2_PLACEMENT_3D ( 'NONE', #55117, #11769, #4516 ) ;
#71516 = CARTESIAN_POINT ( 'NONE',  ( 17.96250000000000213, -5.773502691896255534, -1.060575238724906372E-15 ) ) ;
#71517 = CARTESIAN_POINT ( 'NONE',  ( 25.87500000000000000, 4.330127018922191873, 2.499999999999999556 ) ) ;
#71518 = CARTESIAN_POINT ( 'NONE',  ( 7.837500001229035007, 6.123233995736764310E-16, -4.999999999999998224 ) ) ;
#71519 = CARTESIAN_POINT ( 'NONE',  ( 6.271875000614517859, 3.027376345333613106, -5.243569643749998122 ) ) ;
#71520 = CARTESIAN_POINT ( 'NONE',  ( 17.03437500061451715, 6.421520780324663323E-16, -5.243569643749999010 ) ) ;
#71521 = CARTESIAN_POINT ( 'NONE',  ( 28.05937500061451573, 0.000000000000000000, 5.243569643749999010 ) ) ;
#71522 = ORIENTED_EDGE ( 'NONE', *, *, #13592, .T. ) ;
#71523 = CARTESIAN_POINT ( 'NONE',  ( 26.46562500061451573, 3.027376345333613106, -5.243569643749998122 ) ) ;
#71524 = CARTESIAN_POINT ( 'NONE',  ( 26.85937500061451644, -4.541064518000417216, -2.621784821875001281 ) ) ;
#71525 = FACE_OUTER_BOUND ( 'NONE', #18154, .T. ) ;
#71526 = CARTESIAN_POINT ( 'NONE',  ( 14.40000000000000036, -4.330127018922190985, -2.500000000000001332 ) ) ;
#71527 = CARTESIAN_POINT ( 'NONE',  ( 10.30312500061451431, 4.541064518000418104, -2.621784821874998173 ) ) ;
#71528 = CARTESIAN_POINT ( 'NONE',  ( 9.543750001229033941, -2.886751345948126435, -5.000000000000000000 ) ) ;
#71529 = CARTESIAN_POINT ( 'NONE',  ( 14.02499999999999858, 6.123233995736764310E-16, -4.999999999999998224 ) ) ;
#71530 = CARTESIAN_POINT ( 'NONE',  ( 29.35312500061451502, 0.000000000000000000, 5.243569643749999010 ) ) ;
#71531 = CARTESIAN_POINT ( 'NONE',  ( 16.01250000122903216, 4.330127018922192761, -2.499999999999997780 ) ) ;
#71532 = CARTESIAN_POINT ( 'NONE',  ( 15.03750000122903252, 6.123233995736764310E-16, -4.999999999999998224 ) ) ;
#71533 = CARTESIAN_POINT ( 'NONE',  ( 15.94687500061451502, -2.746126346562646425, 4.756430356249996549 ) ) ;
#71534 = CARTESIAN_POINT ( 'NONE',  ( 5.390625000614518214, 6.054752690667223547, 3.707466751127219781E-16 ) ) ;
#71535 = CARTESIAN_POINT ( 'NONE',  ( 21.72187500061451715, 3.027376345333611329, 5.243569643749999010 ) ) ;
#71536 = CARTESIAN_POINT ( 'NONE',  ( -2.121784821874999949, 17.98437500061451999, 26.32496088578401938 ) ) ;
#71537 = CARTESIAN_POINT ( 'NONE',  ( 22.95937500061451431, 4.541064518000418104, -2.621784821874998173 ) ) ;
#71538 = CARTESIAN_POINT ( 'NONE',  ( 5.062500000000000888, 2.886751345948129099, -4.999999999999998224 ) ) ;
#71539 = CARTESIAN_POINT ( 'NONE',  ( 2.000000000000001332, 10.36250000122903359, 33.46410161513774995 ) ) ;
#71540 = CARTESIAN_POINT ( 'NONE',  ( 12.62812500061451537, 4.541064518000418104, 2.621784821874999949 ) ) ;
#71542 =( BOUNDED_SURFACE ( )  B_SPLINE_SURFACE ( 1, 2, ( 
 ( #57136, #6180, #12085, #34606, #34976, #1374, #46071, #68247, #46796, #57505, #6545, #69333, #30159, #69688, #28709, #23521, #51248, #63413, #29796, #68606, #68970, #651, #23159, #45713, #24609, #17610, #52332, #35697, #18327, #40170, #29079, #51614, #47156, #1015, #1734, #58217, #12445, #12799, #41255, #17967, #19053, #63044, #40900, #6907, #24248, #29438, #23884, #46431, #35335, #57858, #63767, #13155, #7622, #52692, #62329, #2098, #42343, #25342, #48987, #36064, #3924, #24971, #31251, #37525, #70045, #42706, #47516, #8353, #59682, #71142, #31626, #20515, #47888, #43073, #54521, #70416, #19418, #9089, #14617, #48253, #41978, #26078, #7991, #64499, #54160, #37156, #53424, #19792, #70776, #53054, #64866, #13891, #14254, #36431, #36793, #58945, #30527, #30882, #58584, #3556, #48617, #13516, #65599, #20152, #14987, #2448, #59308, #2814, #26447, #8719, #71517, #60046, #53793, #9457, #3188, #25715, #41611, #65228, #31987, #64130, #61513, #20892, #38632, #4654, #49353, #44551, #27183, #21256, #836, #66334, #68425, #33437, #29264, #43446, #60408, #54887, #15712, #15348, #43809, #38250, #66710, #33080, #49717, #26819, #5376, #16084, #60779, #28895, #62867, #51794, #37889, #55258, #65968, #21993, #10911, #72245, #55982, #61156, #21622, #40347, #23345, #44180, #10551, #51434, #9817, #50080, #55618, #45893, #10186, #67082, #32349, #4294, #71883, #5014, #32721, #27548, #72611, #16441, #38998, #17787, #12263, #34793, #57326, #6730, #69869, #18148, #64319, #2276, #7090, #52155, #25155, #35876, #13709, #35520, #24431, #29975, #19605, #42161, #63954, #1196, #47695, #24793, #68792, #12626, #63595, #23703, #64688, #14073, #24069, #41437, #57685, #36612, #13338, #58039, #35161, #47336, #46251, #7814, #59133, #52878, #7449, #8541, #58400, #58767, #52517, #19235, #41789, #70231, #29619, #1558, #36252, #8176, #40715, #63232, #30704, #46614, #53237, #2634, #18875, #31069, #69158, #18516, #41082, #1926, #30350, #12984, #46980, #69516, #3380, #19972, #4479, #4113, #27008, #37349, #10006, #37706, #31810, #43998, #26641, #49178, #32541, #49539, #66520, #71708, #59498, #25901, #43631, #55079, #9641, #48442, #31442, #32175, #53608, #59871, #53982, #70966, #43267, #3000, #38447, #42892, #42525, #72062, #9275, #10373, #21441, #20339, #15900, #66153, #60973, #25528, #65051, #14441, #65417, #48071, #14805, #54348, #26267, #65788, #3742, #8911, #38074, #48804, #71333, #60597, #70598, #36976, #20709, #15169, #60228, #54708, #21081, #15531, #39544, #21808, #49901, #4835, #68345, #61338, #50984, #6279, #56167, #33983, #39912, #55443, #40266, #39180, #11462, #33267, #45447, #27369, #5194, #27734, #38822, #55805, #10734, #62425, #72425, #44372, #62787, #56522, #33623, #16626, #32905, #66899, #17705, #16267, #22537, #28808, #50271, #5915, #72796, #22179, #382, #11824, #22889, #34342, #61696, #56875, #45809, #11095, #44733, #67980, #28449, #62068, #67267, #17355, #5561, #28098, #51347, #750, #50626, #31, #23259, #45085, #67620, #16986, #57958, #35077, #40999, #12543, #1115, #57603, #6650, #24712, #52796, #57237, #41709, #41357, #13623, #51712, #7366, #7007, #70146, #29537, #47615, #30263, #69073, #58317, #29179, #1842, #19524, #52072, #36167, #23622, #2197, #12180, #29896, #18432, #40629, #35795, #63514, #1477, #42082, #46168, #46531, #34707, #13257, #47255, #12901, #18793, #68708, #18068, #63148, #23984, #35434, #69789, #58685, #52435, #7729, #19155, #24349, #46897, #69436, #63867, #64233, #8095, #30624, #53156, #2554, #25072, #64970, #70519, #20995, #59050, #13991, #21360, #43183, #65332, #48358, #71986, #8455, #26927, #47991, #54264, #60513, #19895, #65702, #42448, #31360, #9557, #43547, #54622, #66069, #70883, #15447, #4398, #20257, #14361, #32091, #37625, #71245, #36896, #49093, #30990, #59416, #4028, #60148, #3293, #42809, #20624, #2917, #14721, #8823, #37264, #53901, #59786, #25820, #53523, #9192, #25448, #26553, #71622, #36530, #37991, #15089, #9919, #31727, #3659, #26182, #49452, #48722, #64605, #32457, #54992, #16904, #38359, #33537, #6197, #10652, #45363, #32821, #11382, #43914, #61614, #27649, #72344, #67541, #50185, #44284, #22812, #16187, #17270, #56445, #51266, #66439, #10291, #4753, #38738, #60886, #66814, #61258, #16545, #56087, #72713, #49820, #28367, #39097, #33182, #50903, #11742, #302, #15816, #668, #22096, #22455, #55721, #5835, #55359, #5115, #44654, #21725, #67184, #11016, #67898, #27286, #5479, #28018, #45004, #50546, #73074, #39459, #61980, #28725, #33901, #39831, #62346, #34259, #56792, #6565, #63062, #41276, #52712, #13177, #2118, #6925, #24630, #36085, #51992, #29097, #63787, #69354, #29816, #51632, #7643, #62708, #1033, #35716, #18711, #34995, #29455, #52351, #34623, #23902, #68625, #68988, #46089, #1393, #23539, #12102, #17987, #17627, #58238, #30181, #68265, #47175, #1754, #69708, #57154, #18345, #40546, #8012, #12465, #58605, #19074, #46450, #41631, #40187, #12819, #30547, #57524, #64150, #40920, #13537, #23176, #63432, #35353, #57877, #46816, #7287, #24267, #53074, #45730, #49007, #15008, #9840, #24993, #42000, #36452, #70437, #70066, #2835, #25364, #48274, #14637, #59328, #8374, #60067, #70798, #19812, #9479, #43465, #32369, #19439, #36813, #47537, #3577, #43092, #8739, #9110, #64520, #13913, #58966, #37912, #30903, #20536, #71538, #25737, #26100, #31648, #65989, #54181, #31272, #2469, #65248, #32008, #53815, #48638, #65620, #26468, #53445, #47908, #37545, #71163, #42365, #64887, #54543, #14275, #3945, #20913, #20173, #15370, #3208, #42727, #60429, #37178, #59703, #22015, #27569, #39379, #4673, #21277, #5757, #5395, #28291, #38652, #11303, #39017, #33099, #45283, #27932, #50465, #33824, #50822, #67817, #72993, #60800, #27203, #44926, #56367, #10930, #49738 ),
 ( #33457, #55638, #61176, #62267, #49374, #17190, #38272, #44571, #225, #10206, #56001, #32741, #21643, #22374, #22730, #67462, #39750, #10571, #11662, #54907, #5032, #55278, #16825, #61898, #61532, #72265, #4315, #43831, #44200, #26840, #71904, #66731, #50101, #66356, #15733, #72631, #16102, #67101, #16459, #62977, #34540, #23092, #57070, #28645, #46728, #1667, #6114, #63699, #63345, #35628, #587, #29374, #6477, #18982, #29012, #2031, #41543, #51183, #68540, #56713, #35267, #24176, #40461, #40829, #45649, #68183, #17546, #69620, #62621, #52265, #7554, #57436, #57789, #41190, #40107, #64061, #12373, #12731, #51549, #69263, #12017, #950, #23458, #46004, #17901, #34908, #13090, #6839, #51906, #34177, #7198, #1305, #23814, #46365, #68899, #18256, #29727, #18625, #30088, #58149, #52626, #24542, #47087, #31554, #43000, #3491, #65531, #70342, #14917, #26376, #42270, #19347, #54094, #59609, #20079, #41904, #71075, #52986, #64429, #26009, #9023, #25265, #19718, #42635, #24900, #14184, #58875, #59240, #36361, #64793, #13821, #2382, #8285, #7920, #48548, #20450, #58509, #37459, #65159, #59978, #47445, #8649, #30815, #71446, #53348, #48915, #9388, #36719, #31919, #30457, #3113, #20821, #2746, #54455, #69977, #3854, #13442, #31178, #53721, #47812, #37085, #25643, #48180, #43376, #70704, #35991, #14549, #138, #15280, #32282, #26750, #60705, #60339, #66263, #15640, #38560, #4945, #49647, #71816, #50380, #61083, #10118, #72905, #55549, #61806, #21187, #67011, #49283, #32648, #10840, #22287, #55911, #44839, #72174, #67374, #5671, #21554, #43738, #33375, #38927, #72536, #38181, #16737, #54816, #55189, #5304, #61446, #4584, #44108, #21924, #4222, #66634, #27114, #10481, #16012, #33010, #27479, #50012, #44480, #9748, #27849, #39292, #37820, #11209, #16372, #33736, #56282, #28207, #50736, #22644, #65900, #7469, #63253, #28918, #18168, #39659, #34815, #29995, #11928, #46635, #34090, #12645, #45194, #62887, #51456, #492, #68812, #859, #45561, #24088, #17459, #18538, #57705, #52536, #67726, #11575, #6026, #40017, #62178, #68092, #62531, #17808, #57345, #23366, #51095, #29639, #40369, #34453, #52177, #13003, #1945, #56631, #6385, #17099, #46273, #35181, #45914, #51814, #28560, #23001, #56981, #68446, #12282, #7110, #41102, #6751, #40737, #1579, #29284, #1217, #23723, #69177, #63612, #35540, #58060, #69891, #19256, #30371, #24813, #52900, #55007, #18894, #47000, #55374, #3022, #25176, #8199, #32837, #41456, #60901, #7834, #4413, #41811, #72000, #38007, #24451, #69535, #63974, #58422, #64341, #13357, #47359, #13733, #70255, #36633, #30728, #2298, #9936, #19628, #36275, #32474, #66455, #35898, #58789, #53260, #2658, #25553, #66084, #47717, #31091, #42184, #64709, #14093, #10304, #59155, #43562, #21375, #8563, #49108, #26942, #53630, #71637, #21010, #15462, #60529, #49467, #43929, #15832, #38377, #38753, #10667, #61274, #318, #49835, #27301, #28741, #67556, #61628, #44669, #6213, #72359, #34275, #16202, #28033, #39848, #33197, #16919, #55736, #50203, #11398, #22827, #33917, #45379, #67199, #67915, #56807, #16561, #5130, #56460, #39474, #22470, #27664, #28382, #21740, #72728, #5851, #61997, #22112, #39112, #45021, #66830, #11030, #33553, #56103, #5494, #50562, #73089, #44301, #50920, #17286, #62361, #11757, #4768, #27165, #26799, #72226, #37134, #65949, #71124, #55599, #65578, #33060, #15693, #54503, #43789, #65208, #60389, #4994, #37506, #21605, #59662, #38232, #70756, #15328, #3905, #26059, #21237, #26427, #20496, #44160, #9070, #60762, #20131, #37870, #48968, #48599, #66316, #71497, #43053, #49699, #14968, #66689, #10169, #27526, #42686, #31605, #54142, #60026, #14598, #9438, #31966, #43427, #9797, #20874, #3536, #55240, #32330, #54868, #4635, #38612, #4275, #49333, #71865, #32703, #16063, #61135, #10532, #56678, #38979, #67064, #21972, #12332, #5356, #68144, #23418, #187, #51145, #57031, #72590, #57394, #56328, #28609, #50428, #62583, #44531, #22336, #44888, #55961, #72954, #27894, #6438, #16421, #61495, #6801, #545, #50784, #33785, #50060, #10892, #34867, #33420, #39709, #45965, #67423, #23056, #16785, #39343, #17508, #28973, #40069, #51510, #5717, #910, #62938, #28253, #61856, #11980, #45610, #6076, #11263, #34503, #22692, #45243, #68498, #17862, #67777, #17151, #40421, #62227, #11623, #34139, #42132, #53207, #2973, #8510, #1897, #35130, #53575, #25501, #35490, #52849, #69128, #48046, #2247, #69487, #24036, #36221, #57655, #19206, #70571, #64289, #46950, #19947, #24763, #70200, #41407, #41760, #14043, #52127, #7782, #12953, #42500, #7418, #12598, #30675, #18846, #58737, #7061, #47306, #29589, #52486, #36583, #1529, #2603, #46586, #30319, #63923, #41052, #8148, #13308, #58010, #64658, #29946, #59103, #25124, #18486, #63565, #24401, #35846, #58371, #69841, #13677, #47666, #19576, #31039, #48776, #70939, #49504, #37677, #9247, #72033, #32871, #72392, #8879, #26239, #14412, #66120, #32509, #71300, #71673, #53954, #31414, #36949, #27336, #20310, #9972, #38414, #15139, #15499, #21409, #59469, #21772, #20679, #43599, #65385, #4447, #3351, #37318, #59842, #42863, #14776, #31782, #43966, #25873, #48413, #65023, #38041, #65756, #43236, #54321, #3712, #49868, #60199, #54675, #60935, #9611, #60565, #32142, #4078, #55044, #66487, #26975, #15866, #26606, #10339, #4803, #49144, #21047, #55408, #17321, #50953, #50238, #28774, #10700, #72760, #62393, #39881, #56133, #28065, #351, #55771, #45054, #16592, #16956, #11062, #12147, #67233, #22858, #44699, #38788, #56841, #11791, #16235, #718, #56491, #50595, #22146, #51314, #39509, #61662, #23225, #34674, #51680, #61305, #5527, #66864, #45412, #34308, #28527, #67948, #33233, #5163, #27697, #6618, #39145, #6247, #17673, #67590, #45778, #68313, #33588 ) ),
 .UNSPECIFIED., .F., .F., .F. ) 
 B_SPLINE_SURFACE_WITH_KNOTS ( ( 2, 2 ),
 ( 3, 2, 2, 2, 2, 2, 2, 2, 2, 2, 2, 2, 2, 2, 2, 2, 2, 2, 2, 2, 2, 2, 2, 2, 2, 2, 2, 2, 2, 2, 2, 2, 2, 2, 2, 2, 2, 2, 2, 2, 2, 2, 2, 2, 2, 2, 2, 2, 2, 2, 2, 2, 2, 2, 2, 2, 2, 2, 2, 2, 2, 2, 2, 2, 2, 2, 2, 2, 2, 2, 2, 2, 2, 2, 2, 2, 2, 2, 2, 2, 2, 2, 2, 2, 2, 2, 2, 2, 2, 2, 2, 2, 2, 2, 2, 2, 2, 2, 2, 2, 2, 2, 2, 2, 2, 2, 2, 2, 2, 2, 2, 2, 2, 2, 2, 2, 2, 2, 2, 2, 2, 2, 2, 2, 2, 2, 2, 2, 2, 2, 2, 2, 2, 2, 2, 2, 2, 2, 2, 2, 2, 2, 2, 2, 2, 2, 2, 2, 2, 2, 2, 2, 2, 2, 2, 2, 2, 2, 2, 2, 2, 2, 2, 2, 2, 2, 2, 2, 2, 2, 2, 2, 2, 2, 2, 2, 2, 2, 2, 2, 2, 2, 2, 2, 2, 2, 2, 2, 2, 2, 2, 2, 2, 2, 2, 2, 2, 2, 2, 2, 2, 2, 2, 2, 2, 2, 2, 2, 2, 2, 2, 2, 2, 2, 2, 2, 2, 2, 2, 2, 2, 2, 2, 2, 2, 2, 2, 2, 2, 2, 2, 2, 2, 2, 2, 2, 2, 2, 2, 2, 2, 2, 2, 2, 2, 2, 2, 2, 2, 2, 2, 2, 2, 2, 2, 2, 2, 2, 2, 2, 2, 2, 2, 2, 2, 2, 2, 2, 2, 2, 2, 2, 2, 2, 2, 2, 2, 2, 2, 2, 2, 2, 2, 2, 2, 2, 2, 2, 2, 2, 2, 2, 2, 2, 2, 2, 2, 2, 2, 2, 2, 2, 2, 2, 2, 2, 2, 2, 2, 2, 2, 2, 2, 2, 2, 2, 2, 2, 2, 2, 2, 2, 2, 2, 2, 2, 2, 2, 2, 2, 2, 2, 2, 2, 2, 2, 2, 2, 2, 2, 2, 2, 2, 2, 2, 2, 2, 2, 2, 2, 2, 2, 2, 2, 2, 2, 2, 2, 2, 2, 3 ),
 ( 0.000000000000000000, 1.000000000000000000 ),
 ( 0.000000000000000000, 0.002777777777777777884, 0.005555555555555555768, 0.008333333333333333218, 0.01111111111111111154, 0.01388888888888888812, 0.01666666666666666644, 0.01944444444444444475, 0.02222222222222222307, 0.02500000000000000139, 0.02777777777777777624, 0.03055555555555555455, 0.03333333333333333287, 0.03611111111111110772, 0.03888888888888888951, 0.04166666666666666435, 0.04444444444444444614, 0.04722222222222222099, 0.05000000000000000278, 0.05277777777777777762, 0.05555555555555555247, 0.05833333333333333426, 0.06111111111111110911, 0.06388888888888888395, 0.06666666666666666574, 0.06944444444444444753, 0.07222222222222221544, 0.07499999999999999722, 0.07777777777777777901, 0.08055555555555556080, 0.08333333333333332871, 0.08611111111111111049, 0.08888888888888889228, 0.09166666666666666019, 0.09444444444444444198, 0.09722222222222222376, 0.1000000000000000056, 0.1027777777777777735, 0.1055555555555555552, 0.1083333333333333370, 0.1111111111111111049, 0.1138888888888888867, 0.1166666666666666685, 0.1194444444444444503, 0.1222222222222222182, 0.1250000000000000000, 0.1277777777777777679, 0.1305555555555555636, 0.1333333333333333315, 0.1361111111111110994, 0.1388888888888888951, 0.1416666666666666630, 0.1444444444444444309, 0.1472222222222222265, 0.1499999999999999944, 0.1527777777777777901, 0.1555555555555555580, 0.1583333333333333259, 0.1611111111111111216, 0.1638888888888888895, 0.1666666666666666574, 0.1694444444444444531, 0.1722222222222222210, 0.1749999999999999889, 0.1777777777777777846, 0.1805555555555555525, 0.1833333333333333204, 0.1861111111111111160, 0.1888888888888888840, 0.1916666666666666796, 0.1944444444444444475, 0.1972222222222222154, 0.2000000000000000111, 0.2027777777777777790, 0.2055555555555555469, 0.2083333333333333426, 0.2111111111111111105, 0.2138888888888888784, 0.2166666666666666741, 0.2194444444444444420, 0.2222222222222222099, 0.2250000000000000056, 0.2277777777777777735, 0.2305555555555555691, 0.2333333333333333370, 0.2361111111111111049, 0.2388888888888889006, 0.2416666666666666685, 0.2444444444444444364, 0.2472222222222222321, 0.2500000000000000000, 0.2527777777777777679, 0.2555555555555555358, 0.2583333333333333592, 0.2611111111111111271, 0.2638888888888888951, 0.2666666666666666630, 0.2694444444444444309, 0.2722222222222221988, 0.2750000000000000222, 0.2777777777777777901, 0.2805555555555555580, 0.2833333333333333259, 0.2861111111111110938, 0.2888888888888888618, 0.2916666666666666852, 0.2944444444444444531, 0.2972222222222222210, 0.2999999999999999889, 0.3027777777777777568, 0.3055555555555555802, 0.3083333333333333481, 0.3111111111111111160, 0.3138888888888888840, 0.3166666666666666519, 0.3194444444444444198, 0.3222222222222222432, 0.3250000000000000111, 0.3277777777777777790, 0.3305555555555555469, 0.3333333333333333148, 0.3361111111111111382, 0.3388888888888889062, 0.3416666666666666741, 0.3444444444444444420, 0.3472222222222222099, 0.3499999999999999778, 0.3527777777777778012, 0.3555555555555555691, 0.3583333333333333370, 0.3611111111111111049, 0.3638888888888888729, 0.3666666666666666408, 0.3694444444444444642, 0.3722222222222222321, 0.3750000000000000000, 0.3777777777777777679, 0.3805555555555555358, 0.3833333333333333592, 0.3861111111111111271, 0.3888888888888888951, 0.3916666666666666630, 0.3944444444444444309, 0.3972222222222221988, 0.4000000000000000222, 0.4027777777777777901, 0.4055555555555555580, 0.4083333333333333259, 0.4111111111111110938, 0.4138888888888888618, 0.4166666666666666852, 0.4194444444444444531, 0.4222222222222222210, 0.4249999999999999889, 0.4277777777777777568, 0.4305555555555555802, 0.4333333333333333481, 0.4361111111111111160, 0.4388888888888888840, 0.4416666666666666519, 0.4444444444444444198, 0.4472222222222222432, 0.4500000000000000111, 0.4527777777777777790, 0.4555555555555555469, 0.4583333333333333148, 0.4611111111111111382, 0.4638888888888889062, 0.4666666666666666741, 0.4694444444444444420, 0.4722222222222222099, 0.4749999999999999778, 0.4777777777777778012, 0.4805555555555555691, 0.4833333333333333370, 0.4861111111111111049, 0.4888888888888888729, 0.4916666666666666408, 0.4944444444444444642, 0.4972222222222222321, 0.5000000000000000000, 0.5027777777777777679, 0.5055555555555555358, 0.5083333333333333037, 0.5111111111111110716, 0.5138888888888888395, 0.5166666666666667185, 0.5194444444444444864, 0.5222222222222222543, 0.5250000000000000222, 0.5277777777777777901, 0.5305555555555555580, 0.5333333333333333259, 0.5361111111111110938, 0.5388888888888888618, 0.5416666666666666297, 0.5444444444444443976, 0.5472222222222222765, 0.5500000000000000444, 0.5527777777777778123, 0.5555555555555555802, 0.5583333333333333481, 0.5611111111111111160, 0.5638888888888888840, 0.5666666666666666519, 0.5694444444444444198, 0.5722222222222221877, 0.5749999999999999556, 0.5777777777777777235, 0.5805555555555556024, 0.5833333333333333703, 0.5861111111111111382, 0.5888888888888889062, 0.5916666666666666741, 0.5944444444444444420, 0.5972222222222222099, 0.5999999999999999778, 0.6027777777777777457, 0.6055555555555555136, 0.6083333333333332815, 0.6111111111111111605, 0.6138888888888889284, 0.6166666666666666963, 0.6194444444444444642, 0.6222222222222222321, 0.6250000000000000000, 0.6277777777777777679, 0.6305555555555555358, 0.6333333333333333037, 0.6361111111111110716, 0.6388888888888888395, 0.6416666666666667185, 0.6444444444444444864, 0.6472222222222222543, 0.6500000000000000222, 0.6527777777777777901, 0.6555555555555555580, 0.6583333333333333259, 0.6611111111111110938, 0.6638888888888888618, 0.6666666666666666297, 0.6694444444444443976, 0.6722222222222222765, 0.6750000000000000444, 0.6777777777777778123, 0.6805555555555555802, 0.6833333333333333481, 0.6861111111111111160, 0.6888888888888888840, 0.6916666666666666519, 0.6944444444444444198, 0.6972222222222221877, 0.6999999999999999556, 0.7027777777777777235, 0.7055555555555556024, 0.7083333333333333703, 0.7111111111111111382, 0.7138888888888889062, 0.7166666666666666741, 0.7194444444444444420, 0.7222222222222222099, 0.7249999999999999778, 0.7277777777777777457, 0.7305555555555555136, 0.7333333333333332815, 0.7361111111111111605, 0.7388888888888889284, 0.7416666666666666963, 0.7444444444444444642, 0.7472222222222222321, 0.7500000000000000000, 0.7527777777777777679, 0.7555555555555555358, 0.7583333333333333037, 0.7611111111111110716, 0.7638888888888888395, 0.7666666666666667185, 0.7694444444444444864, 0.7722222222222222543, 0.7750000000000000222, 0.7777777777777777901, 0.7805555555555555580, 0.7833333333333333259, 0.7861111111111110938, 0.7888888888888888618, 0.7916666666666666297, 0.7944444444444443976, 0.7972222222222222765, 0.8000000000000000444, 0.8027777777777778123, 0.8055555555555555802, 0.8083333333333333481, 0.8111111111111111160, 0.8138888888888888840, 0.8166666666666666519, 0.8194444444444444198, 0.8222222222222221877, 0.8249999999999999556, 0.8277777777777777235, 0.8305555555555556024, 0.8333333333333333703, 0.8361111111111111382, 0.8388888888888889062, 0.8416666666666666741, 0.8444444444444444420, 0.8472222222222222099, 0.8499999999999999778, 0.8527777777777777457, 0.8555555555555555136, 0.8583333333333332815, 0.8611111111111111605, 0.8638888888888889284, 0.8666666666666666963, 0.8694444444444444642, 0.8722222222222222321, 0.8750000000000000000, 0.8777777777777777679, 0.8805555555555555358, 0.8833333333333333037, 0.8861111111111110716, 0.8888888888888888395, 0.8916666666666667185, 0.8944444444444444864, 0.8972222222222222543, 0.9000000000000000222, 0.9027777777777777901, 0.9055555555555555580, 0.9083333333333333259, 0.9111111111111110938, 0.9138888888888888618, 0.9166666666666666297, 0.9194444444444443976, 0.9222222222222222765, 0.9250000000000000444, 0.9277777777777778123, 0.9305555555555555802, 0.9333333333333333481, 0.9361111111111111160, 0.9388888888888888840, 0.9416666666666666519, 0.9444444444444444198, 0.9472222222222221877, 0.9499999999999999556, 0.9527777777777777235, 0.9555555555555556024, 0.9583333333333333703, 0.9611111111111111382, 0.9638888888888889062, 0.9666666666666666741, 0.9694444444444444420, 0.9722222222222222099, 0.9749999999999999778, 0.9777777777777777457, 0.9805555555555555136, 0.9833333333333332815, 0.9861111111111111605, 0.9888888888888889284, 0.9916666666666666963, 0.9944444444444444642, 0.9972222222222222321, 1.000000000000000000 ),
 .UNSPECIFIED. ) 
 GEOMETRIC_REPRESENTATION_ITEM ( )  RATIONAL_B_SPLINE_SURFACE ( (
 ( 1.000000000000000000, 0.8660254037844387076, 1.000000000000000000, 0.8660254037844387076, 1.000000000000000000, 0.8660254037844387076, 1.000000000000000000, 0.8660254037844387076, 1.000000000000000000, 0.8660254037844387076, 1.000000000000000000, 0.8660254037844387076, 1.000000000000000000, 0.8660254037844387076, 1.000000000000000000, 0.8660254037844387076, 1.000000000000000000, 0.8660254037844387076, 1.000000000000000000, 0.8660254037844387076, 1.000000000000000000, 0.8660254037844387076, 1.000000000000000000, 0.8660254037844387076, 1.000000000000000000, 0.8660254037844387076, 1.000000000000000000, 0.8660254037844387076, 1.000000000000000000, 0.8660254037844387076, 1.000000000000000000, 0.8660254037844387076, 1.000000000000000000, 0.8660254037844387076, 1.000000000000000000, 0.8660254037844387076, 1.000000000000000000, 0.8660254037844387076, 1.000000000000000000, 0.8660254037844387076, 1.000000000000000000, 0.8660254037844387076, 1.000000000000000000, 0.8660254037844387076, 1.000000000000000000, 0.8660254037844387076, 1.000000000000000000, 0.8660254037844387076, 1.000000000000000000, 0.8660254037844387076, 1.000000000000000000, 0.8660254037844387076, 1.000000000000000000, 0.8660254037844387076, 1.000000000000000000, 0.8660254037844387076, 1.000000000000000000, 0.8660254037844387076, 1.000000000000000000, 0.8660254037844387076, 1.000000000000000000, 0.8660254037844387076, 1.000000000000000000, 0.8660254037844387076, 1.000000000000000000, 0.8660254037844387076, 1.000000000000000000, 0.8660254037844387076, 1.000000000000000000, 0.8660254037844387076, 1.000000000000000000, 0.8660254037844387076, 1.000000000000000000, 0.8660254037844387076, 1.000000000000000000, 0.8660254037844387076, 1.000000000000000000, 0.8660254037844387076, 1.000000000000000000, 0.8660254037844387076, 1.000000000000000000, 0.8660254037844387076, 1.000000000000000000, 0.8660254037844387076, 1.000000000000000000, 0.8660254037844387076, 1.000000000000000000, 0.8660254037844387076, 1.000000000000000000, 0.8660254037844387076, 1.000000000000000000, 0.8660254037844387076, 1.000000000000000000, 0.8660254037844387076, 1.000000000000000000, 0.8660254037844387076, 1.000000000000000000, 0.8660254037844387076, 1.000000000000000000, 0.8660254037844387076, 1.000000000000000000, 0.8660254037844387076, 1.000000000000000000, 0.8660254037844387076, 1.000000000000000000, 0.8660254037844387076, 1.000000000000000000, 0.8660254037844387076, 1.000000000000000000, 0.8660254037844387076, 1.000000000000000000, 0.8660254037844387076, 1.000000000000000000, 0.8660254037844387076, 1.000000000000000000, 0.8660254037844387076, 1.000000000000000000, 0.8660254037844387076, 1.000000000000000000, 0.8660254037844387076, 1.000000000000000000, 0.8660254037844387076, 1.000000000000000000, 0.8660254037844387076, 1.000000000000000000, 0.8660254037844387076, 1.000000000000000000, 0.8660254037844387076, 1.000000000000000000, 0.8660254037844387076, 1.000000000000000000, 0.8660254037844387076, 1.000000000000000000, 0.8660254037844387076, 1.000000000000000000, 0.8660254037844387076, 1.000000000000000000, 0.8660254037844387076, 1.000000000000000000, 0.8660254037844387076, 1.000000000000000000, 0.8660254037844387076, 1.000000000000000000, 0.8660254037844387076, 1.000000000000000000, 0.8660254037844387076, 1.000000000000000000, 0.8660254037844387076, 1.000000000000000000, 0.8660254037844387076, 1.000000000000000000, 0.8660254037844387076, 1.000000000000000000, 0.8660254037844387076, 1.000000000000000000, 0.8660254037844387076, 1.000000000000000000, 0.8660254037844387076, 1.000000000000000000, 0.8660254037844387076, 1.000000000000000000, 0.8660254037844387076, 1.000000000000000000, 0.8660254037844387076, 1.000000000000000000, 0.8660254037844387076, 1.000000000000000000, 0.8660254037844387076, 1.000000000000000000, 0.8660254037844387076, 1.000000000000000000, 0.8660254037844387076, 1.000000000000000000, 0.8660254037844387076, 1.000000000000000000, 0.8660254037844387076, 1.000000000000000000, 0.8660254037844387076, 1.000000000000000000, 0.8660254037844387076, 1.000000000000000000, 0.8660254037844387076, 1.000000000000000000, 0.8660254037844387076, 1.000000000000000000, 0.8660254037844387076, 1.000000000000000000, 0.8660254037844387076, 1.000000000000000000, 0.8660254037844387076, 1.000000000000000000, 0.8660254037844387076, 1.000000000000000000, 0.8660254037844387076, 1.000000000000000000, 0.8660254037844387076, 1.000000000000000000, 0.8660254037844387076, 1.000000000000000000, 0.8660254037844387076, 1.000000000000000000, 0.8660254037844387076, 1.000000000000000000, 0.8660254037844387076, 1.000000000000000000, 0.8660254037844387076, 1.000000000000000000, 0.8660254037844387076, 1.000000000000000000, 0.8660254037844387076, 1.000000000000000000, 0.8660254037844387076, 1.000000000000000000, 0.8660254037844387076, 1.000000000000000000, 0.8660254037844387076, 1.000000000000000000, 0.8660254037844387076, 1.000000000000000000, 0.8660254037844387076, 1.000000000000000000, 0.8660254037844387076, 1.000000000000000000, 0.8660254037844387076, 1.000000000000000000, 0.8660254037844387076, 1.000000000000000000, 0.8660254037844387076, 1.000000000000000000, 0.8660254037844387076, 1.000000000000000000, 0.8660254037844387076, 1.000000000000000000, 0.8660254037844387076, 1.000000000000000000, 0.8660254037844387076, 1.000000000000000000, 0.8660254037844387076, 1.000000000000000000, 0.8660254037844387076, 1.000000000000000000, 0.8660254037844387076, 1.000000000000000000, 0.8660254037844387076, 1.000000000000000000, 0.8660254037844387076, 1.000000000000000000, 0.8660254037844387076, 1.000000000000000000, 0.8660254037844387076, 1.000000000000000000, 0.8660254037844387076, 1.000000000000000000, 0.8660254037844387076, 1.000000000000000000, 0.8660254037844387076, 1.000000000000000000, 0.8660254037844387076, 1.000000000000000000, 0.8660254037844387076, 1.000000000000000000, 0.8660254037844387076, 1.000000000000000000, 0.8660254037844387076, 1.000000000000000000, 0.8660254037844387076, 1.000000000000000000, 0.8660254037844387076, 1.000000000000000000, 0.8660254037844387076, 1.000000000000000000, 0.8660254037844387076, 1.000000000000000000, 0.8660254037844387076, 1.000000000000000000, 0.8660254037844387076, 1.000000000000000000, 0.8660254037844387076, 1.000000000000000000, 0.8660254037844387076, 1.000000000000000000, 0.8660254037844387076, 1.000000000000000000, 0.8660254037844387076, 1.000000000000000000, 0.8660254037844387076, 1.000000000000000000, 0.8660254037844387076, 1.000000000000000000, 0.8660254037844387076, 1.000000000000000000, 0.8660254037844387076, 1.000000000000000000, 0.8660254037844387076, 1.000000000000000000, 0.8660254037844387076, 1.000000000000000000, 0.8660254037844387076, 1.000000000000000000, 0.8660254037844387076, 1.000000000000000000, 0.8660254037844387076, 1.000000000000000000, 0.8660254037844387076, 1.000000000000000000, 0.8660254037844387076, 1.000000000000000000, 0.8660254037844387076, 1.000000000000000000, 0.8660254037844387076, 1.000000000000000000, 0.8660254037844387076, 1.000000000000000000, 0.8660254037844387076, 1.000000000000000000, 0.8660254037844387076, 1.000000000000000000, 0.8660254037844387076, 1.000000000000000000, 0.8660254037844387076, 1.000000000000000000, 0.8660254037844387076, 1.000000000000000000, 0.8660254037844387076, 1.000000000000000000, 0.8660254037844387076, 1.000000000000000000, 0.8660254037844387076, 1.000000000000000000, 0.8660254037844387076, 1.000000000000000000, 0.8660254037844387076, 1.000000000000000000, 0.8660254037844387076, 1.000000000000000000, 0.8660254037844387076, 1.000000000000000000, 0.8660254037844387076, 1.000000000000000000, 0.8660254037844387076, 1.000000000000000000, 0.8660254037844387076, 1.000000000000000000, 0.8660254037844387076, 1.000000000000000000, 0.8660254037844387076, 1.000000000000000000, 0.8660254037844387076, 1.000000000000000000, 0.8660254037844387076, 1.000000000000000000, 0.8660254037844387076, 1.000000000000000000, 0.8660254037844387076, 1.000000000000000000, 0.8660254037844387076, 1.000000000000000000, 0.8660254037844387076, 1.000000000000000000, 0.8660254037844387076, 1.000000000000000000, 0.8660254037844387076, 1.000000000000000000, 0.8660254037844387076, 1.000000000000000000, 0.8660254037844387076, 1.000000000000000000, 0.8660254037844387076, 1.000000000000000000, 0.8660254037844387076, 1.000000000000000000, 0.8660254037844387076, 1.000000000000000000, 0.8660254037844387076, 1.000000000000000000, 0.8660254037844387076, 1.000000000000000000, 0.8660254037844387076, 1.000000000000000000, 0.8660254037844387076, 1.000000000000000000, 0.8660254037844387076, 1.000000000000000000, 0.8660254037844387076, 1.000000000000000000, 0.8660254037844387076, 1.000000000000000000, 0.8660254037844387076, 1.000000000000000000, 0.8660254037844387076, 1.000000000000000000, 0.8660254037844387076, 1.000000000000000000, 0.8660254037844387076, 1.000000000000000000, 0.8660254037844387076, 1.000000000000000000, 0.8660254037844387076, 1.000000000000000000, 0.8660254037844387076, 1.000000000000000000, 0.8660254037844387076, 1.000000000000000000, 0.8660254037844387076, 1.000000000000000000, 0.8660254037844387076, 1.000000000000000000, 0.8660254037844387076, 1.000000000000000000, 0.8660254037844387076, 1.000000000000000000, 0.8660254037844387076, 1.000000000000000000, 0.8660254037844387076, 1.000000000000000000, 0.8660254037844387076, 1.000000000000000000, 0.8660254037844387076, 1.000000000000000000, 0.8660254037844387076, 1.000000000000000000, 0.8660254037844387076, 1.000000000000000000, 0.8660254037844387076, 1.000000000000000000, 0.8660254037844387076, 1.000000000000000000, 0.8660254037844387076, 1.000000000000000000, 0.8660254037844387076, 1.000000000000000000, 0.8660254037844387076, 1.000000000000000000, 0.8660254037844387076, 1.000000000000000000, 0.8660254037844387076, 1.000000000000000000, 0.8660254037844387076, 1.000000000000000000, 0.8660254037844387076, 1.000000000000000000, 0.8660254037844387076, 1.000000000000000000, 0.8660254037844387076, 1.000000000000000000, 0.8660254037844387076, 1.000000000000000000, 0.8660254037844387076, 1.000000000000000000, 0.8660254037844387076, 1.000000000000000000, 0.8660254037844387076, 1.000000000000000000, 0.8660254037844387076, 1.000000000000000000, 0.8660254037844387076, 1.000000000000000000, 0.8660254037844387076, 1.000000000000000000, 0.8660254037844387076, 1.000000000000000000, 0.8660254037844387076, 1.000000000000000000, 0.8660254037844387076, 1.000000000000000000, 0.8660254037844387076, 1.000000000000000000, 0.8660254037844387076, 1.000000000000000000, 0.8660254037844387076, 1.000000000000000000, 0.8660254037844387076, 1.000000000000000000, 0.8660254037844387076, 1.000000000000000000, 0.8660254037844387076, 1.000000000000000000, 0.8660254037844387076, 1.000000000000000000, 0.8660254037844387076, 1.000000000000000000, 0.8660254037844387076, 1.000000000000000000, 0.8660254037844387076, 1.000000000000000000, 0.8660254037844387076, 1.000000000000000000, 0.8660254037844387076, 1.000000000000000000, 0.8660254037844387076, 1.000000000000000000, 0.8660254037844387076, 1.000000000000000000, 0.8660254037844387076, 1.000000000000000000, 0.8660254037844387076, 1.000000000000000000, 0.8660254037844387076, 1.000000000000000000, 0.8660254037844387076, 1.000000000000000000, 0.8660254037844387076, 1.000000000000000000, 0.8660254037844387076, 1.000000000000000000, 0.8660254037844387076, 1.000000000000000000, 0.8660254037844387076, 1.000000000000000000, 0.8660254037844387076, 1.000000000000000000, 0.8660254037844387076, 1.000000000000000000, 0.8660254037844387076, 1.000000000000000000, 0.8660254037844387076, 1.000000000000000000, 0.8660254037844387076, 1.000000000000000000, 0.8660254037844387076, 1.000000000000000000, 0.8660254037844387076, 1.000000000000000000, 0.8660254037844387076, 1.000000000000000000, 0.8660254037844387076, 1.000000000000000000, 0.8660254037844387076, 1.000000000000000000, 0.8660254037844387076, 1.000000000000000000, 0.8660254037844387076, 1.000000000000000000, 0.8660254037844387076, 1.000000000000000000, 0.8660254037844387076, 1.000000000000000000, 0.8660254037844387076, 1.000000000000000000, 0.8660254037844387076, 1.000000000000000000, 0.8660254037844387076, 1.000000000000000000, 0.8660254037844387076, 1.000000000000000000, 0.8660254037844387076, 1.000000000000000000, 0.8660254037844387076, 1.000000000000000000, 0.8660254037844387076, 1.000000000000000000, 0.8660254037844387076, 1.000000000000000000, 0.8660254037844387076, 1.000000000000000000, 0.8660254037844387076, 1.000000000000000000, 0.8660254037844387076, 1.000000000000000000, 0.8660254037844387076, 1.000000000000000000, 0.8660254037844387076, 1.000000000000000000, 0.8660254037844387076, 1.000000000000000000, 0.8660254037844387076, 1.000000000000000000, 0.8660254037844387076, 1.000000000000000000, 0.8660254037844387076, 1.000000000000000000, 0.8660254037844387076, 1.000000000000000000, 0.8660254037844387076, 1.000000000000000000, 0.8660254037844387076, 1.000000000000000000, 0.8660254037844387076, 1.000000000000000000, 0.8660254037844387076, 1.000000000000000000, 0.8660254037844387076, 1.000000000000000000, 0.8660254037844387076, 1.000000000000000000, 0.8660254037844387076, 1.000000000000000000, 0.8660254037844387076, 1.000000000000000000, 0.8660254037844387076, 1.000000000000000000, 0.8660254037844387076, 1.000000000000000000, 0.8660254037844387076, 1.000000000000000000, 0.8660254037844387076, 1.000000000000000000, 0.8660254037844387076, 1.000000000000000000, 0.8660254037844387076, 1.000000000000000000, 0.8660254037844387076, 1.000000000000000000, 0.8660254037844387076, 1.000000000000000000, 0.8660254037844387076, 1.000000000000000000, 0.8660254037844387076, 1.000000000000000000, 0.8660254037844387076, 1.000000000000000000, 0.8660254037844387076, 1.000000000000000000, 0.8660254037844387076, 1.000000000000000000, 0.8660254037844387076, 1.000000000000000000, 0.8660254037844387076, 1.000000000000000000, 0.8660254037844387076, 1.000000000000000000, 0.8660254037844387076, 1.000000000000000000, 0.8660254037844387076, 1.000000000000000000, 0.8660254037844387076, 1.000000000000000000, 0.8660254037844387076, 1.000000000000000000, 0.8660254037844387076, 1.000000000000000000, 0.8660254037844387076, 1.000000000000000000, 0.8660254037844387076, 1.000000000000000000, 0.8660254037844387076, 1.000000000000000000, 0.8660254037844387076, 1.000000000000000000, 0.8660254037844387076, 1.000000000000000000, 0.8660254037844387076, 1.000000000000000000, 0.8660254037844387076, 1.000000000000000000, 0.8660254037844387076, 1.000000000000000000, 0.8660254037844387076, 1.000000000000000000, 0.8660254037844387076, 1.000000000000000000, 0.8660254037844387076, 1.000000000000000000, 0.8660254037844387076, 1.000000000000000000, 0.8660254037844387076, 1.000000000000000000, 0.8660254037844387076, 1.000000000000000000, 0.8660254037844387076, 1.000000000000000000, 0.8660254037844387076, 1.000000000000000000, 0.8660254037844387076, 1.000000000000000000, 0.8660254037844387076, 1.000000000000000000, 0.8660254037844387076, 1.000000000000000000, 0.8660254037844387076, 1.000000000000000000, 0.8660254037844387076, 1.000000000000000000, 0.8660254037844387076, 1.000000000000000000, 0.8660254037844387076, 1.000000000000000000, 0.8660254037844387076, 1.000000000000000000, 0.8660254037844387076, 1.000000000000000000, 0.8660254037844387076, 1.000000000000000000, 0.8660254037844387076, 1.000000000000000000, 0.8660254037844387076, 1.000000000000000000, 0.8660254037844387076, 1.000000000000000000, 0.8660254037844387076, 1.000000000000000000, 0.8660254037844387076, 1.000000000000000000, 0.8660254037844387076, 1.000000000000000000, 0.8660254037844387076, 1.000000000000000000, 0.8660254037844387076, 1.000000000000000000, 0.8660254037844387076, 1.000000000000000000, 0.8660254037844387076, 1.000000000000000000, 0.8660254037844387076, 1.000000000000000000, 0.8660254037844387076, 1.000000000000000000, 0.8660254037844387076, 1.000000000000000000, 0.8660254037844387076, 1.000000000000000000, 0.8660254037844387076, 1.000000000000000000, 0.8660254037844387076, 1.000000000000000000, 0.8660254037844387076, 1.000000000000000000, 0.8660254037844387076, 1.000000000000000000, 0.8660254037844387076, 1.000000000000000000),
 ( 1.000000000000000000, 0.8660254037844387076, 1.000000000000000000, 0.8660254037844387076, 1.000000000000000000, 0.8660254037844387076, 1.000000000000000000, 0.8660254037844387076, 1.000000000000000000, 0.8660254037844387076, 1.000000000000000000, 0.8660254037844387076, 1.000000000000000000, 0.8660254037844387076, 1.000000000000000000, 0.8660254037844387076, 1.000000000000000000, 0.8660254037844387076, 1.000000000000000000, 0.8660254037844387076, 1.000000000000000000, 0.8660254037844387076, 1.000000000000000000, 0.8660254037844387076, 1.000000000000000000, 0.8660254037844387076, 1.000000000000000000, 0.8660254037844387076, 1.000000000000000000, 0.8660254037844387076, 1.000000000000000000, 0.8660254037844387076, 1.000000000000000000, 0.8660254037844387076, 1.000000000000000000, 0.8660254037844387076, 1.000000000000000000, 0.8660254037844387076, 1.000000000000000000, 0.8660254037844387076, 1.000000000000000000, 0.8660254037844387076, 1.000000000000000000, 0.8660254037844387076, 1.000000000000000000, 0.8660254037844387076, 1.000000000000000000, 0.8660254037844387076, 1.000000000000000000, 0.8660254037844387076, 1.000000000000000000, 0.8660254037844387076, 1.000000000000000000, 0.8660254037844387076, 1.000000000000000000, 0.8660254037844387076, 1.000000000000000000, 0.8660254037844387076, 1.000000000000000000, 0.8660254037844387076, 1.000000000000000000, 0.8660254037844387076, 1.000000000000000000, 0.8660254037844387076, 1.000000000000000000, 0.8660254037844387076, 1.000000000000000000, 0.8660254037844387076, 1.000000000000000000, 0.8660254037844387076, 1.000000000000000000, 0.8660254037844387076, 1.000000000000000000, 0.8660254037844387076, 1.000000000000000000, 0.8660254037844387076, 1.000000000000000000, 0.8660254037844387076, 1.000000000000000000, 0.8660254037844387076, 1.000000000000000000, 0.8660254037844387076, 1.000000000000000000, 0.8660254037844387076, 1.000000000000000000, 0.8660254037844387076, 1.000000000000000000, 0.8660254037844387076, 1.000000000000000000, 0.8660254037844387076, 1.000000000000000000, 0.8660254037844387076, 1.000000000000000000, 0.8660254037844387076, 1.000000000000000000, 0.8660254037844387076, 1.000000000000000000, 0.8660254037844387076, 1.000000000000000000, 0.8660254037844387076, 1.000000000000000000, 0.8660254037844387076, 1.000000000000000000, 0.8660254037844387076, 1.000000000000000000, 0.8660254037844387076, 1.000000000000000000, 0.8660254037844387076, 1.000000000000000000, 0.8660254037844387076, 1.000000000000000000, 0.8660254037844387076, 1.000000000000000000, 0.8660254037844387076, 1.000000000000000000, 0.8660254037844387076, 1.000000000000000000, 0.8660254037844387076, 1.000000000000000000, 0.8660254037844387076, 1.000000000000000000, 0.8660254037844387076, 1.000000000000000000, 0.8660254037844387076, 1.000000000000000000, 0.8660254037844387076, 1.000000000000000000, 0.8660254037844387076, 1.000000000000000000, 0.8660254037844387076, 1.000000000000000000, 0.8660254037844387076, 1.000000000000000000, 0.8660254037844387076, 1.000000000000000000, 0.8660254037844387076, 1.000000000000000000, 0.8660254037844387076, 1.000000000000000000, 0.8660254037844387076, 1.000000000000000000, 0.8660254037844387076, 1.000000000000000000, 0.8660254037844387076, 1.000000000000000000, 0.8660254037844387076, 1.000000000000000000, 0.8660254037844387076, 1.000000000000000000, 0.8660254037844387076, 1.000000000000000000, 0.8660254037844387076, 1.000000000000000000, 0.8660254037844387076, 1.000000000000000000, 0.8660254037844387076, 1.000000000000000000, 0.8660254037844387076, 1.000000000000000000, 0.8660254037844387076, 1.000000000000000000, 0.8660254037844387076, 1.000000000000000000, 0.8660254037844387076, 1.000000000000000000, 0.8660254037844387076, 1.000000000000000000, 0.8660254037844387076, 1.000000000000000000, 0.8660254037844387076, 1.000000000000000000, 0.8660254037844387076, 1.000000000000000000, 0.8660254037844387076, 1.000000000000000000, 0.8660254037844387076, 1.000000000000000000, 0.8660254037844387076, 1.000000000000000000, 0.8660254037844387076, 1.000000000000000000, 0.8660254037844387076, 1.000000000000000000, 0.8660254037844387076, 1.000000000000000000, 0.8660254037844387076, 1.000000000000000000, 0.8660254037844387076, 1.000000000000000000, 0.8660254037844387076, 1.000000000000000000, 0.8660254037844387076, 1.000000000000000000, 0.8660254037844387076, 1.000000000000000000, 0.8660254037844387076, 1.000000000000000000, 0.8660254037844387076, 1.000000000000000000, 0.8660254037844387076, 1.000000000000000000, 0.8660254037844387076, 1.000000000000000000, 0.8660254037844387076, 1.000000000000000000, 0.8660254037844387076, 1.000000000000000000, 0.8660254037844387076, 1.000000000000000000, 0.8660254037844387076, 1.000000000000000000, 0.8660254037844387076, 1.000000000000000000, 0.8660254037844387076, 1.000000000000000000, 0.8660254037844387076, 1.000000000000000000, 0.8660254037844387076, 1.000000000000000000, 0.8660254037844387076, 1.000000000000000000, 0.8660254037844387076, 1.000000000000000000, 0.8660254037844387076, 1.000000000000000000, 0.8660254037844387076, 1.000000000000000000, 0.8660254037844387076, 1.000000000000000000, 0.8660254037844387076, 1.000000000000000000, 0.8660254037844387076, 1.000000000000000000, 0.8660254037844387076, 1.000000000000000000, 0.8660254037844387076, 1.000000000000000000, 0.8660254037844387076, 1.000000000000000000, 0.8660254037844387076, 1.000000000000000000, 0.8660254037844387076, 1.000000000000000000, 0.8660254037844387076, 1.000000000000000000, 0.8660254037844387076, 1.000000000000000000, 0.8660254037844387076, 1.000000000000000000, 0.8660254037844387076, 1.000000000000000000, 0.8660254037844387076, 1.000000000000000000, 0.8660254037844387076, 1.000000000000000000, 0.8660254037844387076, 1.000000000000000000, 0.8660254037844387076, 1.000000000000000000, 0.8660254037844387076, 1.000000000000000000, 0.8660254037844387076, 1.000000000000000000, 0.8660254037844387076, 1.000000000000000000, 0.8660254037844387076, 1.000000000000000000, 0.8660254037844387076, 1.000000000000000000, 0.8660254037844387076, 1.000000000000000000, 0.8660254037844387076, 1.000000000000000000, 0.8660254037844387076, 1.000000000000000000, 0.8660254037844387076, 1.000000000000000000, 0.8660254037844387076, 1.000000000000000000, 0.8660254037844387076, 1.000000000000000000, 0.8660254037844387076, 1.000000000000000000, 0.8660254037844387076, 1.000000000000000000, 0.8660254037844387076, 1.000000000000000000, 0.8660254037844387076, 1.000000000000000000, 0.8660254037844387076, 1.000000000000000000, 0.8660254037844387076, 1.000000000000000000, 0.8660254037844387076, 1.000000000000000000, 0.8660254037844387076, 1.000000000000000000, 0.8660254037844387076, 1.000000000000000000, 0.8660254037844387076, 1.000000000000000000, 0.8660254037844387076, 1.000000000000000000, 0.8660254037844387076, 1.000000000000000000, 0.8660254037844387076, 1.000000000000000000, 0.8660254037844387076, 1.000000000000000000, 0.8660254037844387076, 1.000000000000000000, 0.8660254037844387076, 1.000000000000000000, 0.8660254037844387076, 1.000000000000000000, 0.8660254037844387076, 1.000000000000000000, 0.8660254037844387076, 1.000000000000000000, 0.8660254037844387076, 1.000000000000000000, 0.8660254037844387076, 1.000000000000000000, 0.8660254037844387076, 1.000000000000000000, 0.8660254037844387076, 1.000000000000000000, 0.8660254037844387076, 1.000000000000000000, 0.8660254037844387076, 1.000000000000000000, 0.8660254037844387076, 1.000000000000000000, 0.8660254037844387076, 1.000000000000000000, 0.8660254037844387076, 1.000000000000000000, 0.8660254037844387076, 1.000000000000000000, 0.8660254037844387076, 1.000000000000000000, 0.8660254037844387076, 1.000000000000000000, 0.8660254037844387076, 1.000000000000000000, 0.8660254037844387076, 1.000000000000000000, 0.8660254037844387076, 1.000000000000000000, 0.8660254037844387076, 1.000000000000000000, 0.8660254037844387076, 1.000000000000000000, 0.8660254037844387076, 1.000000000000000000, 0.8660254037844387076, 1.000000000000000000, 0.8660254037844387076, 1.000000000000000000, 0.8660254037844387076, 1.000000000000000000, 0.8660254037844387076, 1.000000000000000000, 0.8660254037844387076, 1.000000000000000000, 0.8660254037844387076, 1.000000000000000000, 0.8660254037844387076, 1.000000000000000000, 0.8660254037844387076, 1.000000000000000000, 0.8660254037844387076, 1.000000000000000000, 0.8660254037844387076, 1.000000000000000000, 0.8660254037844387076, 1.000000000000000000, 0.8660254037844387076, 1.000000000000000000, 0.8660254037844387076, 1.000000000000000000, 0.8660254037844387076, 1.000000000000000000, 0.8660254037844387076, 1.000000000000000000, 0.8660254037844387076, 1.000000000000000000, 0.8660254037844387076, 1.000000000000000000, 0.8660254037844387076, 1.000000000000000000, 0.8660254037844387076, 1.000000000000000000, 0.8660254037844387076, 1.000000000000000000, 0.8660254037844387076, 1.000000000000000000, 0.8660254037844387076, 1.000000000000000000, 0.8660254037844387076, 1.000000000000000000, 0.8660254037844387076, 1.000000000000000000, 0.8660254037844387076, 1.000000000000000000, 0.8660254037844387076, 1.000000000000000000, 0.8660254037844387076, 1.000000000000000000, 0.8660254037844387076, 1.000000000000000000, 0.8660254037844387076, 1.000000000000000000, 0.8660254037844387076, 1.000000000000000000, 0.8660254037844387076, 1.000000000000000000, 0.8660254037844387076, 1.000000000000000000, 0.8660254037844387076, 1.000000000000000000, 0.8660254037844387076, 1.000000000000000000, 0.8660254037844387076, 1.000000000000000000, 0.8660254037844387076, 1.000000000000000000, 0.8660254037844387076, 1.000000000000000000, 0.8660254037844387076, 1.000000000000000000, 0.8660254037844387076, 1.000000000000000000, 0.8660254037844387076, 1.000000000000000000, 0.8660254037844387076, 1.000000000000000000, 0.8660254037844387076, 1.000000000000000000, 0.8660254037844387076, 1.000000000000000000, 0.8660254037844387076, 1.000000000000000000, 0.8660254037844387076, 1.000000000000000000, 0.8660254037844387076, 1.000000000000000000, 0.8660254037844387076, 1.000000000000000000, 0.8660254037844387076, 1.000000000000000000, 0.8660254037844387076, 1.000000000000000000, 0.8660254037844387076, 1.000000000000000000, 0.8660254037844387076, 1.000000000000000000, 0.8660254037844387076, 1.000000000000000000, 0.8660254037844387076, 1.000000000000000000, 0.8660254037844387076, 1.000000000000000000, 0.8660254037844387076, 1.000000000000000000, 0.8660254037844387076, 1.000000000000000000, 0.8660254037844387076, 1.000000000000000000, 0.8660254037844387076, 1.000000000000000000, 0.8660254037844387076, 1.000000000000000000, 0.8660254037844387076, 1.000000000000000000, 0.8660254037844387076, 1.000000000000000000, 0.8660254037844387076, 1.000000000000000000, 0.8660254037844387076, 1.000000000000000000, 0.8660254037844387076, 1.000000000000000000, 0.8660254037844387076, 1.000000000000000000, 0.8660254037844387076, 1.000000000000000000, 0.8660254037844387076, 1.000000000000000000, 0.8660254037844387076, 1.000000000000000000, 0.8660254037844387076, 1.000000000000000000, 0.8660254037844387076, 1.000000000000000000, 0.8660254037844387076, 1.000000000000000000, 0.8660254037844387076, 1.000000000000000000, 0.8660254037844387076, 1.000000000000000000, 0.8660254037844387076, 1.000000000000000000, 0.8660254037844387076, 1.000000000000000000, 0.8660254037844387076, 1.000000000000000000, 0.8660254037844387076, 1.000000000000000000, 0.8660254037844387076, 1.000000000000000000, 0.8660254037844387076, 1.000000000000000000, 0.8660254037844387076, 1.000000000000000000, 0.8660254037844387076, 1.000000000000000000, 0.8660254037844387076, 1.000000000000000000, 0.8660254037844387076, 1.000000000000000000, 0.8660254037844387076, 1.000000000000000000, 0.8660254037844387076, 1.000000000000000000, 0.8660254037844387076, 1.000000000000000000, 0.8660254037844387076, 1.000000000000000000, 0.8660254037844387076, 1.000000000000000000, 0.8660254037844387076, 1.000000000000000000, 0.8660254037844387076, 1.000000000000000000, 0.8660254037844387076, 1.000000000000000000, 0.8660254037844387076, 1.000000000000000000, 0.8660254037844387076, 1.000000000000000000, 0.8660254037844387076, 1.000000000000000000, 0.8660254037844387076, 1.000000000000000000, 0.8660254037844387076, 1.000000000000000000, 0.8660254037844387076, 1.000000000000000000, 0.8660254037844387076, 1.000000000000000000, 0.8660254037844387076, 1.000000000000000000, 0.8660254037844387076, 1.000000000000000000, 0.8660254037844387076, 1.000000000000000000, 0.8660254037844387076, 1.000000000000000000, 0.8660254037844387076, 1.000000000000000000, 0.8660254037844387076, 1.000000000000000000, 0.8660254037844387076, 1.000000000000000000, 0.8660254037844387076, 1.000000000000000000, 0.8660254037844387076, 1.000000000000000000, 0.8660254037844387076, 1.000000000000000000, 0.8660254037844387076, 1.000000000000000000, 0.8660254037844387076, 1.000000000000000000, 0.8660254037844387076, 1.000000000000000000, 0.8660254037844387076, 1.000000000000000000, 0.8660254037844387076, 1.000000000000000000, 0.8660254037844387076, 1.000000000000000000, 0.8660254037844387076, 1.000000000000000000, 0.8660254037844387076, 1.000000000000000000, 0.8660254037844387076, 1.000000000000000000, 0.8660254037844387076, 1.000000000000000000, 0.8660254037844387076, 1.000000000000000000, 0.8660254037844387076, 1.000000000000000000, 0.8660254037844387076, 1.000000000000000000, 0.8660254037844387076, 1.000000000000000000, 0.8660254037844387076, 1.000000000000000000, 0.8660254037844387076, 1.000000000000000000, 0.8660254037844387076, 1.000000000000000000, 0.8660254037844387076, 1.000000000000000000, 0.8660254037844387076, 1.000000000000000000, 0.8660254037844387076, 1.000000000000000000, 0.8660254037844387076, 1.000000000000000000, 0.8660254037844387076, 1.000000000000000000, 0.8660254037844387076, 1.000000000000000000, 0.8660254037844387076, 1.000000000000000000, 0.8660254037844387076, 1.000000000000000000, 0.8660254037844387076, 1.000000000000000000, 0.8660254037844387076, 1.000000000000000000, 0.8660254037844387076, 1.000000000000000000, 0.8660254037844387076, 1.000000000000000000, 0.8660254037844387076, 1.000000000000000000, 0.8660254037844387076, 1.000000000000000000, 0.8660254037844387076, 1.000000000000000000, 0.8660254037844387076, 1.000000000000000000, 0.8660254037844387076, 1.000000000000000000, 0.8660254037844387076, 1.000000000000000000, 0.8660254037844387076, 1.000000000000000000, 0.8660254037844387076, 1.000000000000000000, 0.8660254037844387076, 1.000000000000000000, 0.8660254037844387076, 1.000000000000000000, 0.8660254037844387076, 1.000000000000000000, 0.8660254037844387076, 1.000000000000000000, 0.8660254037844387076, 1.000000000000000000, 0.8660254037844387076, 1.000000000000000000, 0.8660254037844387076, 1.000000000000000000, 0.8660254037844387076, 1.000000000000000000, 0.8660254037844387076, 1.000000000000000000, 0.8660254037844387076, 1.000000000000000000, 0.8660254037844387076, 1.000000000000000000, 0.8660254037844387076, 1.000000000000000000, 0.8660254037844387076, 1.000000000000000000, 0.8660254037844387076, 1.000000000000000000, 0.8660254037844387076, 1.000000000000000000, 0.8660254037844387076, 1.000000000000000000, 0.8660254037844387076, 1.000000000000000000, 0.8660254037844387076, 1.000000000000000000, 0.8660254037844387076, 1.000000000000000000, 0.8660254037844387076, 1.000000000000000000, 0.8660254037844387076, 1.000000000000000000, 0.8660254037844387076, 1.000000000000000000, 0.8660254037844387076, 1.000000000000000000, 0.8660254037844387076, 1.000000000000000000, 0.8660254037844387076, 1.000000000000000000, 0.8660254037844387076, 1.000000000000000000, 0.8660254037844387076, 1.000000000000000000, 0.8660254037844387076, 1.000000000000000000, 0.8660254037844387076, 1.000000000000000000, 0.8660254037844387076, 1.000000000000000000, 0.8660254037844387076, 1.000000000000000000, 0.8660254037844387076, 1.000000000000000000, 0.8660254037844387076, 1.000000000000000000, 0.8660254037844387076, 1.000000000000000000, 0.8660254037844387076, 1.000000000000000000, 0.8660254037844387076, 1.000000000000000000, 0.8660254037844387076, 1.000000000000000000, 0.8660254037844387076, 1.000000000000000000) ) ) 
 REPRESENTATION_ITEM ( '' )  SURFACE ( )  );
#71541 = CARTESIAN_POINT ( 'NONE',  ( 5.325000001229033941, 2.886751345948126879, 4.999999999999999112 ) ) ;
#71543 = EDGE_CURVE ( 'NONE', #32563, #58840, #63250, .T. ) ;
#71544 = CARTESIAN_POINT ( 'NONE',  ( 10.24687500061451750, -3.027376345333610441, -5.243569643749999898 ) ) ;
#71545 = CARTESIAN_POINT ( 'NONE',  ( 7.387500001229032165, 6.123233995736764310E-16, -4.999999999999998224 ) ) ;
#71546 = CARTESIAN_POINT ( 'NONE',  ( 10.07812500061451644, -4.541064518000419881, 2.621784821874995952 ) ) ;
#71547 = CARTESIAN_POINT ( 'NONE',  ( 14.97187500061451892, 3.027376345333611329, 5.243569643749999010 ) ) ;
#71548 = CARTESIAN_POINT ( 'NONE',  ( 21.56250000122903288, 0.000000000000000000, 4.999999999999998224 ) ) ;
#71549 = CARTESIAN_POINT ( 'NONE',  ( 9.909375000614517148, 4.541064518000418104, -2.621784821874998173 ) ) ;
#71550 = CARTESIAN_POINT ( 'NONE',  ( 11.50312500061451892, -4.541064518000417216, -2.621784821875001281 ) ) ;
#71551 = CARTESIAN_POINT ( 'NONE',  ( 27.54375000122903216, -2.886751345948125991, -5.000000000000000000 ) ) ;
#71552 = CARTESIAN_POINT ( 'NONE',  ( 22.17187500061451644, 3.027376345333611329, 5.243569643749999010 ) ) ;
#71553 = CARTESIAN_POINT ( 'NONE',  ( 14.17500000000000071, 4.330127018922191873, 2.499999999999999556 ) ) ;
#71554 = CARTESIAN_POINT ( 'NONE',  ( -3.942095835588578900, 3.076014195111398397, 30.69138026080431203 ) ) ;
#71555 = CARTESIAN_POINT ( 'NONE',  ( 8.250000000000000000, 4.330127018922192761, -2.499999999999997780 ) ) ;
#71556 = CARTESIAN_POINT ( 'NONE',  ( 2.121784821875001281, 13.25937500061451857, -26.32496088578401938 ) ) ;
#71557 = CARTESIAN_POINT ( 'NONE',  ( 16.42500000122903359, 2.886751345948129099, -4.999999999999998224 ) ) ;
#71558 = CARTESIAN_POINT ( 'NONE',  ( 8.934375000614517504, 6.421520780324663323E-16, -5.243569643749999010 ) ) ;
#71559 = CARTESIAN_POINT ( 'NONE',  ( 4.243569643749999010, 17.36562500061451786, -32.45002607614398471 ) ) ;
#71560 = CARTESIAN_POINT ( 'NONE',  ( 17.21250000122903145, -4.330127018922190985, -2.500000000000001332 ) ) ;
#71561 = CARTESIAN_POINT ( 'NONE',  ( 9.628125000614517148, -4.541064518000419881, 2.621784821874995952 ) ) ;
#71562 = ORIENTED_EDGE ( 'NONE', *, *, #27156, .F. ) ;
#71563 = CARTESIAN_POINT ( 'NONE',  ( 14.81250000000000000, -5.773502691896255534, -1.060575238724906372E-15 ) ) ;
#71564 = CARTESIAN_POINT ( 'NONE',  ( 17.96249999999999858, -5.773502691896255534, -1.060575238724906372E-15 ) ) ;
#71565 = VECTOR ( 'NONE', #8094, 1000.000000000000000 ) ;
#71566 = CARTESIAN_POINT ( 'NONE',  ( 9.496875000614517504, 6.054752690667223547, 3.707466751127219781E-16 ) ) ;
#71567 = CARTESIAN_POINT ( 'NONE',  ( 2.955228467731844333, 4.033190387708875946, -2.955228467731844333 ) ) ;
#71568 = CARTESIAN_POINT ( 'NONE',  ( 10.20000000122903572, 5.773502691896255534, 3.535250795749688894E-16 ) ) ;
#71569 = CARTESIAN_POINT ( 'NONE',  ( 19.61250000122903359, 4.330127018922192761, -2.499999999999997780 ) ) ;
#71570 = CARTESIAN_POINT ( 'NONE',  ( 14.05312500061451431, 0.000000000000000000, 5.243569643749999010 ) ) ;
#71571 = CARTESIAN_POINT ( 'NONE',  ( 18.47812500061451857, 4.541064518000418104, 2.621784821874999949 ) ) ;
#71572 = CARTESIAN_POINT ( 'NONE',  ( 26.70000000122903572, -2.886751345948125991, -5.000000000000000000 ) ) ;
#71573 = CARTESIAN_POINT ( 'NONE',  ( 2.803125000614518747, 0.000000000000000000, 5.243569643749999010 ) ) ;
#71574 = CARTESIAN_POINT ( 'NONE',  ( 25.53750000000000142, -2.886751345948129988, 4.999999999999997335 ) ) ;
#71575 = CARTESIAN_POINT ( 'NONE',  ( 1.878215178125000495, 13.61562499938548321, 26.74683588394047007 ) ) ;
#71576 = CARTESIAN_POINT ( 'NONE',  ( 24.83437500061451431, 4.541064518000418104, 2.621784821874999949 ) ) ;
#71577 = CARTESIAN_POINT ( 'NONE',  ( 0.000000000000000000, 20.00000000000000000, 30.00000000000000000 ) ) ;
#71578 = CARTESIAN_POINT ( 'NONE',  ( 13.53750000122903430, -4.330127018922194537, 2.499999999999995559 ) ) ;
#71579 = CARTESIAN_POINT ( 'NONE',  ( 4.724999999999999645, 4.330127018922191873, 2.499999999999999556 ) ) ;
#71580 = EDGE_CURVE ( 'NONE', #53469, #47796, #19816, .T. ) ;
#71581 = CARTESIAN_POINT ( 'NONE',  ( 22.64999999999999858, 4.330127018922192761, -2.499999999999997780 ) ) ;
#71582 = CARTESIAN_POINT ( 'NONE',  ( 8.409375000614518925, -4.541064518000417216, -2.621784821875001281 ) ) ;
#71583 = CARTESIAN_POINT ( 'NONE',  ( 25.71562500061451573, 3.027376345333611329, 5.243569643749999010 ) ) ;
#71584 = CARTESIAN_POINT ( 'NONE',  ( 9.356250001229033941, 0.000000000000000000, 4.999999999999998224 ) ) ;
#71585 = CARTESIAN_POINT ( 'NONE',  ( 11.47500000122903252, 2.886751345948129099, -4.999999999999997335 ) ) ;
#71586 = DIRECTION ( 'NONE',  ( -1.000000000000000000, -0.000000000000000000, -0.000000000000000000 ) ) ;
#71587 = CARTESIAN_POINT ( 'NONE',  ( 5.484375000614518214, 4.541064518000418104, 2.621784821874999949 ) ) ;
#71588 = CARTESIAN_POINT ( 'NONE',  ( 9.046875000614518214, 6.054752690667223547, 3.707466751127219781E-16 ) ) ;
#71589 = CARTESIAN_POINT ( 'NONE',  ( 28.50937500061451502, 0.000000000000000000, 5.243569643749999010 ) ) ;
#71590 = CARTESIAN_POINT ( 'NONE',  ( -4.243569643749999898, 11.70312500061459460, 30.00000000000000000 ) ) ;
#71591 = CARTESIAN_POINT ( 'NONE',  ( 21.82499999999999574, 4.330127018922191873, 2.499999999999999556 ) ) ;
#71593 = ADVANCED_FACE ( 'NONE', ( #69883 ), #41093, .F. ) ;
#71592 = CARTESIAN_POINT ( 'NONE',  ( 29.77499999999999858, 6.123233995736764310E-16, -4.999999999999998224 ) ) ;
#71594 = CARTESIAN_POINT ( 'NONE',  ( 5.175000000000002487, 4.330127018922191873, 2.499999999999999556 ) ) ;
#71595 = ORIENTED_EDGE ( 'NONE', *, *, #14306, .F. ) ;
#71596 = CARTESIAN_POINT ( 'NONE',  ( 17.01562500061451644, 3.027376345333613106, -5.243569643749998122 ) ) ;
#71597 = CARTESIAN_POINT ( 'NONE',  ( 11.01562500061451821, -6.054752690667223547, -1.112240025338166033E-15 ) ) ;
#71598 = CARTESIAN_POINT ( 'NONE',  ( 20.29687500061451289, 0.000000000000000000, 4.756430356249998326 ) ) ;
#71599 = CARTESIAN_POINT ( 'NONE',  ( 8.259375000614518569, 0.000000000000000000, 5.243569643749999010 ) ) ;
#71600 = CARTESIAN_POINT ( 'NONE',  ( 22.80000000000000071, 0.000000000000000000, 4.999999999999998224 ) ) ;
#71601 = CARTESIAN_POINT ( 'NONE',  ( 19.83750000122903145, -4.330127018922194537, 2.499999999999995559 ) ) ;
#71602 = DIRECTION ( 'NONE',  ( 0.000000000000000000, 1.000000000000000000, 0.000000000000000000 ) ) ;
#71603 = CARTESIAN_POINT ( 'NONE',  ( 9.759375000614516793, -4.541064518000417216, -2.621784821875001281 ) ) ;
#71604 = CARTESIAN_POINT ( 'NONE',  ( 13.84687500061451537, -3.027376345333610441, -5.243569643749999898 ) ) ;
#71605 = CARTESIAN_POINT ( 'NONE',  ( 24.90937500061451715, 0.000000000000000000, 5.243569643749999010 ) ) ;
#71606 = EDGE_CURVE ( 'NONE', #61419, #8461, #27886, .T. ) ;
#71607 = CARTESIAN_POINT ( 'NONE',  ( 4.321628989681628674, -3.794150667385939979, -3.915477560016185965 ) ) ;
#71608 = ORIENTED_EDGE ( 'NONE', *, *, #16221, .T. ) ;
#71609 = CARTESIAN_POINT ( 'NONE',  ( 13.64999999999999858, 4.330127018922192761, -2.499999999999997780 ) ) ;
#71610 = AXIS2_PLACEMENT_3D ( 'NONE', #52762, #25040, #63115 ) ;
#71611 = CARTESIAN_POINT ( 'NONE',  ( 17.07187500061451502, 3.027376345333613106, -5.243569643749998122 ) ) ;
#71612 = CARTESIAN_POINT ( 'NONE',  ( 9.871875000614517504, 3.027376345333613106, -5.243569643749998122 ) ) ;
#71613 = CARTESIAN_POINT ( 'NONE',  ( 3.756430356250000546, 12.67812499938548143, 27.83122392262697886 ) ) ;
#71614 = CARTESIAN_POINT ( 'NONE',  ( 19.94999999999999929, 4.330127018922192761, -2.499999999999997780 ) ) ;
#71615 = CARTESIAN_POINT ( 'NONE',  ( 4.000000000000000000, 16.10000000000000142, 30.00000000000000000 ) ) ;
#71616 = CARTESIAN_POINT ( 'NONE',  ( 4.243569643749999010, 10.22187500061451892, -32.45002607614398471 ) ) ;
#71617 = CARTESIAN_POINT ( 'NONE',  ( 23.37187500061451573, 2.746126346562645981, -4.756430356249997438 ) ) ;
#71618 = CARTESIAN_POINT ( 'NONE',  ( 12.55312500061451786, 4.541064518000418104, -2.621784821874998173 ) ) ;
#71619 = CARTESIAN_POINT ( 'NONE',  ( 28.50937500061451502, 0.000000000000000000, 5.243569643749999010 ) ) ;
#71620 = CARTESIAN_POINT ( 'NONE',  ( 0.000000000000000000, 20.00000000000000000, -33.99999999999999289 ) ) ;
#71621 = DIRECTION ( 'NONE',  ( 0.000000000000000000, 0.000000000000000000, 1.000000000000000000 ) ) ;
#71622 = CARTESIAN_POINT ( 'NONE',  ( 11.58750000000000036, -2.886751345948129988, 4.999999999999997335 ) ) ;
#71623 = CARTESIAN_POINT ( 'NONE',  ( -3.999999999999999556, 17.37500000122903288, 27.69059892324149530 ) ) ;
#71624 = CARTESIAN_POINT ( 'NONE',  ( 12.26250000122903394, -4.330127018922190985, -2.500000000000001332 ) ) ;
#71625 = CARTESIAN_POINT ( 'NONE',  ( 21.19687500061451502, 6.054752690667223547, 3.707466751127219781E-16 ) ) ;
#71626 = CARTESIAN_POINT ( 'NONE',  ( 16.09687500061452070, -3.027376345333610441, -5.243569643749999898 ) ) ;
#71627 = CARTESIAN_POINT ( 'NONE',  ( -3.999999999999997335, 12.38750000000000107, 32.30940107675850470 ) ) ;
#71628 = EDGE_LOOP ( 'NONE', ( #50061, #65338, #64240, #69600 ) ) ;
#71629 = CARTESIAN_POINT ( 'NONE',  ( 16.56562500061451715, 3.027376345333613106, -5.243569643749998122 ) ) ;
#71630 = CARTESIAN_POINT ( 'NONE',  ( 28.65000000122903145, 5.773502691896255534, 3.535250795749688894E-16 ) ) ;
#71631 = CARTESIAN_POINT ( 'NONE',  ( 18.64687500061451786, -3.027376345333614438, 5.243569643749998122 ) ) ;
#71632 = CARTESIAN_POINT ( 'NONE',  ( 5.090625000614516615, -3.027376345333614438, 5.243569643749998122 ) ) ;
#71633 = CARTESIAN_POINT ( 'NONE',  ( 20.09062500061451573, -3.027376345333610441, -5.243569643749999898 ) ) ;
#71634 = CARTESIAN_POINT ( 'NONE',  ( 1.999999999999998668, 18.50000000000000000, -33.46410161513775705 ) ) ;
#71635 = CARTESIAN_POINT ( 'NONE',  ( 27.72187500061451715, -6.054752690667223547, -1.112240025338166033E-15 ) ) ;
#71636 = CARTESIAN_POINT ( 'NONE',  ( -4.243569643749999898, 13.46562500061451928, 27.54997392385601529 ) ) ;
#71637 = CARTESIAN_POINT ( 'NONE',  ( 16.69687500061451502, 6.054752690667223547, 3.707466751127219781E-16 ) ) ;
#71638 = CARTESIAN_POINT ( 'NONE',  ( 16.50000000122903288, 5.773502691896255534, 3.535250795749688894E-16 ) ) ;
#71639 = CARTESIAN_POINT ( 'NONE',  ( 10.24687500061451573, -2.746126346562641984, -4.756430356249999214 ) ) ;
#71640 = CARTESIAN_POINT ( 'NONE',  ( 1.071796769724490117, 18.89509619066136992, -26.00000000000000000 ) ) ;
#71641 = CARTESIAN_POINT ( 'NONE',  ( 20.40937500061451715, 0.000000000000000000, 5.243569643749999010 ) ) ;
#71642 = CARTESIAN_POINT ( 'NONE',  ( 21.63750000122903572, -4.330127018922194537, 2.499999999999995559 ) ) ;
#71643 = CARTESIAN_POINT ( 'NONE',  ( 23.42812500061451786, 4.541064518000418104, 2.621784821874999949 ) ) ;
#71644 = CARTESIAN_POINT ( 'NONE',  ( 16.58437500061451786, 6.421520780324663323E-16, -5.243569643749999010 ) ) ;
#71645 = CARTESIAN_POINT ( 'NONE',  ( 11.69062500061451360, 6.054752690667223547, 3.707466751127219781E-16 ) ) ;
#71646 = CARTESIAN_POINT ( 'NONE',  ( 4.243569643749999010, 13.82187500061451857, 27.54997392385601174 ) ) ;
#71647 = CARTESIAN_POINT ( 'NONE',  ( 16.97812500061451502, 6.421520780324663323E-16, -5.243569643749999010 ) ) ;
#71648 = CARTESIAN_POINT ( 'NONE',  ( -1.071796769724492115, 17.76740381056766438, 34.00000000000000000 ) ) ;
#71649 = VERTEX_POINT ( 'NONE', #59513 ) ;
#71650 = ORIENTED_EDGE ( 'NONE', *, *, #13859, .F. ) ;
#71651 = CARTESIAN_POINT ( 'NONE',  ( 23.43750000000000000, -2.886751345948125991, -5.000000000000000000 ) ) ;
#71652 = CARTESIAN_POINT ( 'NONE',  ( -2.121784821874996840, 18.58437500061451786, -26.32496088578401583 ) ) ;
#71653 = CARTESIAN_POINT ( 'NONE',  ( 3.824725165337683030, -3.220477823186019606, -4.017693170146901416 ) ) ;
#71654 = CARTESIAN_POINT ( 'NONE',  ( 24.47812500061451502, -4.541064518000419881, 2.621784821874995952 ) ) ;
#71655 = CARTESIAN_POINT ( 'NONE',  ( 6.103125000614515905, -4.541064518000417216, -2.621784821875001281 ) ) ;
#71656 = CARTESIAN_POINT ( 'NONE',  ( 17.47500000122903430, 2.886751345948126879, 4.999999999999999112 ) ) ;
#71657 = CARTESIAN_POINT ( 'NONE',  ( 22.94062500061451715, 6.054752690667223547, 3.707466751127219781E-16 ) ) ;
#71658 = CARTESIAN_POINT ( 'NONE',  ( 23.58749999999999858, 5.773502691896255534, 3.535250795749688894E-16 ) ) ;
#71659 = CARTESIAN_POINT ( 'NONE',  ( 28.75312500061451715, 4.541064518000418104, -2.621784821874998173 ) ) ;
#71660 = CARTESIAN_POINT ( 'NONE',  ( 7.040625000614517681, -3.027376345333610441, -5.243569643749999898 ) ) ;
#71661 = ORIENTED_EDGE ( 'NONE', *, *, #70747, .T. ) ;
#71662 = CARTESIAN_POINT ( 'NONE',  ( 23.91562500061451502, 3.027376345333611329, 5.243569643749999010 ) ) ;
#71663 = CARTESIAN_POINT ( 'NONE',  ( 3.403125000614518836, -4.541064518000417216, -2.621784821875001281 ) ) ;
#71664 = CARTESIAN_POINT ( 'NONE',  ( 12.12187500061451573, 2.746126346562645981, -4.756430356249997438 ) ) ;
#71665 = CYLINDRICAL_SURFACE ( 'NONE', #21731, 4.999999999999998224 ) ;
#71666 = CARTESIAN_POINT ( 'NONE',  ( 3.999999999999999112, 13.58750000122903323, -30.00000000000000000 ) ) ;
#71667 = CARTESIAN_POINT ( 'NONE',  ( 13.55625000122903323, -4.330127018922190985, -2.500000000000001332 ) ) ;
#71668 = CARTESIAN_POINT ( 'NONE',  ( 11.77500000000000036, 6.123233995736764310E-16, -4.999999999999998224 ) ) ;
#71669 = ADVANCED_FACE ( 'NONE', ( #48457 ), #15545, .F. ) ;
#71670 = CARTESIAN_POINT ( 'NONE',  ( 11.40937500061451892, 0.000000000000000000, 5.243569643749999010 ) ) ;
#71671 = CARTESIAN_POINT ( 'NONE',  ( 5.400000001229032343, -2.886751345948129988, 4.999999999999997335 ) ) ;
#71672 = CARTESIAN_POINT ( 'NONE',  ( 15.00937500061451679, 0.000000000000000000, 5.243569643749999010 ) ) ;
#71673 = CARTESIAN_POINT ( 'NONE',  ( 6.646875000614518747, -3.027376345333610441, -5.243569643749999898 ) ) ;
#71674 = LINE ( 'NONE', #66121, #38507 ) ;
#71675 = CARTESIAN_POINT ( 'NONE',  ( 10.76250000122903572, 0.000000000000000000, 4.999999999999998224 ) ) ;
#71677 = ADVANCED_FACE ( 'NONE', ( #8556 ), #21094, .F. ) ;
#71676 = CARTESIAN_POINT ( 'NONE',  ( 11.67187500061451821, 3.027376345333613106, -5.243569643749998122 ) ) ;
#71678 = CARTESIAN_POINT ( 'NONE',  ( 21.97500000122902364, 2.886751345948161074, 4.999999999999941380 ) ) ;
#71679 = CARTESIAN_POINT ( 'NONE',  ( 22.22812500061451502, -4.541064518000419881, 2.621784821874995952 ) ) ;
#71680 = CARTESIAN_POINT ( 'NONE',  ( -4.243569643749998122, 10.89687500061451786, 32.45002607614398471 ) ) ;
#71681 = CARTESIAN_POINT ( 'NONE',  ( 20.08125000122903359, 4.330127018922191873, 2.499999999999999556 ) ) ;
#71682 = CARTESIAN_POINT ( 'NONE',  ( 23.97187500061451360, 3.027376345333611329, 5.243569643749999010 ) ) ;
#71683 =( BOUNDED_CURVE ( )  B_SPLINE_CURVE ( 2, ( #36381, #53007, #71095, #52644, #2767, #13842, #13110 ),
 .UNSPECIFIED., .F., .F. ) 
 B_SPLINE_CURVE_WITH_KNOTS ( ( 3, 2, 2, 3 ),
 ( 0.9599999999999999645, 0.9633333333333333748, 0.9666666666666666741, 0.9699999999999999734 ),
 .UNSPECIFIED. ) 
 CURVE ( )  GEOMETRIC_REPRESENTATION_ITEM ( )  RATIONAL_B_SPLINE_CURVE ( ( 1.000000000000000000, 0.8660254037844387076, 1.000000000000000000, 0.8660254037844387076, 1.000000000000000000, 0.8660254037844387076, 1.000000000000000000 ) ) 
 REPRESENTATION_ITEM ( '' )  );
#71684 = ADVANCED_FACE ( 'NONE', ( #59147 ), #31825, .F. ) ;
#71685 = CARTESIAN_POINT ( 'NONE',  ( 4.104815315424666267, 2.854990486726923571, -4.236757528529293992 ) ) ;
#71686 = CARTESIAN_POINT ( 'NONE',  ( 3.028125000614518392, 6.421520780324663323E-16, -5.243569643749999010 ) ) ;
#71687 = CARTESIAN_POINT ( 'NONE',  ( 19.20937500061451786, 2.746126346562645981, -4.756430356249997438 ) ) ;
#71688 = CARTESIAN_POINT ( 'NONE',  ( 25.26562500061451289, 3.027376345333611329, 5.243569643749999010 ) ) ;
#71689 = CARTESIAN_POINT ( 'NONE',  ( 18.17812500061451786, -4.541064518000419881, 2.621784821874995952 ) ) ;
#71690 = CARTESIAN_POINT ( 'NONE',  ( 14.79375000122903216, -2.886751345948129988, 4.999999999999997335 ) ) ;
#71691 = CARTESIAN_POINT ( 'NONE',  ( 14.85937500061451644, 4.541064518000418104, -2.621784821874998173 ) ) ;
#71692 = CARTESIAN_POINT ( 'NONE',  ( -1.071796769724486120, 15.96740381056766722, 34.00000000000000000 ) ) ;
#71693 = CARTESIAN_POINT ( 'NONE',  ( 28.31250000122903288, 0.000000000000000000, 4.999999999999998224 ) ) ;
#71694 = CARTESIAN_POINT ( 'NONE',  ( 5.971875000614516260, 3.027376345333611329, 5.243569643749999010 ) ) ;
#71695 = CARTESIAN_POINT ( 'NONE',  ( 16.95937500061451786, -4.541064518000417216, -2.621784821875001281 ) ) ;
#71696 = CARTESIAN_POINT ( 'NONE',  ( 25.27499999999999858, 6.123233995736764310E-16, -4.999999999999998224 ) ) ;
#71697 = CARTESIAN_POINT ( 'NONE',  ( 23.28750000000000142, -2.886751345948129988, 4.999999999999997335 ) ) ;
#71698 = CARTESIAN_POINT ( 'NONE',  ( 2.850000001229036073, -2.886751345948125991, -5.000000000000000000 ) ) ;
#71699 = CARTESIAN_POINT ( 'NONE',  ( 25.54687500061451644, -3.027376345333610441, -5.243569643749999898 ) ) ;
#71700 = CARTESIAN_POINT ( 'NONE',  ( 15.72187500061451892, 3.027376345333613106, -5.243569643749998122 ) ) ;
#71701 = CARTESIAN_POINT ( 'NONE',  ( 4.000000000000000000, 15.68750000000000000, 27.69059892324149885 ) ) ;
#71702 = CARTESIAN_POINT ( 'NONE',  ( 29.32499999999999929, 6.123233995736764310E-16, -4.999999999999998224 ) ) ;
#71703 = CARTESIAN_POINT ( 'NONE',  ( 6.262500000000000178, -5.773502691896255534, -1.060575238724906372E-15 ) ) ;
#71704 = CARTESIAN_POINT ( 'NONE',  ( 8.709375000614516082, -5.492252693125287522, -1.008910452111647106E-15 ) ) ;
#71705 = CARTESIAN_POINT ( 'NONE',  ( 18.51562500061451289, 3.027376345333611329, 5.243569643749999010 ) ) ;
#71706 = CARTESIAN_POINT ( 'NONE',  ( 9.975000000000001421, 6.123233995736764310E-16, -4.999999999999998224 ) ) ;
#71707 = CARTESIAN_POINT ( 'NONE',  ( 3.365625000614516082, -6.054752690667223547, -1.112240025338166033E-15 ) ) ;
#71708 = CARTESIAN_POINT ( 'NONE',  ( 20.13749999999999929, -2.886751345948129988, 4.999999999999997335 ) ) ;
#71709 = LINE ( 'NONE', #43269, #30121 ) ;
#71710 = CARTESIAN_POINT ( 'NONE',  ( 24.07500000122903216, 2.886751345948129099, -4.999999999999998224 ) ) ;
#71711 = CARTESIAN_POINT ( 'NONE',  ( 0.000000000000000000, 27.50000000000000000, 30.00000000000000000 ) ) ;
#71712 = CARTESIAN_POINT ( 'NONE',  ( 28.50937500061451502, 0.000000000000000000, 5.243569643749999010 ) ) ;
#71713 = ORIENTED_EDGE ( 'NONE', *, *, #68005, .F. ) ;
#71714 = CARTESIAN_POINT ( 'NONE',  ( 17.95312500061451644, 4.541064518000418104, -2.621784821874998173 ) ) ;
#71715 = CARTESIAN_POINT ( 'NONE',  ( 23.91562500061451502, 3.027376345333611329, 5.243569643749999010 ) ) ;
#71716 = CARTESIAN_POINT ( 'NONE',  ( 23.74687500061451573, -3.027376345333610441, -5.243569643749999898 ) ) ;
#71717 = CARTESIAN_POINT ( 'NONE',  ( 9.787499999999999645, -2.886751345948129988, 4.999999999999997335 ) ) ;
#71718 = CARTESIAN_POINT ( 'NONE',  ( 11.87812500061451537, -4.541064518000419881, 2.621784821874995952 ) ) ;
#71719 = CARTESIAN_POINT ( 'NONE',  ( 27.25312500061451360, -4.541064518000417216, -2.621784821875001281 ) ) ;
#71720 = CARTESIAN_POINT ( 'NONE',  ( 13.99687500061451928, 6.054752690667223547, 3.707466751127219781E-16 ) ) ;
#71721 = CARTESIAN_POINT ( 'NONE',  ( 19.47187500061451360, 3.027376345333611329, 5.243569643749999010 ) ) ;
#71722 = CARTESIAN_POINT ( 'NONE',  ( 4.000000000000000000, 14.69374999877096677, 30.00000000000000000 ) ) ;
#71723 = CARTESIAN_POINT ( 'NONE',  ( -2.121784821874999949, 19.27812500061451573, 26.32496088578401938 ) ) ;
#71724 = EDGE_CURVE ( 'NONE', #10011, #42322, #38688, .T. ) ;
#71725 = AXIS2_PLACEMENT_3D ( 'NONE', #27193, #67807, #17181 ) ;
#71726 = CARTESIAN_POINT ( 'NONE',  ( 23.47500000122903430, -5.773502691896255534, -1.060575238724906372E-15 ) ) ;
#71727 = CARTESIAN_POINT ( 'NONE',  ( 17.70937500061451431, 0.000000000000000000, 4.756430356249998326 ) ) ;
#71728 = CARTESIAN_POINT ( 'NONE',  ( 13.75312500061451715, -4.541064518000417216, -2.621784821875001281 ) ) ;
#71729 = CARTESIAN_POINT ( 'NONE',  ( 7.546875000614517326, -3.027376345333610441, -5.243569643749999898 ) ) ;
#71730 = CARTESIAN_POINT ( 'NONE',  ( 7.059375000614518392, -4.541064518000417216, -2.621784821875001281 ) ) ;
#71731 = EDGE_LOOP ( 'NONE', ( #5947, #28661, #1761, #22211 ) ) ;
#71732 = CARTESIAN_POINT ( 'NONE',  ( 27.42187500061451644, 3.027376345333613106, -5.243569643749998122 ) ) ;
#71733 = CARTESIAN_POINT ( 'NONE',  ( 19.60312500061451502, -4.541064518000417216, -2.621784821875001281 ) ) ;
#71734 = CARTESIAN_POINT ( 'NONE',  ( 29.27812500061451573, 4.541064518000418104, 2.621784821874999949 ) ) ;
#71735 = CARTESIAN_POINT ( 'NONE',  ( 25.39687500061451431, -3.027376345333614438, 5.243569643749998122 ) ) ;
#71736 = CARTESIAN_POINT ( 'NONE',  ( 20.61562500061451431, 3.027376345333613106, -5.243569643749998122 ) ) ;
#71737 = CARTESIAN_POINT ( 'NONE',  ( -2.000000000000000000, 11.37500000000000178, 26.53589838486224650 ) ) ;
#71738 = CARTESIAN_POINT ( 'NONE',  ( 25.49062500061451786, -3.027376345333610441, -5.243569643749999898 ) ) ;
#71739 = CARTESIAN_POINT ( 'NONE',  ( 7.050000001229036251, 5.773502691896255534, 3.535250795749688894E-16 ) ) ;
#71740 = ORIENTED_EDGE ( 'NONE', *, *, #15748, .T. ) ;
#71741 = CARTESIAN_POINT ( 'NONE',  ( 2.812500001229033320, -4.330127018922190985, -2.500000000000001332 ) ) ;
#71742 = CARTESIAN_POINT ( 'NONE',  ( 2.000000000000001332, 14.30000000000000071, -26.53589838486224650 ) ) ;
#71743 = CARTESIAN_POINT ( 'NONE',  ( 21.78750000122903074, 6.123233995736764310E-16, -4.999999999999998224 ) ) ;
#71744 = CARTESIAN_POINT ( 'NONE',  ( 3.756430356249998770, 15.41562499938548392, 32.16877607737302469 ) ) ;
#71745 = CARTESIAN_POINT ( 'NONE',  ( 4.996875000614516615, 6.054752690667223547, 3.707466751127219781E-16 ) ) ;
#71746 = CARTESIAN_POINT ( 'NONE',  ( 20.45625000122903359, 4.330127018922192761, -2.499999999999997780 ) ) ;
#71747 = CARTESIAN_POINT ( 'NONE',  ( 13.56562500061451892, 3.027376345333611329, 5.243569643749999010 ) ) ;
#71748 = CARTESIAN_POINT ( 'NONE',  ( 9.346875000614517148, -3.027376345333610441, -5.243569643749999898 ) ) ;
#71749 = CARTESIAN_POINT ( 'NONE',  ( 23.88750000122903216, -4.330127018922194537, 2.499999999999995559 ) ) ;
#71750 =( BOUNDED_CURVE ( )  B_SPLINE_CURVE ( 2, ( #23461, #51909, #12734, #18628, #24179, #51552, #40464, #30091, #1670 ),
 .UNSPECIFIED., .F., .F. ) 
 B_SPLINE_CURVE_WITH_KNOTS ( ( 3, 2, 2, 2, 3 ),
 ( 0.07608695652173913526, 0.07971014492753622505, 0.08695652173913043237, 0.09420289855072463969, 0.09782608695652174335 ),
 .UNSPECIFIED. ) 
 CURVE ( )  GEOMETRIC_REPRESENTATION_ITEM ( )  RATIONAL_B_SPLINE_CURVE ( ( 0.9330127018922192983, 0.9330127018922194093, 1.000000000000000000, 0.8660254037844387076, 1.000000000000000000, 0.8660254037844387076, 1.000000000000000000, 0.9330127018922194093, 0.9330127018922194093 ) ) 
 REPRESENTATION_ITEM ( '' )  );
#71751 = CARTESIAN_POINT ( 'NONE',  ( 15.42187500061451821, 3.027376345333611329, 5.243569643749999010 ) ) ;
#71752 = CARTESIAN_POINT ( 'NONE',  ( 29.57812500061451644, 6.421520780324663323E-16, -5.243569643749999010 ) ) ;
#71753 = DIRECTION ( 'NONE',  ( -1.000000000000000000, -0.000000000000000000, -0.000000000000000000 ) ) ;
#71754 = CARTESIAN_POINT ( 'NONE',  ( 4.265625000614517326, -6.054752690667223547, -1.112240025338166033E-15 ) ) ;
#71755 = CARTESIAN_POINT ( 'NONE',  ( 14.16562500061451679, -6.054752690667223547, -1.112240025338166033E-15 ) ) ;
#71756 = EDGE_LOOP ( 'NONE', ( #10119, #39435, #12184, #15842 ) ) ;
#71757 = CARTESIAN_POINT ( 'NONE',  ( 12.25312500061451537, 0.000000000000000000, 5.243569643749999010 ) ) ;
#71758 = CARTESIAN_POINT ( 'NONE',  ( 8.240625000614516082, -3.027376345333614438, 5.243569643749998122 ) ) ;
#71759 = CARTESIAN_POINT ( 'NONE',  ( 19.73437500061451644, 5.824947211148865298E-16, -4.756430356249998326 ) ) ;
#71760 = CARTESIAN_POINT ( 'NONE',  ( 7.912499999999999645, 2.886751345948126879, 4.999999999999999112 ) ) ;
#71761 = CARTESIAN_POINT ( 'NONE',  ( 3.975000001229033852, 2.886751345948126879, 4.999999999999999112 ) ) ;
#71762 = CARTESIAN_POINT ( 'NONE',  ( 17.77499999999999858, 4.330127018922191873, 2.499999999999999556 ) ) ;
#71763 = CARTESIAN_POINT ( 'NONE',  ( 18.49687500061452283, 6.054752690667223547, 3.707466751127219781E-16 ) ) ;
#71764 = CARTESIAN_POINT ( 'NONE',  ( 13.08750000122903323, -4.330127018922194537, 2.499999999999995559 ) ) ;
#71765 = CARTESIAN_POINT ( 'NONE',  ( 22.50000000000000000, -4.330127018922190985, -2.500000000000001332 ) ) ;
#71766 = CARTESIAN_POINT ( 'NONE',  ( -3.000416591977282496E-16, 17.44062500061451360, -34.90005215228797653 ) ) ;
#71767 = CARTESIAN_POINT ( 'NONE',  ( -1.999999999999997113, 16.92500000000000426, 33.46410161513775705 ) ) ;
#71768 = CARTESIAN_POINT ( 'NONE',  ( 14.45625000122903359, -4.330127018922190985, -2.500000000000001332 ) ) ;
#71769 = CARTESIAN_POINT ( 'NONE',  ( 28.64062500061451289, -3.027376345333610441, -5.243569643749999898 ) ) ;
#71770 = FACE_OUTER_BOUND ( 'NONE', #55346, .T. ) ;
#71771 = CARTESIAN_POINT ( 'NONE',  ( 24.22500000000000142, -4.330127018922194537, 2.499999999999995559 ) ) ;
#71772 = CARTESIAN_POINT ( 'NONE',  ( 14.07187500061451679, 3.027376345333611329, 5.243569643749999010 ) ) ;
#71773 = EDGE_CURVE ( 'NONE', #35438, #26212, #47031, .T. ) ;
#71774 = CARTESIAN_POINT ( 'NONE',  ( 27.63749999999999929, 5.773502691896255534, 3.535250795749688894E-16 ) ) ;
#71775 = CARTESIAN_POINT ( 'NONE',  ( 12.55312500061451786, 4.541064518000418104, -2.621784821874998173 ) ) ;
#71776 = CARTESIAN_POINT ( 'NONE',  ( 27.94687500061451502, 0.000000000000000000, 4.756430356249998326 ) ) ;
#71777 =( BOUNDED_SURFACE ( )  B_SPLINE_SURFACE ( 1, 2, ( 
 ( #50690, #92, #22598, #45149, #17053, #32236, #62486, #34408, #40324, #51773, #7068, #1904, #57662, #51049, #29596, #68768, #7425, #63209, #28871, #445, #18852, #52133, #34045, #22953, #62131, #62846, #12239, #35137, #29953, #12960, #45515, #56936, #5981, #68045, #813, #1536, #39972, #46229, #6707, #24044, #46593, #17415, #11883, #18125, #51410, #6341, #69135, #1173, #17764, #18494, #40691, #23320, #45870, #68403, #56584, #34770, #12604, #57303, #35497, #28511, #41059, #52493, #63572, #29240, #23681, #58017, #24408, #46958, #69494, #11523, #36956, #59477, #64666, #8155, #26247, #8889, #70947, #59850, #58745, #63930, #3720, #31047, #25133, #14050, #14422, #35854, #7788, #53585, #19584, #36591, #42140, #42872, #69847, #13315, #2980, #19213, #70579, #41414, #59112, #25881, #30326, #47313, #31422, #53962, #25509, #8518, #9255, #58377, #48420, #48054, #70209, #3359, #19954, #2255, #24770, #52856, #41768, #47674, #42507, #65030, #65394, #64297, #20318, #31790, #14785, #13685, #36229, #30684, #53215, #2611, #37327, #54328, #48784, #71309, #43974, #60573, #5536, #38797, #50247, #39154, #38048, #43244, #56142, #10348, #4455, #66493, #66873, #15147, #60207, #32878, #72040, #15876, #21417, #22154, #49153, #65765, #55417, #71682, #49875, #20686, #38422, #5171, #9619, #26616, #61313, #33242, #4812, #60944, #61671, #37684, #44707, #32151, #27344, #72400, #16242, #21781, #44346, #9980, #10709, #72769, #54684, #67242, #4086, #21056, #55779, #28073, #27706, #16600, #26984, #43607, #66128, #11070, #15507, #32517, #33597, #55054, #49513, #50601, #34316, #23235, #6626, #6981, #57212, #39517, #29155, #17681, #35050, #12155, #45421, #62044, #23956, #51687, #22513, #11439, #6, #6255, #28783, #1091, #29512, #57578, #33958, #67957, #56497, #5892, #62401, #23599, #50960, #62763, #45786, #46144, #68683, #28423, #358, #40240, #39888, #22865, #45060, #52047, #51323, #63123, #1451, #11799, #17329, #56849, #34682, #67597, #727, #68321, #18044, #40601, #12519, #16963, #32555, #60987, #60610, #66533, #4848, #33280, #28112, #10747, #4126, #55819, #21822, #33638, #16280, #55092, #26655, #45098, #5206, #60242, #49191, #15183, #15913, #38461, #61351, #56182, #39195, #71721, #10019, #32190, #21093, #27021, #27747, #66168, #72438, #32918, #50286, #72810, #43644, #15544, #44387, #4492, #38088, #22193, #27382, #44011, #44747, #66912, #49553, #72075, #21456, #9656, #10386, #38836, #55455, #61710, #54723, #67281, #5575, #16640, #49914, #11109, #50641, #45, #22550, #37722, #41010, #63159, #12554, #17717, #34354, #52447, #35088, #23995, #12912, #11836, #17000, #29907, #57248, #51359, #40277, #40640, #62082, #33998, #6661, #45820, #62798, #68356, #69084, #22902, #39557, #29190, #45461, #23634, #67633, #12191, #52084, #56535, #395, #57614, #7017, #51724, #34718, #35445, #11475, #18445, #5928, #1125, #46180, #29548, #68719, #18079, #56887, #1489, #46543, #63525, #762, #28462, #67993, #39924, #7376, #24360, #62438, #17367, #57969, #6292, #1853, #50997, #28821, #23270, #10215, #42373, #43101, #43472, #65627, #20543, #4680, #32748, #14645, #36822, #32376, #54916, #60807, #37919, #15377, #32015, #15014, #71547, #37552, #60074, #9486, #55286, #66365, #3216, #65996, #31281, #60437, #31655, #48646, #20920, #53823, #9117, #37186, #25745, #14285, #54188, #54550, #47916, #70445, #20181, #3585, #3952, #26107, #26475, #49015, #19821, #9847, #59337, #49381, #71171, #64895, #4323, #26848, #8748, #42736, #48282, #71911, #70806, #21285, #43838, #59710, #15740, #38279, #65255, #33463, #33106, #22021, #67470, #5403, #22739, #5040, #33831, #50472, #67824, #57077, #12024, #44207, #16833, #27939, #72999, #40114, #22383, #38661, #55645, #27576, #51191, #61905, #5766, #34548, #6122, #50108, #66739, #72637, #27210, #11310, #16466, #45290, #39757, #44577, #44932, #10940, #49745, #17553, #39386, #56720, #595, #39025, #16110, #61539, #56374, #68189, #67110, #28297, #50832, #28652, #56009, #72273, #232, #17197, #62275, #21650, #11669, #34185, #61184, #23099, #45657, #62629, #10579, #29734, #24908, #51555, #7927, #17907, #52272, #13097, #2038, #41197, #24183, #23821, #24549, #58517, #957, #52994, #40469, #6485, #1674, #41911, #13449, #58157, #63354, #46011, #62984, #63705, #68548, #51914, #35635, #46372, #46736, #1312, #57796, #69270, #47094, #19354, #69627, #12379, #18989, #7561, #47452, #30096, #68906, #34916, #36368, #41551, #23465, #57443, #29020, #7205, #18632, #52632, #69984, #30464, #6846, #18263, #29381, #40837, #12738, #64068, #35275, #35998, #2390, #64436, #13828, #19727, #70351, #43009, #48188, #42278, #43383, #71082, #14558, #20830, #65538, #64801, #14192, #47820, #30824, #65167, #59985, #31561, #9755, #2754, #48924, #49290, #37466, #53356, #31187, #53729, #36727, #59249, #37092, #32289, #54462, #3860, #9031, #25651, #43746, #26383, #15287, #4231, #3122, #8293, #21195, #48555, #42643, #54100, #31926, #25273, #8657, #20456, #59616, #15649, #14925, #70712, #60346, #3498, #58883, #26016, #9396, #20086, #71455, #65907, #37827, #54823, #26758, #71823, #66271, #5678, #10848, #4953, #44488, #44116, #33018, #5313, #16381, #33743, #16020, #44846, #61454, #28214, #68100, #23010, #55198, #27855, #38936, #33382, #51104, #55918, #49655, #66643, #38568, #62185, #72912, #16744, #45569, #17106, #61092, #4592, #10491, #38189, #22294, #27486, #56288, #50743, #55557, #50387, #21932, #60714, #28568, #67382, #67733, #11582, #50020, #27121, #72544, #39299, #6034, #67020, #61814, #11217, #146, #72183, #22652, #45201, #500, #10126, #39666, #34098, #56638, #32658, #21562, #69185, #41463, #29647, #52907, #11936, #12653, #13010, #35188, #63261, #47367, #2305, #57353, #6396, #1953, #24460, #30378, #7477, #58067, #1587, #57713, #41110 ),
 ( #62539, #23731, #18545, #7118, #63982, #34461, #35548, #52185, #24097, #34825, #30004, #69543, #56989, #13364, #28927, #17466, #46644, #24820, #47008, #63620, #1225, #51464, #867, #52546, #23374, #62896, #18902, #6758, #35906, #12291, #68820, #58430, #7841, #40025, #45922, #68454, #17816, #40377, #29292, #51822, #46280, #18177, #40745, #37377, #41818, #30735, #69898, #48102, #70625, #42921, #15199, #20738, #8206, #64716, #13740, #58796, #8570, #65445, #47725, #54014, #14471, #59901, #31840, #53267, #2665, #3410, #59162, #25182, #54376, #8940, #25561, #3771, #25930, #70264, #19635, #42192, #64349, #3030, #70994, #42553, #43296, #36282, #9306, #60257, #48470, #14100, #36640, #31098, #53638, #20000, #65080, #65817, #14836, #26296, #37005, #59528, #54738, #48833, #71364, #37737, #31471, #19264, #32204, #20370, #9671, #4140, #26671, #43661, #15561, #38852, #27400, #44403, #49930, #50657, #4509, #71738, #61367, #27038, #5222, #49204, #21840, #33654, #38104, #55109, #67298, #61726, #10764, #72455, #67650, #21108, #61, #60626, #66929, #55835, #49569, #16656, #11127, #33297, #16298, #17016, #66183, #22567, #10037, #27764, #50304, #44763, #72826, #22209, #66550, #39214, #28129, #32571, #45115, #72091, #21475, #56199, #11492, #5592, #39575, #32934, #44028, #15930, #62098, #38479, #61003, #34014, #10402, #56551, #55472, #5945, #4864, #46557, #41381, #24009, #17382, #69099, #35103, #46922, #29562, #68372, #39940, #58343, #18461, #411, #62453, #28478, #6676, #29204, #1504, #69460, #52461, #11851, #23287, #45478, #34370, #40292, #41024, #6308, #12569, #46194, #63540, #12926, #56903, #28837, #57628, #17733, #51376, #35461, #40654, #57264, #57983, #7033, #778, #45835, #62814, #22920, #34734, #52099, #1139, #1868, #68010, #7393, #18818, #29921, #12206, #51740, #23650, #68735, #18093, #63175, #24374, #63893, #13283, #35821, #51015, #65729, #25847, #37291, #26210, #25098, #30290, #43209, #70545, #64632, #53548, #53926, #2224, #47281, #19920, #59077, #2945, #8481, #9219, #36193, #52822, #42474, #58711, #36922, #7754, #25473, #65359, #69815, #70175, #48384, #20283, #8123, #31015, #14018, #37651, #71273, #48019, #59814, #31756, #19552, #19181, #42109, #64997, #48749, #30650, #14387, #8850, #36557, #41734, #53182, #2579, #20651, #24737, #47642, #59443, #31387, #3321, #54293, #70912, #3686, #42837, #15114, #64262, #14749, #13650, #55383, #32846, #16930, #22480, #26951, #49119, #44677, #67208, #73098, #50211, #27673, #44310, #4777, #10675, #27311, #49844, #72369, #67565, #5504, #15473, #5138, #43573, #72736, #43940, #60911, #33205, #66094, #21384, #49477, #38017, #26579, #66464, #21749, #60174, #9583, #32484, #15841, #66840, #38387, #16210, #38763, #32115, #61282, #71647, #61636, #10314, #54649, #55744, #22122, #21020, #55018, #60540, #16569, #9946, #39121, #11038, #72009, #33563, #56112, #28042, #50571, #4422, #45030, #4053, #17650, #35020, #17297, #46113, #62732, #6950, #69381, #24293, #56469, #6593, #40210, #12124, #52376, #34651, #50930, #45388, #39858, #63459, #1058, #18014, #46841, #18377, #62370, #5860, #11768, #39484, #23568, #68650, #62007, #11409, #34284, #692, #57179, #23201, #40571, #29123, #33927, #63091, #28392, #40945, #45754, #327, #51656, #12492, #22836, #56816, #67924, #57548, #6223, #68290, #52019, #28751, #29482, #1420, #51291, #23926, #46476, #69014, #12846, #35379, #57902, #7311, #29841, #1782, #59353, #48661, #3600, #35742, #58992, #19465, #70088, #31670, #13937, #30206, #24653, #69730, #42751, #53468, #70462, #26122, #70823, #19099, #58261, #64175, #18736, #2859, #8036, #36839, #31298, #41654, #42023, #2493, #41300, #9133, #64544, #48297, #65272, #30571, #7667, #53097, #8398, #59725, #13563, #36474, #19837, #25017, #52737, #36108, #58629, #54203, #63810, #47559, #30927, #47933, #47199, #14659, #42389, #37202, #25389, #13202, #2142, #64911, #14301, #8764, #53839, #3234, #25761, #20197, #60091, #55659, #5055, #11952, #61199, #38678, #55300, #66379, #21665, #15755, #60823, #38294, #6412, #17482, #26490, #16125, #54565, #10594, #54931, #71925, #44222, #3968, #32391, #37933, #49032, #37567, #4338, #21300, #60453, #57006, #33122, #27592, #40042, #15391, #20559, #34477, #10229, #26863, #43854, #66755, #65642, #9500, #32763, #49394, #4694, #27224, #72655, #71561, #43117, #49761, #20936, #72287, #71186, #50124, #22036, #32029, #43487, #44595, #67126, #62556, #28944, #15030, #66011, #9861, #62912, #1601, #58083, #47023, #13025, #69200, #68835, #69558, #30393, #45939, #24835, #12306, #51482, #46661, #13755, #58446, #30018, #35206, #17832, #34841, #35564, #40393, #23747, #7491, #18192, #24112, #46295, #29663, #41125, #18919, #64365, #41479, #57368, #63999, #52562, #69913, #1968, #40762, #6776, #8222, #13379, #23390, #29308, #883, #52200, #18560, #24476, #19282, #2320, #51839, #63277, #68470, #1242, #12669, #35922, #57728, #7857, #63636, #52922, #47383, #7134, #41834, #36298, #58811, #14117, #15214, #42936, #59544, #65832, #14853, #64731, #36656, #19651, #2681, #37020, #31855, #3425, #54753, #47743, #20754, #21123, #9322, #25197, #3047, #25577, #59176, #8585, #8955, #4155, #26311, #48849, #60640, #66199, #70640, #42207, #37754, #60272, #43676, #43312, #71379, #37392, #25945, #54390, #48485, #20385, #71009, #38119, #49220, #31115, #9686, #53653, #32219, #14486, #31489, #3787, #48117, #65096, #20015, #42568, #70280, #54030, #65461, #30750, #53282, #59916, #26687, #71754, #15577, #67312, #27779, #39953, #44778, #72106, #11504, #66944, #10053, #10778, #16670, #21490, #4878, #44043, #39228, #66566, #44417, #22580, #49945, #50671, #55849, #72469, #16312, #15946, #27414, #50318, #61382, #5607, #61019, #61740, #33311, #75, #32586, #68024, #27052, #72841, #5238, #22223, #22933 ) ),
 .UNSPECIFIED., .F., .F., .F. ) 
 B_SPLINE_SURFACE_WITH_KNOTS ( ( 2, 2 ),
 ( 3, 2, 2, 2, 2, 2, 2, 2, 2, 2, 2, 2, 2, 2, 2, 2, 2, 2, 2, 2, 2, 2, 2, 2, 2, 2, 2, 2, 2, 2, 2, 2, 2, 2, 2, 2, 2, 2, 2, 2, 2, 2, 2, 2, 2, 2, 2, 2, 2, 2, 2, 2, 2, 2, 2, 2, 2, 2, 2, 2, 2, 2, 2, 2, 2, 2, 2, 2, 2, 2, 2, 2, 2, 2, 2, 2, 2, 2, 2, 2, 2, 2, 2, 2, 2, 2, 2, 2, 2, 2, 2, 2, 2, 2, 2, 2, 2, 2, 2, 2, 2, 2, 2, 2, 2, 2, 2, 2, 2, 2, 2, 2, 2, 2, 2, 2, 2, 2, 2, 2, 2, 2, 2, 2, 2, 2, 2, 2, 2, 2, 2, 2, 2, 2, 2, 2, 2, 2, 2, 2, 2, 2, 2, 2, 2, 2, 2, 2, 2, 2, 2, 2, 2, 2, 2, 2, 2, 2, 2, 2, 2, 2, 2, 2, 2, 2, 2, 2, 2, 2, 2, 2, 2, 2, 2, 2, 2, 2, 2, 2, 2, 2, 2, 2, 2, 2, 2, 2, 2, 2, 2, 2, 2, 2, 2, 2, 2, 2, 2, 2, 2, 2, 2, 2, 2, 2, 2, 2, 2, 2, 2, 2, 2, 2, 2, 2, 2, 2, 2, 2, 2, 2, 2, 2, 2, 2, 2, 2, 2, 2, 2, 2, 2, 2, 2, 2, 2, 2, 2, 2, 2, 2, 2, 2, 2, 2, 2, 2, 2, 2, 2, 2, 2, 2, 2, 2, 2, 2, 2, 2, 2, 2, 2, 2, 2, 2, 2, 2, 2, 2, 2, 2, 2, 2, 2, 2, 2, 2, 2, 2, 2, 2, 2, 2, 2, 2, 2, 2, 2, 2, 2, 2, 2, 2, 2, 2, 2, 2, 2, 2, 2, 2, 2, 2, 2, 2, 2, 2, 2, 2, 2, 2, 2, 2, 2, 2, 2, 2, 2, 2, 2, 2, 2, 2, 2, 2, 2, 2, 2, 2, 2, 2, 2, 2, 2, 2, 2, 2, 2, 2, 2, 2, 2, 2, 2, 2, 2, 2, 2, 2, 2, 2, 2, 2, 2, 2, 2, 2, 2, 2, 3 ),
 ( 0.000000000000000000, 1.000000000000000000 ),
 ( 0.000000000000000000, 0.002777777777777777884, 0.005555555555555555768, 0.008333333333333333218, 0.01111111111111111154, 0.01388888888888888812, 0.01666666666666666644, 0.01944444444444444475, 0.02222222222222222307, 0.02500000000000000139, 0.02777777777777777624, 0.03055555555555555455, 0.03333333333333333287, 0.03611111111111110772, 0.03888888888888888951, 0.04166666666666666435, 0.04444444444444444614, 0.04722222222222222099, 0.05000000000000000278, 0.05277777777777777762, 0.05555555555555555247, 0.05833333333333333426, 0.06111111111111110911, 0.06388888888888888395, 0.06666666666666666574, 0.06944444444444444753, 0.07222222222222221544, 0.07499999999999999722, 0.07777777777777777901, 0.08055555555555556080, 0.08333333333333332871, 0.08611111111111111049, 0.08888888888888889228, 0.09166666666666666019, 0.09444444444444444198, 0.09722222222222222376, 0.1000000000000000056, 0.1027777777777777735, 0.1055555555555555552, 0.1083333333333333370, 0.1111111111111111049, 0.1138888888888888867, 0.1166666666666666685, 0.1194444444444444503, 0.1222222222222222182, 0.1250000000000000000, 0.1277777777777777679, 0.1305555555555555636, 0.1333333333333333315, 0.1361111111111110994, 0.1388888888888888951, 0.1416666666666666630, 0.1444444444444444309, 0.1472222222222222265, 0.1499999999999999944, 0.1527777777777777901, 0.1555555555555555580, 0.1583333333333333259, 0.1611111111111111216, 0.1638888888888888895, 0.1666666666666666574, 0.1694444444444444531, 0.1722222222222222210, 0.1749999999999999889, 0.1777777777777777846, 0.1805555555555555525, 0.1833333333333333204, 0.1861111111111111160, 0.1888888888888888840, 0.1916666666666666796, 0.1944444444444444475, 0.1972222222222222154, 0.2000000000000000111, 0.2027777777777777790, 0.2055555555555555469, 0.2083333333333333426, 0.2111111111111111105, 0.2138888888888888784, 0.2166666666666666741, 0.2194444444444444420, 0.2222222222222222099, 0.2250000000000000056, 0.2277777777777777735, 0.2305555555555555691, 0.2333333333333333370, 0.2361111111111111049, 0.2388888888888889006, 0.2416666666666666685, 0.2444444444444444364, 0.2472222222222222321, 0.2500000000000000000, 0.2527777777777777679, 0.2555555555555555358, 0.2583333333333333592, 0.2611111111111111271, 0.2638888888888888951, 0.2666666666666666630, 0.2694444444444444309, 0.2722222222222221988, 0.2750000000000000222, 0.2777777777777777901, 0.2805555555555555580, 0.2833333333333333259, 0.2861111111111110938, 0.2888888888888888618, 0.2916666666666666852, 0.2944444444444444531, 0.2972222222222222210, 0.2999999999999999889, 0.3027777777777777568, 0.3055555555555555802, 0.3083333333333333481, 0.3111111111111111160, 0.3138888888888888840, 0.3166666666666666519, 0.3194444444444444198, 0.3222222222222222432, 0.3250000000000000111, 0.3277777777777777790, 0.3305555555555555469, 0.3333333333333333148, 0.3361111111111111382, 0.3388888888888889062, 0.3416666666666666741, 0.3444444444444444420, 0.3472222222222222099, 0.3499999999999999778, 0.3527777777777778012, 0.3555555555555555691, 0.3583333333333333370, 0.3611111111111111049, 0.3638888888888888729, 0.3666666666666666408, 0.3694444444444444642, 0.3722222222222222321, 0.3750000000000000000, 0.3777777777777777679, 0.3805555555555555358, 0.3833333333333333592, 0.3861111111111111271, 0.3888888888888888951, 0.3916666666666666630, 0.3944444444444444309, 0.3972222222222221988, 0.4000000000000000222, 0.4027777777777777901, 0.4055555555555555580, 0.4083333333333333259, 0.4111111111111110938, 0.4138888888888888618, 0.4166666666666666852, 0.4194444444444444531, 0.4222222222222222210, 0.4249999999999999889, 0.4277777777777777568, 0.4305555555555555802, 0.4333333333333333481, 0.4361111111111111160, 0.4388888888888888840, 0.4416666666666666519, 0.4444444444444444198, 0.4472222222222222432, 0.4500000000000000111, 0.4527777777777777790, 0.4555555555555555469, 0.4583333333333333148, 0.4611111111111111382, 0.4638888888888889062, 0.4666666666666666741, 0.4694444444444444420, 0.4722222222222222099, 0.4749999999999999778, 0.4777777777777778012, 0.4805555555555555691, 0.4833333333333333370, 0.4861111111111111049, 0.4888888888888888729, 0.4916666666666666408, 0.4944444444444444642, 0.4972222222222222321, 0.5000000000000000000, 0.5027777777777777679, 0.5055555555555555358, 0.5083333333333333037, 0.5111111111111110716, 0.5138888888888888395, 0.5166666666666667185, 0.5194444444444444864, 0.5222222222222222543, 0.5250000000000000222, 0.5277777777777777901, 0.5305555555555555580, 0.5333333333333333259, 0.5361111111111110938, 0.5388888888888888618, 0.5416666666666666297, 0.5444444444444443976, 0.5472222222222222765, 0.5500000000000000444, 0.5527777777777778123, 0.5555555555555555802, 0.5583333333333333481, 0.5611111111111111160, 0.5638888888888888840, 0.5666666666666666519, 0.5694444444444444198, 0.5722222222222221877, 0.5749999999999999556, 0.5777777777777777235, 0.5805555555555556024, 0.5833333333333333703, 0.5861111111111111382, 0.5888888888888889062, 0.5916666666666666741, 0.5944444444444444420, 0.5972222222222222099, 0.5999999999999999778, 0.6027777777777777457, 0.6055555555555555136, 0.6083333333333332815, 0.6111111111111111605, 0.6138888888888889284, 0.6166666666666666963, 0.6194444444444444642, 0.6222222222222222321, 0.6250000000000000000, 0.6277777777777777679, 0.6305555555555555358, 0.6333333333333333037, 0.6361111111111110716, 0.6388888888888888395, 0.6416666666666667185, 0.6444444444444444864, 0.6472222222222222543, 0.6500000000000000222, 0.6527777777777777901, 0.6555555555555555580, 0.6583333333333333259, 0.6611111111111110938, 0.6638888888888888618, 0.6666666666666666297, 0.6694444444444443976, 0.6722222222222222765, 0.6750000000000000444, 0.6777777777777778123, 0.6805555555555555802, 0.6833333333333333481, 0.6861111111111111160, 0.6888888888888888840, 0.6916666666666666519, 0.6944444444444444198, 0.6972222222222221877, 0.6999999999999999556, 0.7027777777777777235, 0.7055555555555556024, 0.7083333333333333703, 0.7111111111111111382, 0.7138888888888889062, 0.7166666666666666741, 0.7194444444444444420, 0.7222222222222222099, 0.7249999999999999778, 0.7277777777777777457, 0.7305555555555555136, 0.7333333333333332815, 0.7361111111111111605, 0.7388888888888889284, 0.7416666666666666963, 0.7444444444444444642, 0.7472222222222222321, 0.7500000000000000000, 0.7527777777777777679, 0.7555555555555555358, 0.7583333333333333037, 0.7611111111111110716, 0.7638888888888888395, 0.7666666666666667185, 0.7694444444444444864, 0.7722222222222222543, 0.7750000000000000222, 0.7777777777777777901, 0.7805555555555555580, 0.7833333333333333259, 0.7861111111111110938, 0.7888888888888888618, 0.7916666666666666297, 0.7944444444444443976, 0.7972222222222222765, 0.8000000000000000444, 0.8027777777777778123, 0.8055555555555555802, 0.8083333333333333481, 0.8111111111111111160, 0.8138888888888888840, 0.8166666666666666519, 0.8194444444444444198, 0.8222222222222221877, 0.8249999999999999556, 0.8277777777777777235, 0.8305555555555556024, 0.8333333333333333703, 0.8361111111111111382, 0.8388888888888889062, 0.8416666666666666741, 0.8444444444444444420, 0.8472222222222222099, 0.8499999999999999778, 0.8527777777777777457, 0.8555555555555555136, 0.8583333333333332815, 0.8611111111111111605, 0.8638888888888889284, 0.8666666666666666963, 0.8694444444444444642, 0.8722222222222222321, 0.8750000000000000000, 0.8777777777777777679, 0.8805555555555555358, 0.8833333333333333037, 0.8861111111111110716, 0.8888888888888888395, 0.8916666666666667185, 0.8944444444444444864, 0.8972222222222222543, 0.9000000000000000222, 0.9027777777777777901, 0.9055555555555555580, 0.9083333333333333259, 0.9111111111111110938, 0.9138888888888888618, 0.9166666666666666297, 0.9194444444444443976, 0.9222222222222222765, 0.9250000000000000444, 0.9277777777777778123, 0.9305555555555555802, 0.9333333333333333481, 0.9361111111111111160, 0.9388888888888888840, 0.9416666666666666519, 0.9444444444444444198, 0.9472222222222221877, 0.9499999999999999556, 0.9527777777777777235, 0.9555555555555556024, 0.9583333333333333703, 0.9611111111111111382, 0.9638888888888889062, 0.9666666666666666741, 0.9694444444444444420, 0.9722222222222222099, 0.9749999999999999778, 0.9777777777777777457, 0.9805555555555555136, 0.9833333333333332815, 0.9861111111111111605, 0.9888888888888889284, 0.9916666666666666963, 0.9944444444444444642, 0.9972222222222222321, 1.000000000000000000 ),
 .UNSPECIFIED. ) 
 GEOMETRIC_REPRESENTATION_ITEM ( )  RATIONAL_B_SPLINE_SURFACE ( (
 ( 1.000000000000000000, 0.8660254037844387076, 1.000000000000000000, 0.8660254037844387076, 1.000000000000000000, 0.8660254037844387076, 1.000000000000000000, 0.8660254037844387076, 1.000000000000000000, 0.8660254037844387076, 1.000000000000000000, 0.8660254037844387076, 1.000000000000000000, 0.8660254037844387076, 1.000000000000000000, 0.8660254037844387076, 1.000000000000000000, 0.8660254037844387076, 1.000000000000000000, 0.8660254037844387076, 1.000000000000000000, 0.8660254037844387076, 1.000000000000000000, 0.8660254037844387076, 1.000000000000000000, 0.8660254037844387076, 1.000000000000000000, 0.8660254037844387076, 1.000000000000000000, 0.8660254037844387076, 1.000000000000000000, 0.8660254037844387076, 1.000000000000000000, 0.8660254037844387076, 1.000000000000000000, 0.8660254037844387076, 1.000000000000000000, 0.8660254037844387076, 1.000000000000000000, 0.8660254037844387076, 1.000000000000000000, 0.8660254037844387076, 1.000000000000000000, 0.8660254037844387076, 1.000000000000000000, 0.8660254037844387076, 1.000000000000000000, 0.8660254037844387076, 1.000000000000000000, 0.8660254037844387076, 1.000000000000000000, 0.8660254037844387076, 1.000000000000000000, 0.8660254037844387076, 1.000000000000000000, 0.8660254037844387076, 1.000000000000000000, 0.8660254037844387076, 1.000000000000000000, 0.8660254037844387076, 1.000000000000000000, 0.8660254037844387076, 1.000000000000000000, 0.8660254037844387076, 1.000000000000000000, 0.8660254037844387076, 1.000000000000000000, 0.8660254037844387076, 1.000000000000000000, 0.8660254037844387076, 1.000000000000000000, 0.8660254037844387076, 1.000000000000000000, 0.8660254037844387076, 1.000000000000000000, 0.8660254037844387076, 1.000000000000000000, 0.8660254037844387076, 1.000000000000000000, 0.8660254037844387076, 1.000000000000000000, 0.8660254037844387076, 1.000000000000000000, 0.8660254037844387076, 1.000000000000000000, 0.8660254037844387076, 1.000000000000000000, 0.8660254037844387076, 1.000000000000000000, 0.8660254037844387076, 1.000000000000000000, 0.8660254037844387076, 1.000000000000000000, 0.8660254037844387076, 1.000000000000000000, 0.8660254037844387076, 1.000000000000000000, 0.8660254037844387076, 1.000000000000000000, 0.8660254037844387076, 1.000000000000000000, 0.8660254037844387076, 1.000000000000000000, 0.8660254037844387076, 1.000000000000000000, 0.8660254037844387076, 1.000000000000000000, 0.8660254037844387076, 1.000000000000000000, 0.8660254037844387076, 1.000000000000000000, 0.8660254037844387076, 1.000000000000000000, 0.8660254037844387076, 1.000000000000000000, 0.8660254037844387076, 1.000000000000000000, 0.8660254037844387076, 1.000000000000000000, 0.8660254037844387076, 1.000000000000000000, 0.8660254037844387076, 1.000000000000000000, 0.8660254037844387076, 1.000000000000000000, 0.8660254037844387076, 1.000000000000000000, 0.8660254037844387076, 1.000000000000000000, 0.8660254037844387076, 1.000000000000000000, 0.8660254037844387076, 1.000000000000000000, 0.8660254037844387076, 1.000000000000000000, 0.8660254037844387076, 1.000000000000000000, 0.8660254037844387076, 1.000000000000000000, 0.8660254037844387076, 1.000000000000000000, 0.8660254037844387076, 1.000000000000000000, 0.8660254037844387076, 1.000000000000000000, 0.8660254037844387076, 1.000000000000000000, 0.8660254037844387076, 1.000000000000000000, 0.8660254037844387076, 1.000000000000000000, 0.8660254037844387076, 1.000000000000000000, 0.8660254037844387076, 1.000000000000000000, 0.8660254037844387076, 1.000000000000000000, 0.8660254037844387076, 1.000000000000000000, 0.8660254037844387076, 1.000000000000000000, 0.8660254037844387076, 1.000000000000000000, 0.8660254037844387076, 1.000000000000000000, 0.8660254037844387076, 1.000000000000000000, 0.8660254037844387076, 1.000000000000000000, 0.8660254037844387076, 1.000000000000000000, 0.8660254037844387076, 1.000000000000000000, 0.8660254037844387076, 1.000000000000000000, 0.8660254037844387076, 1.000000000000000000, 0.8660254037844387076, 1.000000000000000000, 0.8660254037844387076, 1.000000000000000000, 0.8660254037844387076, 1.000000000000000000, 0.8660254037844387076, 1.000000000000000000, 0.8660254037844387076, 1.000000000000000000, 0.8660254037844387076, 1.000000000000000000, 0.8660254037844387076, 1.000000000000000000, 0.8660254037844387076, 1.000000000000000000, 0.8660254037844387076, 1.000000000000000000, 0.8660254037844387076, 1.000000000000000000, 0.8660254037844387076, 1.000000000000000000, 0.8660254037844387076, 1.000000000000000000, 0.8660254037844387076, 1.000000000000000000, 0.8660254037844387076, 1.000000000000000000, 0.8660254037844387076, 1.000000000000000000, 0.8660254037844387076, 1.000000000000000000, 0.8660254037844387076, 1.000000000000000000, 0.8660254037844387076, 1.000000000000000000, 0.8660254037844387076, 1.000000000000000000, 0.8660254037844387076, 1.000000000000000000, 0.8660254037844387076, 1.000000000000000000, 0.8660254037844387076, 1.000000000000000000, 0.8660254037844387076, 1.000000000000000000, 0.8660254037844387076, 1.000000000000000000, 0.8660254037844387076, 1.000000000000000000, 0.8660254037844387076, 1.000000000000000000, 0.8660254037844387076, 1.000000000000000000, 0.8660254037844387076, 1.000000000000000000, 0.8660254037844387076, 1.000000000000000000, 0.8660254037844387076, 1.000000000000000000, 0.8660254037844387076, 1.000000000000000000, 0.8660254037844387076, 1.000000000000000000, 0.8660254037844387076, 1.000000000000000000, 0.8660254037844387076, 1.000000000000000000, 0.8660254037844387076, 1.000000000000000000, 0.8660254037844387076, 1.000000000000000000, 0.8660254037844387076, 1.000000000000000000, 0.8660254037844387076, 1.000000000000000000, 0.8660254037844387076, 1.000000000000000000, 0.8660254037844387076, 1.000000000000000000, 0.8660254037844387076, 1.000000000000000000, 0.8660254037844387076, 1.000000000000000000, 0.8660254037844387076, 1.000000000000000000, 0.8660254037844387076, 1.000000000000000000, 0.8660254037844387076, 1.000000000000000000, 0.8660254037844387076, 1.000000000000000000, 0.8660254037844387076, 1.000000000000000000, 0.8660254037844387076, 1.000000000000000000, 0.8660254037844387076, 1.000000000000000000, 0.8660254037844387076, 1.000000000000000000, 0.8660254037844387076, 1.000000000000000000, 0.8660254037844387076, 1.000000000000000000, 0.8660254037844387076, 1.000000000000000000, 0.8660254037844387076, 1.000000000000000000, 0.8660254037844387076, 1.000000000000000000, 0.8660254037844387076, 1.000000000000000000, 0.8660254037844387076, 1.000000000000000000, 0.8660254037844387076, 1.000000000000000000, 0.8660254037844387076, 1.000000000000000000, 0.8660254037844387076, 1.000000000000000000, 0.8660254037844387076, 1.000000000000000000, 0.8660254037844387076, 1.000000000000000000, 0.8660254037844387076, 1.000000000000000000, 0.8660254037844387076, 1.000000000000000000, 0.8660254037844387076, 1.000000000000000000, 0.8660254037844387076, 1.000000000000000000, 0.8660254037844387076, 1.000000000000000000, 0.8660254037844387076, 1.000000000000000000, 0.8660254037844387076, 1.000000000000000000, 0.8660254037844387076, 1.000000000000000000, 0.8660254037844387076, 1.000000000000000000, 0.8660254037844387076, 1.000000000000000000, 0.8660254037844387076, 1.000000000000000000, 0.8660254037844387076, 1.000000000000000000, 0.8660254037844387076, 1.000000000000000000, 0.8660254037844387076, 1.000000000000000000, 0.8660254037844387076, 1.000000000000000000, 0.8660254037844387076, 1.000000000000000000, 0.8660254037844387076, 1.000000000000000000, 0.8660254037844387076, 1.000000000000000000, 0.8660254037844387076, 1.000000000000000000, 0.8660254037844387076, 1.000000000000000000, 0.8660254037844387076, 1.000000000000000000, 0.8660254037844387076, 1.000000000000000000, 0.8660254037844387076, 1.000000000000000000, 0.8660254037844387076, 1.000000000000000000, 0.8660254037844387076, 1.000000000000000000, 0.8660254037844387076, 1.000000000000000000, 0.8660254037844387076, 1.000000000000000000, 0.8660254037844387076, 1.000000000000000000, 0.8660254037844387076, 1.000000000000000000, 0.8660254037844387076, 1.000000000000000000, 0.8660254037844387076, 1.000000000000000000, 0.8660254037844387076, 1.000000000000000000, 0.8660254037844387076, 1.000000000000000000, 0.8660254037844387076, 1.000000000000000000, 0.8660254037844387076, 1.000000000000000000, 0.8660254037844387076, 1.000000000000000000, 0.8660254037844387076, 1.000000000000000000, 0.8660254037844387076, 1.000000000000000000, 0.8660254037844387076, 1.000000000000000000, 0.8660254037844387076, 1.000000000000000000, 0.8660254037844387076, 1.000000000000000000, 0.8660254037844387076, 1.000000000000000000, 0.8660254037844387076, 1.000000000000000000, 0.8660254037844387076, 1.000000000000000000, 0.8660254037844387076, 1.000000000000000000, 0.8660254037844387076, 1.000000000000000000, 0.8660254037844387076, 1.000000000000000000, 0.8660254037844387076, 1.000000000000000000, 0.8660254037844387076, 1.000000000000000000, 0.8660254037844387076, 1.000000000000000000, 0.8660254037844387076, 1.000000000000000000, 0.8660254037844387076, 1.000000000000000000, 0.8660254037844387076, 1.000000000000000000, 0.8660254037844387076, 1.000000000000000000, 0.8660254037844387076, 1.000000000000000000, 0.8660254037844387076, 1.000000000000000000, 0.8660254037844387076, 1.000000000000000000, 0.8660254037844387076, 1.000000000000000000, 0.8660254037844387076, 1.000000000000000000, 0.8660254037844387076, 1.000000000000000000, 0.8660254037844387076, 1.000000000000000000, 0.8660254037844387076, 1.000000000000000000, 0.8660254037844387076, 1.000000000000000000, 0.8660254037844387076, 1.000000000000000000, 0.8660254037844387076, 1.000000000000000000, 0.8660254037844387076, 1.000000000000000000, 0.8660254037844387076, 1.000000000000000000, 0.8660254037844387076, 1.000000000000000000, 0.8660254037844387076, 1.000000000000000000, 0.8660254037844387076, 1.000000000000000000, 0.8660254037844387076, 1.000000000000000000, 0.8660254037844387076, 1.000000000000000000, 0.8660254037844387076, 1.000000000000000000, 0.8660254037844387076, 1.000000000000000000, 0.8660254037844387076, 1.000000000000000000, 0.8660254037844387076, 1.000000000000000000, 0.8660254037844387076, 1.000000000000000000, 0.8660254037844387076, 1.000000000000000000, 0.8660254037844387076, 1.000000000000000000, 0.8660254037844387076, 1.000000000000000000, 0.8660254037844387076, 1.000000000000000000, 0.8660254037844387076, 1.000000000000000000, 0.8660254037844387076, 1.000000000000000000, 0.8660254037844387076, 1.000000000000000000, 0.8660254037844387076, 1.000000000000000000, 0.8660254037844387076, 1.000000000000000000, 0.8660254037844387076, 1.000000000000000000, 0.8660254037844387076, 1.000000000000000000, 0.8660254037844387076, 1.000000000000000000, 0.8660254037844387076, 1.000000000000000000, 0.8660254037844387076, 1.000000000000000000, 0.8660254037844387076, 1.000000000000000000, 0.8660254037844387076, 1.000000000000000000, 0.8660254037844387076, 1.000000000000000000, 0.8660254037844387076, 1.000000000000000000, 0.8660254037844387076, 1.000000000000000000, 0.8660254037844387076, 1.000000000000000000, 0.8660254037844387076, 1.000000000000000000, 0.8660254037844387076, 1.000000000000000000, 0.8660254037844387076, 1.000000000000000000, 0.8660254037844387076, 1.000000000000000000, 0.8660254037844387076, 1.000000000000000000, 0.8660254037844387076, 1.000000000000000000, 0.8660254037844387076, 1.000000000000000000, 0.8660254037844387076, 1.000000000000000000, 0.8660254037844387076, 1.000000000000000000, 0.8660254037844387076, 1.000000000000000000, 0.8660254037844387076, 1.000000000000000000, 0.8660254037844387076, 1.000000000000000000, 0.8660254037844387076, 1.000000000000000000, 0.8660254037844387076, 1.000000000000000000, 0.8660254037844387076, 1.000000000000000000, 0.8660254037844387076, 1.000000000000000000, 0.8660254037844387076, 1.000000000000000000, 0.8660254037844387076, 1.000000000000000000, 0.8660254037844387076, 1.000000000000000000, 0.8660254037844387076, 1.000000000000000000, 0.8660254037844387076, 1.000000000000000000, 0.8660254037844387076, 1.000000000000000000, 0.8660254037844387076, 1.000000000000000000, 0.8660254037844387076, 1.000000000000000000, 0.8660254037844387076, 1.000000000000000000, 0.8660254037844387076, 1.000000000000000000, 0.8660254037844387076, 1.000000000000000000, 0.8660254037844387076, 1.000000000000000000, 0.8660254037844387076, 1.000000000000000000, 0.8660254037844387076, 1.000000000000000000, 0.8660254037844387076, 1.000000000000000000, 0.8660254037844387076, 1.000000000000000000, 0.8660254037844387076, 1.000000000000000000, 0.8660254037844387076, 1.000000000000000000, 0.8660254037844387076, 1.000000000000000000, 0.8660254037844387076, 1.000000000000000000, 0.8660254037844387076, 1.000000000000000000, 0.8660254037844387076, 1.000000000000000000, 0.8660254037844387076, 1.000000000000000000, 0.8660254037844387076, 1.000000000000000000, 0.8660254037844387076, 1.000000000000000000, 0.8660254037844387076, 1.000000000000000000, 0.8660254037844387076, 1.000000000000000000, 0.8660254037844387076, 1.000000000000000000, 0.8660254037844387076, 1.000000000000000000, 0.8660254037844387076, 1.000000000000000000, 0.8660254037844387076, 1.000000000000000000, 0.8660254037844387076, 1.000000000000000000, 0.8660254037844387076, 1.000000000000000000, 0.8660254037844387076, 1.000000000000000000, 0.8660254037844387076, 1.000000000000000000, 0.8660254037844387076, 1.000000000000000000, 0.8660254037844387076, 1.000000000000000000, 0.8660254037844387076, 1.000000000000000000, 0.8660254037844387076, 1.000000000000000000, 0.8660254037844387076, 1.000000000000000000, 0.8660254037844387076, 1.000000000000000000, 0.8660254037844387076, 1.000000000000000000, 0.8660254037844387076, 1.000000000000000000, 0.8660254037844387076, 1.000000000000000000, 0.8660254037844387076, 1.000000000000000000, 0.8660254037844387076, 1.000000000000000000, 0.8660254037844387076, 1.000000000000000000, 0.8660254037844387076, 1.000000000000000000, 0.8660254037844387076, 1.000000000000000000, 0.8660254037844387076, 1.000000000000000000, 0.8660254037844387076, 1.000000000000000000, 0.8660254037844387076, 1.000000000000000000, 0.8660254037844387076, 1.000000000000000000, 0.8660254037844387076, 1.000000000000000000, 0.8660254037844387076, 1.000000000000000000, 0.8660254037844387076, 1.000000000000000000, 0.8660254037844387076, 1.000000000000000000, 0.8660254037844387076, 1.000000000000000000, 0.8660254037844387076, 1.000000000000000000, 0.8660254037844387076, 1.000000000000000000, 0.8660254037844387076, 1.000000000000000000, 0.8660254037844387076, 1.000000000000000000, 0.8660254037844387076, 1.000000000000000000, 0.8660254037844387076, 1.000000000000000000, 0.8660254037844387076, 1.000000000000000000, 0.8660254037844387076, 1.000000000000000000, 0.8660254037844387076, 1.000000000000000000, 0.8660254037844387076, 1.000000000000000000, 0.8660254037844387076, 1.000000000000000000, 0.8660254037844387076, 1.000000000000000000, 0.8660254037844387076, 1.000000000000000000, 0.8660254037844387076, 1.000000000000000000, 0.8660254037844387076, 1.000000000000000000, 0.8660254037844387076, 1.000000000000000000, 0.8660254037844387076, 1.000000000000000000, 0.8660254037844387076, 1.000000000000000000, 0.8660254037844387076, 1.000000000000000000, 0.8660254037844387076, 1.000000000000000000, 0.8660254037844387076, 1.000000000000000000, 0.8660254037844387076, 1.000000000000000000, 0.8660254037844387076, 1.000000000000000000, 0.8660254037844387076, 1.000000000000000000, 0.8660254037844387076, 1.000000000000000000, 0.8660254037844387076, 1.000000000000000000, 0.8660254037844387076, 1.000000000000000000, 0.8660254037844387076, 1.000000000000000000, 0.8660254037844387076, 1.000000000000000000, 0.8660254037844387076, 1.000000000000000000, 0.8660254037844387076, 1.000000000000000000, 0.8660254037844387076, 1.000000000000000000, 0.8660254037844387076, 1.000000000000000000, 0.8660254037844387076, 1.000000000000000000, 0.8660254037844387076, 1.000000000000000000, 0.8660254037844387076, 1.000000000000000000, 0.8660254037844387076, 1.000000000000000000, 0.8660254037844387076, 1.000000000000000000, 0.8660254037844387076, 1.000000000000000000),
 ( 1.000000000000000000, 0.8660254037844387076, 1.000000000000000000, 0.8660254037844387076, 1.000000000000000000, 0.8660254037844387076, 1.000000000000000000, 0.8660254037844387076, 1.000000000000000000, 0.8660254037844387076, 1.000000000000000000, 0.8660254037844387076, 1.000000000000000000, 0.8660254037844387076, 1.000000000000000000, 0.8660254037844387076, 1.000000000000000000, 0.8660254037844387076, 1.000000000000000000, 0.8660254037844387076, 1.000000000000000000, 0.8660254037844387076, 1.000000000000000000, 0.8660254037844387076, 1.000000000000000000, 0.8660254037844387076, 1.000000000000000000, 0.8660254037844387076, 1.000000000000000000, 0.8660254037844387076, 1.000000000000000000, 0.8660254037844387076, 1.000000000000000000, 0.8660254037844387076, 1.000000000000000000, 0.8660254037844387076, 1.000000000000000000, 0.8660254037844387076, 1.000000000000000000, 0.8660254037844387076, 1.000000000000000000, 0.8660254037844387076, 1.000000000000000000, 0.8660254037844387076, 1.000000000000000000, 0.8660254037844387076, 1.000000000000000000, 0.8660254037844387076, 1.000000000000000000, 0.8660254037844387076, 1.000000000000000000, 0.8660254037844387076, 1.000000000000000000, 0.8660254037844387076, 1.000000000000000000, 0.8660254037844387076, 1.000000000000000000, 0.8660254037844387076, 1.000000000000000000, 0.8660254037844387076, 1.000000000000000000, 0.8660254037844387076, 1.000000000000000000, 0.8660254037844387076, 1.000000000000000000, 0.8660254037844387076, 1.000000000000000000, 0.8660254037844387076, 1.000000000000000000, 0.8660254037844387076, 1.000000000000000000, 0.8660254037844387076, 1.000000000000000000, 0.8660254037844387076, 1.000000000000000000, 0.8660254037844387076, 1.000000000000000000, 0.8660254037844387076, 1.000000000000000000, 0.8660254037844387076, 1.000000000000000000, 0.8660254037844387076, 1.000000000000000000, 0.8660254037844387076, 1.000000000000000000, 0.8660254037844387076, 1.000000000000000000, 0.8660254037844387076, 1.000000000000000000, 0.8660254037844387076, 1.000000000000000000, 0.8660254037844387076, 1.000000000000000000, 0.8660254037844387076, 1.000000000000000000, 0.8660254037844387076, 1.000000000000000000, 0.8660254037844387076, 1.000000000000000000, 0.8660254037844387076, 1.000000000000000000, 0.8660254037844387076, 1.000000000000000000, 0.8660254037844387076, 1.000000000000000000, 0.8660254037844387076, 1.000000000000000000, 0.8660254037844387076, 1.000000000000000000, 0.8660254037844387076, 1.000000000000000000, 0.8660254037844387076, 1.000000000000000000, 0.8660254037844387076, 1.000000000000000000, 0.8660254037844387076, 1.000000000000000000, 0.8660254037844387076, 1.000000000000000000, 0.8660254037844387076, 1.000000000000000000, 0.8660254037844387076, 1.000000000000000000, 0.8660254037844387076, 1.000000000000000000, 0.8660254037844387076, 1.000000000000000000, 0.8660254037844387076, 1.000000000000000000, 0.8660254037844387076, 1.000000000000000000, 0.8660254037844387076, 1.000000000000000000, 0.8660254037844387076, 1.000000000000000000, 0.8660254037844387076, 1.000000000000000000, 0.8660254037844387076, 1.000000000000000000, 0.8660254037844387076, 1.000000000000000000, 0.8660254037844387076, 1.000000000000000000, 0.8660254037844387076, 1.000000000000000000, 0.8660254037844387076, 1.000000000000000000, 0.8660254037844387076, 1.000000000000000000, 0.8660254037844387076, 1.000000000000000000, 0.8660254037844387076, 1.000000000000000000, 0.8660254037844387076, 1.000000000000000000, 0.8660254037844387076, 1.000000000000000000, 0.8660254037844387076, 1.000000000000000000, 0.8660254037844387076, 1.000000000000000000, 0.8660254037844387076, 1.000000000000000000, 0.8660254037844387076, 1.000000000000000000, 0.8660254037844387076, 1.000000000000000000, 0.8660254037844387076, 1.000000000000000000, 0.8660254037844387076, 1.000000000000000000, 0.8660254037844387076, 1.000000000000000000, 0.8660254037844387076, 1.000000000000000000, 0.8660254037844387076, 1.000000000000000000, 0.8660254037844387076, 1.000000000000000000, 0.8660254037844387076, 1.000000000000000000, 0.8660254037844387076, 1.000000000000000000, 0.8660254037844387076, 1.000000000000000000, 0.8660254037844387076, 1.000000000000000000, 0.8660254037844387076, 1.000000000000000000, 0.8660254037844387076, 1.000000000000000000, 0.8660254037844387076, 1.000000000000000000, 0.8660254037844387076, 1.000000000000000000, 0.8660254037844387076, 1.000000000000000000, 0.8660254037844387076, 1.000000000000000000, 0.8660254037844387076, 1.000000000000000000, 0.8660254037844387076, 1.000000000000000000, 0.8660254037844387076, 1.000000000000000000, 0.8660254037844387076, 1.000000000000000000, 0.8660254037844387076, 1.000000000000000000, 0.8660254037844387076, 1.000000000000000000, 0.8660254037844387076, 1.000000000000000000, 0.8660254037844387076, 1.000000000000000000, 0.8660254037844387076, 1.000000000000000000, 0.8660254037844387076, 1.000000000000000000, 0.8660254037844387076, 1.000000000000000000, 0.8660254037844387076, 1.000000000000000000, 0.8660254037844387076, 1.000000000000000000, 0.8660254037844387076, 1.000000000000000000, 0.8660254037844387076, 1.000000000000000000, 0.8660254037844387076, 1.000000000000000000, 0.8660254037844387076, 1.000000000000000000, 0.8660254037844387076, 1.000000000000000000, 0.8660254037844387076, 1.000000000000000000, 0.8660254037844387076, 1.000000000000000000, 0.8660254037844387076, 1.000000000000000000, 0.8660254037844387076, 1.000000000000000000, 0.8660254037844387076, 1.000000000000000000, 0.8660254037844387076, 1.000000000000000000, 0.8660254037844387076, 1.000000000000000000, 0.8660254037844387076, 1.000000000000000000, 0.8660254037844387076, 1.000000000000000000, 0.8660254037844387076, 1.000000000000000000, 0.8660254037844387076, 1.000000000000000000, 0.8660254037844387076, 1.000000000000000000, 0.8660254037844387076, 1.000000000000000000, 0.8660254037844387076, 1.000000000000000000, 0.8660254037844387076, 1.000000000000000000, 0.8660254037844387076, 1.000000000000000000, 0.8660254037844387076, 1.000000000000000000, 0.8660254037844387076, 1.000000000000000000, 0.8660254037844387076, 1.000000000000000000, 0.8660254037844387076, 1.000000000000000000, 0.8660254037844387076, 1.000000000000000000, 0.8660254037844387076, 1.000000000000000000, 0.8660254037844387076, 1.000000000000000000, 0.8660254037844387076, 1.000000000000000000, 0.8660254037844387076, 1.000000000000000000, 0.8660254037844387076, 1.000000000000000000, 0.8660254037844387076, 1.000000000000000000, 0.8660254037844387076, 1.000000000000000000, 0.8660254037844387076, 1.000000000000000000, 0.8660254037844387076, 1.000000000000000000, 0.8660254037844387076, 1.000000000000000000, 0.8660254037844387076, 1.000000000000000000, 0.8660254037844387076, 1.000000000000000000, 0.8660254037844387076, 1.000000000000000000, 0.8660254037844387076, 1.000000000000000000, 0.8660254037844387076, 1.000000000000000000, 0.8660254037844387076, 1.000000000000000000, 0.8660254037844387076, 1.000000000000000000, 0.8660254037844387076, 1.000000000000000000, 0.8660254037844387076, 1.000000000000000000, 0.8660254037844387076, 1.000000000000000000, 0.8660254037844387076, 1.000000000000000000, 0.8660254037844387076, 1.000000000000000000, 0.8660254037844387076, 1.000000000000000000, 0.8660254037844387076, 1.000000000000000000, 0.8660254037844387076, 1.000000000000000000, 0.8660254037844387076, 1.000000000000000000, 0.8660254037844387076, 1.000000000000000000, 0.8660254037844387076, 1.000000000000000000, 0.8660254037844387076, 1.000000000000000000, 0.8660254037844387076, 1.000000000000000000, 0.8660254037844387076, 1.000000000000000000, 0.8660254037844387076, 1.000000000000000000, 0.8660254037844387076, 1.000000000000000000, 0.8660254037844387076, 1.000000000000000000, 0.8660254037844387076, 1.000000000000000000, 0.8660254037844387076, 1.000000000000000000, 0.8660254037844387076, 1.000000000000000000, 0.8660254037844387076, 1.000000000000000000, 0.8660254037844387076, 1.000000000000000000, 0.8660254037844387076, 1.000000000000000000, 0.8660254037844387076, 1.000000000000000000, 0.8660254037844387076, 1.000000000000000000, 0.8660254037844387076, 1.000000000000000000, 0.8660254037844387076, 1.000000000000000000, 0.8660254037844387076, 1.000000000000000000, 0.8660254037844387076, 1.000000000000000000, 0.8660254037844387076, 1.000000000000000000, 0.8660254037844387076, 1.000000000000000000, 0.8660254037844387076, 1.000000000000000000, 0.8660254037844387076, 1.000000000000000000, 0.8660254037844387076, 1.000000000000000000, 0.8660254037844387076, 1.000000000000000000, 0.8660254037844387076, 1.000000000000000000, 0.8660254037844387076, 1.000000000000000000, 0.8660254037844387076, 1.000000000000000000, 0.8660254037844387076, 1.000000000000000000, 0.8660254037844387076, 1.000000000000000000, 0.8660254037844387076, 1.000000000000000000, 0.8660254037844387076, 1.000000000000000000, 0.8660254037844387076, 1.000000000000000000, 0.8660254037844387076, 1.000000000000000000, 0.8660254037844387076, 1.000000000000000000, 0.8660254037844387076, 1.000000000000000000, 0.8660254037844387076, 1.000000000000000000, 0.8660254037844387076, 1.000000000000000000, 0.8660254037844387076, 1.000000000000000000, 0.8660254037844387076, 1.000000000000000000, 0.8660254037844387076, 1.000000000000000000, 0.8660254037844387076, 1.000000000000000000, 0.8660254037844387076, 1.000000000000000000, 0.8660254037844387076, 1.000000000000000000, 0.8660254037844387076, 1.000000000000000000, 0.8660254037844387076, 1.000000000000000000, 0.8660254037844387076, 1.000000000000000000, 0.8660254037844387076, 1.000000000000000000, 0.8660254037844387076, 1.000000000000000000, 0.8660254037844387076, 1.000000000000000000, 0.8660254037844387076, 1.000000000000000000, 0.8660254037844387076, 1.000000000000000000, 0.8660254037844387076, 1.000000000000000000, 0.8660254037844387076, 1.000000000000000000, 0.8660254037844387076, 1.000000000000000000, 0.8660254037844387076, 1.000000000000000000, 0.8660254037844387076, 1.000000000000000000, 0.8660254037844387076, 1.000000000000000000, 0.8660254037844387076, 1.000000000000000000, 0.8660254037844387076, 1.000000000000000000, 0.8660254037844387076, 1.000000000000000000, 0.8660254037844387076, 1.000000000000000000, 0.8660254037844387076, 1.000000000000000000, 0.8660254037844387076, 1.000000000000000000, 0.8660254037844387076, 1.000000000000000000, 0.8660254037844387076, 1.000000000000000000, 0.8660254037844387076, 1.000000000000000000, 0.8660254037844387076, 1.000000000000000000, 0.8660254037844387076, 1.000000000000000000, 0.8660254037844387076, 1.000000000000000000, 0.8660254037844387076, 1.000000000000000000, 0.8660254037844387076, 1.000000000000000000, 0.8660254037844387076, 1.000000000000000000, 0.8660254037844387076, 1.000000000000000000, 0.8660254037844387076, 1.000000000000000000, 0.8660254037844387076, 1.000000000000000000, 0.8660254037844387076, 1.000000000000000000, 0.8660254037844387076, 1.000000000000000000, 0.8660254037844387076, 1.000000000000000000, 0.8660254037844387076, 1.000000000000000000, 0.8660254037844387076, 1.000000000000000000, 0.8660254037844387076, 1.000000000000000000, 0.8660254037844387076, 1.000000000000000000, 0.8660254037844387076, 1.000000000000000000, 0.8660254037844387076, 1.000000000000000000, 0.8660254037844387076, 1.000000000000000000, 0.8660254037844387076, 1.000000000000000000, 0.8660254037844387076, 1.000000000000000000, 0.8660254037844387076, 1.000000000000000000, 0.8660254037844387076, 1.000000000000000000, 0.8660254037844387076, 1.000000000000000000, 0.8660254037844387076, 1.000000000000000000, 0.8660254037844387076, 1.000000000000000000, 0.8660254037844387076, 1.000000000000000000, 0.8660254037844387076, 1.000000000000000000, 0.8660254037844387076, 1.000000000000000000, 0.8660254037844387076, 1.000000000000000000, 0.8660254037844387076, 1.000000000000000000, 0.8660254037844387076, 1.000000000000000000, 0.8660254037844387076, 1.000000000000000000, 0.8660254037844387076, 1.000000000000000000, 0.8660254037844387076, 1.000000000000000000, 0.8660254037844387076, 1.000000000000000000, 0.8660254037844387076, 1.000000000000000000, 0.8660254037844387076, 1.000000000000000000, 0.8660254037844387076, 1.000000000000000000, 0.8660254037844387076, 1.000000000000000000, 0.8660254037844387076, 1.000000000000000000, 0.8660254037844387076, 1.000000000000000000, 0.8660254037844387076, 1.000000000000000000, 0.8660254037844387076, 1.000000000000000000, 0.8660254037844387076, 1.000000000000000000, 0.8660254037844387076, 1.000000000000000000, 0.8660254037844387076, 1.000000000000000000, 0.8660254037844387076, 1.000000000000000000, 0.8660254037844387076, 1.000000000000000000, 0.8660254037844387076, 1.000000000000000000, 0.8660254037844387076, 1.000000000000000000, 0.8660254037844387076, 1.000000000000000000, 0.8660254037844387076, 1.000000000000000000, 0.8660254037844387076, 1.000000000000000000, 0.8660254037844387076, 1.000000000000000000, 0.8660254037844387076, 1.000000000000000000, 0.8660254037844387076, 1.000000000000000000, 0.8660254037844387076, 1.000000000000000000, 0.8660254037844387076, 1.000000000000000000, 0.8660254037844387076, 1.000000000000000000, 0.8660254037844387076, 1.000000000000000000, 0.8660254037844387076, 1.000000000000000000, 0.8660254037844387076, 1.000000000000000000, 0.8660254037844387076, 1.000000000000000000, 0.8660254037844387076, 1.000000000000000000, 0.8660254037844387076, 1.000000000000000000, 0.8660254037844387076, 1.000000000000000000, 0.8660254037844387076, 1.000000000000000000, 0.8660254037844387076, 1.000000000000000000, 0.8660254037844387076, 1.000000000000000000, 0.8660254037844387076, 1.000000000000000000, 0.8660254037844387076, 1.000000000000000000, 0.8660254037844387076, 1.000000000000000000, 0.8660254037844387076, 1.000000000000000000, 0.8660254037844387076, 1.000000000000000000, 0.8660254037844387076, 1.000000000000000000, 0.8660254037844387076, 1.000000000000000000, 0.8660254037844387076, 1.000000000000000000, 0.8660254037844387076, 1.000000000000000000, 0.8660254037844387076, 1.000000000000000000, 0.8660254037844387076, 1.000000000000000000, 0.8660254037844387076, 1.000000000000000000, 0.8660254037844387076, 1.000000000000000000, 0.8660254037844387076, 1.000000000000000000, 0.8660254037844387076, 1.000000000000000000, 0.8660254037844387076, 1.000000000000000000, 0.8660254037844387076, 1.000000000000000000, 0.8660254037844387076, 1.000000000000000000, 0.8660254037844387076, 1.000000000000000000, 0.8660254037844387076, 1.000000000000000000, 0.8660254037844387076, 1.000000000000000000, 0.8660254037844387076, 1.000000000000000000, 0.8660254037844387076, 1.000000000000000000, 0.8660254037844387076, 1.000000000000000000, 0.8660254037844387076, 1.000000000000000000, 0.8660254037844387076, 1.000000000000000000, 0.8660254037844387076, 1.000000000000000000, 0.8660254037844387076, 1.000000000000000000, 0.8660254037844387076, 1.000000000000000000, 0.8660254037844387076, 1.000000000000000000, 0.8660254037844387076, 1.000000000000000000, 0.8660254037844387076, 1.000000000000000000, 0.8660254037844387076, 1.000000000000000000, 0.8660254037844387076, 1.000000000000000000, 0.8660254037844387076, 1.000000000000000000, 0.8660254037844387076, 1.000000000000000000, 0.8660254037844387076, 1.000000000000000000, 0.8660254037844387076, 1.000000000000000000, 0.8660254037844387076, 1.000000000000000000, 0.8660254037844387076, 1.000000000000000000, 0.8660254037844387076, 1.000000000000000000, 0.8660254037844387076, 1.000000000000000000, 0.8660254037844387076, 1.000000000000000000, 0.8660254037844387076, 1.000000000000000000, 0.8660254037844387076, 1.000000000000000000, 0.8660254037844387076, 1.000000000000000000, 0.8660254037844387076, 1.000000000000000000, 0.8660254037844387076, 1.000000000000000000, 0.8660254037844387076, 1.000000000000000000, 0.8660254037844387076, 1.000000000000000000, 0.8660254037844387076, 1.000000000000000000, 0.8660254037844387076, 1.000000000000000000, 0.8660254037844387076, 1.000000000000000000, 0.8660254037844387076, 1.000000000000000000, 0.8660254037844387076, 1.000000000000000000, 0.8660254037844387076, 1.000000000000000000, 0.8660254037844387076, 1.000000000000000000, 0.8660254037844387076, 1.000000000000000000) ) ) 
 REPRESENTATION_ITEM ( '' )  SURFACE ( )  );
#71778 = CARTESIAN_POINT ( 'NONE',  ( 21.60937500061451644, 4.541064518000418104, -2.621784821874998173 ) ) ;
#71779 = CARTESIAN_POINT ( 'NONE',  ( 13.84687500061451715, 4.119189519843966529, -2.378215178124998275 ) ) ;
#71780 = CARTESIAN_POINT ( 'NONE',  ( 7.078125000614516438, 6.421520780324663323E-16, -5.243569643749999010 ) ) ;
#71781 = CARTESIAN_POINT ( 'NONE',  ( 14.22187500061451537, -6.054752690667223547, -1.112240025338166033E-15 ) ) ;
#71782 = EDGE_LOOP ( 'NONE', ( #31569, #42923, #39072, #40354 ) ) ;
#71783 = CARTESIAN_POINT ( 'NONE',  ( 22.88437500061451857, 6.421520780324663323E-16, -5.243569643749999010 ) ) ;
#71784 = CARTESIAN_POINT ( 'NONE',  ( 3.780892357739494170, 3.275126314170736741, -28.66976688362063186 ) ) ;
#71785 = CARTESIAN_POINT ( 'NONE',  ( 8.699999999999999289, 4.330127018922192761, -2.499999999999997780 ) ) ;
#71786 = CARTESIAN_POINT ( 'NONE',  ( 6.262500000000000178, -5.773502691896255534, -1.060575238724906372E-15 ) ) ;
#71787 = CARTESIAN_POINT ( 'NONE',  ( 16.65000000122903501, -2.886751345948129988, 4.999999999999997335 ) ) ;
#71788 = LINE ( 'NONE', #53690, #67907 ) ;
#71789 = CARTESIAN_POINT ( 'NONE',  ( 8.559375000614515727, 2.746126346562643317, 4.756430356249998326 ) ) ;
#71790 = ORIENTED_EDGE ( 'NONE', *, *, #18349, .F. ) ;
#71791 = CARTESIAN_POINT ( 'NONE',  ( 14.13750000000000107, 5.773502691896255534, 3.535250795749688894E-16 ) ) ;
#71792 = CARTESIAN_POINT ( 'NONE',  ( 15.93750000000000000, 5.773502691896255534, 3.535250795749688894E-16 ) ) ;
#71793 = CARTESIAN_POINT ( 'NONE',  ( 11.09062500061451573, -3.027376345333610441, -5.243569643749999898 ) ) ;
#71794 = ORIENTED_EDGE ( 'NONE', *, *, #51099, .F. ) ;
#71795 = CARTESIAN_POINT ( 'NONE',  ( -3.999999999999999112, 16.92500000122903359, -32.30940107675850470 ) ) ;
#71796 = CARTESIAN_POINT ( 'NONE',  ( -2.121784821874999949, 16.18437500061451573, -33.67503911421598417 ) ) ;
#71797 = CARTESIAN_POINT ( 'NONE',  ( 29.21250000122903145, 0.000000000000000000, 4.999999999999998224 ) ) ;
#71798 = CARTESIAN_POINT ( 'NONE',  ( 3.756430356249998770, 13.95312499938548534, 32.16877607737301759 ) ) ;
#71799 = CARTESIAN_POINT ( 'NONE',  ( 9.299999999999998934, 0.000000000000000000, 4.999999999999998224 ) ) ;
#71800 = CARTESIAN_POINT ( 'NONE',  ( 3.937500001229034208, 4.330127018922191873, 2.499999999999999556 ) ) ;
#71801 = VERTEX_POINT ( 'NONE', #53999 ) ;
#71802 = CARTESIAN_POINT ( 'NONE',  ( 23.46562500061451573, 3.027376345333611329, 5.243569643749999010 ) ) ;
#71803 = CARTESIAN_POINT ( 'NONE',  ( 10.20000000000000107, 0.000000000000000000, 4.999999999999998224 ) ) ;
#71804 = CARTESIAN_POINT ( 'NONE',  ( 3.756430356250000102, 19.39062499938548356, 30.00000000000000000 ) ) ;
#71805 = CARTESIAN_POINT ( 'NONE',  ( 20.40937500061451715, 0.000000000000000000, 5.243569643749999010 ) ) ;
#71806 = CARTESIAN_POINT ( 'NONE',  ( 19.86562500061451786, 3.027376345333611329, 5.243569643749999010 ) ) ;
#71807 = CARTESIAN_POINT ( 'NONE',  ( -2.121784821874996840, 14.02812500061459389, -26.32496088578401583 ) ) ;
#71808 = CARTESIAN_POINT ( 'NONE',  ( 24.26250000122903216, 0.000000000000000000, 4.999999999999998224 ) ) ;
#71809 = CARTESIAN_POINT ( 'NONE',  ( 4.978125000614518569, 4.541064518000418104, 2.621784821874999949 ) ) ;
#71810 = CARTESIAN_POINT ( 'NONE',  ( 24.15937500061451715, -4.119189519843965641, -2.378215178125001383 ) ) ;
#71811 = CARTESIAN_POINT ( 'NONE',  ( 20.80312500061451431, 0.000000000000000000, 5.243569643749999010 ) ) ;
#71812 = CARTESIAN_POINT ( 'NONE',  ( 7.471875000614519813, -5.492252693125287522, -1.008910452111647106E-15 ) ) ;
#71813 = CARTESIAN_POINT ( 'NONE',  ( -1.878215178125001827, 17.89062499938548356, 33.25316411605952283 ) ) ;
#71814 = CARTESIAN_POINT ( 'NONE',  ( 15.68437500061451573, 6.421520780324663323E-16, -5.243569643749999010 ) ) ;
#71815 = CARTESIAN_POINT ( 'NONE',  ( 13.80937500061451750, -4.541064518000417216, -2.621784821875001281 ) ) ;
#71816 = CARTESIAN_POINT ( 'NONE',  ( 23.18437500061451573, -4.541064518000419881, 2.621784821874995952 ) ) ;
#71817 = CARTESIAN_POINT ( 'NONE',  ( 4.243569643749999898, 12.84687500061451715, 32.45002607614398471 ) ) ;
#71818 = CARTESIAN_POINT ( 'NONE',  ( 5.090625000614516615, -3.027376345333614438, 5.243569643749998122 ) ) ;
#71819 = CARTESIAN_POINT ( 'NONE',  ( 27.62812500061451360, -4.541064518000419881, 2.621784821874995952 ) ) ;
#71820 = CARTESIAN_POINT ( 'NONE',  ( 26.80312500061451431, -4.541064518000417216, -2.621784821875001281 ) ) ;
#71821 = CARTESIAN_POINT ( 'NONE',  ( -1.394453263437886604E-15, 19.32500000122903216, -26.00000000000000000 ) ) ;
#71822 = CARTESIAN_POINT ( 'NONE',  ( 1.999999999999998668, 18.05000000000000071, 26.53589838486224650 ) ) ;
#71823 = CARTESIAN_POINT ( 'NONE',  ( 6.084375000614518747, -4.541064518000419881, 2.621784821874995952 ) ) ;
#71824 =( NAMED_UNIT ( * ) SI_UNIT ( $, .STERADIAN. ) SOLID_ANGLE_UNIT ( ) );
#71825 = CARTESIAN_POINT ( 'NONE',  ( 14.85000000122903252, -2.886751345948129988, 4.999999999999997335 ) ) ;
#71826 = CARTESIAN_POINT ( 'NONE',  ( 10.08750000122903323, 6.123233995736764310E-16, -4.999999999999998224 ) ) ;
#71827 = CARTESIAN_POINT ( 'NONE',  ( 28.38750000122903216, -4.330127018922194537, 2.499999999999995559 ) ) ;
#71828 = CARTESIAN_POINT ( 'NONE',  ( 2.828200636599751609E-16, 16.60624999877096641, 25.38119784648299415 ) ) ;
#71829 = CARTESIAN_POINT ( 'NONE',  ( 17.90625000122903288, 0.000000000000000000, 4.999999999999998224 ) ) ;
#71830 = CARTESIAN_POINT ( 'NONE',  ( 15.49687500061451750, -3.027376345333614438, 5.243569643749998122 ) ) ;
#71831 = CYLINDRICAL_SURFACE ( 'NONE', #63215, 4.000000000000000000 ) ;
#71832 = ORIENTED_EDGE ( 'NONE', *, *, #49066, .F. ) ;
#71833 = EDGE_CURVE ( 'NONE', #4995, #61022, #40602, .T. ) ;
#71834 = CARTESIAN_POINT ( 'NONE',  ( 18.70312500061451644, -4.541064518000417216, -2.621784821875001281 ) ) ;
#71835 = CARTESIAN_POINT ( 'NONE',  ( 8.428125000614517859, 6.421520780324663323E-16, -5.243569643749999010 ) ) ;
#71836 = CARTESIAN_POINT ( 'NONE',  ( 23.18437500061451573, -4.541064518000419881, 2.621784821874995952 ) ) ;
#71837 = CARTESIAN_POINT ( 'NONE',  ( 5.540625000614515905, -3.027376345333614438, 5.243569643749998122 ) ) ;
#71838 = CARTESIAN_POINT ( 'NONE',  ( 20.88749999999999929, 5.773502691896255534, 3.535250795749688401E-16 ) ) ;
#71839 = CARTESIAN_POINT ( 'NONE',  ( 7.012500001229035718, 4.330127018922192761, -2.499999999999997780 ) ) ;
#71840 = CARTESIAN_POINT ( 'NONE',  ( 23.54062500061451146, -3.027376345333614438, 5.243569643749998122 ) ) ;
#71841 = CARTESIAN_POINT ( 'NONE',  ( 3.999999999999999112, 17.63750000122903572, -30.00000000000000000 ) ) ;
#71842 = CARTESIAN_POINT ( 'NONE',  ( 9.637500001229033941, 6.123233995736764310E-16, -4.999999999999998224 ) ) ;
#71843 = CARTESIAN_POINT ( 'NONE',  ( 18.85312500061451502, 4.541064518000418104, -2.621784821874998173 ) ) ;
#71844 = CARTESIAN_POINT ( 'NONE',  ( 16.30312500061451786, 0.000000000000000000, 5.243569643749999010 ) ) ;
#71845 = CARTESIAN_POINT ( 'NONE',  ( 29.22187500061451715, 2.746126346562645981, -4.756430356249997438 ) ) ;
#71846 = CARTESIAN_POINT ( 'NONE',  ( 15.45000000000000107, 4.330127018922192761, -2.499999999999997780 ) ) ;
#71847 = CARTESIAN_POINT ( 'NONE',  ( 12.18750000122903465, -4.330127018922194537, 2.499999999999995559 ) ) ;
#71848 = CARTESIAN_POINT ( 'NONE',  ( 7.678125000614516082, 4.541064518000418104, 2.621784821874999949 ) ) ;
#71849 = CARTESIAN_POINT ( 'NONE',  ( 12.21562500061451573, 3.027376345333611329, 5.243569643749999010 ) ) ;
#71850 = CARTESIAN_POINT ( 'NONE',  ( 21.26250000122903572, -4.330127018922190985, -2.500000000000001332 ) ) ;
#71851 = CARTESIAN_POINT ( 'NONE',  ( 19.05937500061451928, 0.000000000000000000, 5.243569643749999010 ) ) ;
#71852 = CARTESIAN_POINT ( 'NONE',  ( 7.368750001229031454, 2.886751345948018077, -5.000000000000190070 ) ) ;
#71853 = CARTESIAN_POINT ( 'NONE',  ( 5.625000001229036428, 2.886751345948129099, -4.999999999999998224 ) ) ;
#71854 = CARTESIAN_POINT ( 'NONE',  ( 4.021875000614516082, 3.027376345333613106, -5.243569643749998122 ) ) ;
#71855 = CARTESIAN_POINT ( 'NONE',  ( 24.15937500061451715, -4.541064518000417216, -2.621784821875001281 ) ) ;
#71856 = EDGE_CURVE ( 'NONE', #8994, #27542, #25496, .T. ) ;
#71857 = CARTESIAN_POINT ( 'NONE',  ( 1.626862140677534273E-15, 18.42500000122903359, 34.00000000000000000 ) ) ;
#71858 = CARTESIAN_POINT ( 'NONE',  ( 19.00312500061451715, 0.000000000000000000, 5.243569643749999010 ) ) ;
#71859 = CARTESIAN_POINT ( 'NONE',  ( 23.14687500061451786, -3.027376345333614438, 5.243569643749998122 ) ) ;
#71860 = CARTESIAN_POINT ( 'NONE',  ( -7.967954043666661671E-16, 19.39062499938548356, 34.33755215474603517 ) ) ;
#71861 = CARTESIAN_POINT ( 'NONE',  ( 0.000000000000000000, 27.50000000000000000, 30.00000000000000000 ) ) ;
#71862 = CARTESIAN_POINT ( 'NONE',  ( 28.32187500061451502, 3.027376345333613106, -5.243569643749998122 ) ) ;
#71863 = CARTESIAN_POINT ( 'NONE',  ( 20.18437500061451217, 5.492252693125287522, 3.363034840372157021E-16 ) ) ;
#71864 = CARTESIAN_POINT ( 'NONE',  ( 15.32812500061451644, 4.541064518000418104, 2.621784821874999949 ) ) ;
#71865 = CARTESIAN_POINT ( 'NONE',  ( 12.15937500061451892, 4.541064518000418104, -2.621784821874998173 ) ) ;
#71866 = VERTEX_POINT ( 'NONE', #50642 ) ;
#71867 = CARTESIAN_POINT ( 'NONE',  ( 10.66875000122903216, 2.886751345948126879, 4.999999999999998224 ) ) ;
#71868 = CARTESIAN_POINT ( 'NONE',  ( 21.77812500061451928, -4.541064518000419881, 2.621784821874995952 ) ) ;
#71869 = CARTESIAN_POINT ( 'NONE',  ( -3.999999999999999112, 19.83125000061451715, 30.00000000000000000 ) ) ;
#71870 = DIRECTION ( 'NONE',  ( 1.000000000000000000, 0.000000000000000000, 0.000000000000000000 ) ) ;
#71871 = CARTESIAN_POINT ( 'NONE',  ( 15.48749999999999893, 5.773502691896255534, 3.535250795749688894E-16 ) ) ;
#71872 = CARTESIAN_POINT ( 'NONE',  ( 23.13750000122903216, 6.123233995736764310E-16, -4.999999999999998224 ) ) ;
#71873 = CARTESIAN_POINT ( 'NONE',  ( 19.00312500061451715, 0.000000000000000000, 5.243569643749999010 ) ) ;
#71874 = ORIENTED_EDGE ( 'NONE', *, *, #11525, .F. ) ;
#71875 = CARTESIAN_POINT ( 'NONE',  ( 22.72499999999999787, 4.330127018922191873, 2.499999999999999556 ) ) ;
#71876 = CARTESIAN_POINT ( 'NONE',  ( 24.53437500061451715, -4.541064518000419881, 2.621784821874995952 ) ) ;
#71877 = ORIENTED_EDGE ( 'NONE', *, *, #62721, .T. ) ;
#71878 = CARTESIAN_POINT ( 'NONE',  ( 4.000000000000000000, 19.25000000000000000, 30.00000000000000000 ) ) ;
#71879 = CARTESIAN_POINT ( 'NONE',  ( 11.87812500061451537, -4.541064518000419881, 2.621784821874995952 ) ) ;
#71880 = DIRECTION ( 'NONE',  ( -1.000000000000000000, -0.000000000000000000, -0.000000000000000000 ) ) ;
#71881 = CARTESIAN_POINT ( 'NONE',  ( 13.50937500061451679, 2.746126346562643317, 4.756430356249998326 ) ) ;
#71882 = CARTESIAN_POINT ( 'NONE',  ( 17.36249999999999716, 2.886751345948126879, 4.999999999999999112 ) ) ;
#71883 = CARTESIAN_POINT ( 'NONE',  ( 23.55000000000000071, 4.330127018922192761, -2.499999999999997780 ) ) ;
#71884 = CARTESIAN_POINT ( 'NONE',  ( 9.001249775931846008E-16, 19.01562500061451644, 34.90005215228797653 ) ) ;
#71885 = CARTESIAN_POINT ( 'NONE',  ( 5.109375000614518214, 0.000000000000000000, 5.243569643749999010 ) ) ;
#71886 = CARTESIAN_POINT ( 'NONE',  ( 17.40937500061451715, -4.541064518000417216, -2.621784821875001281 ) ) ;
#71887 = CARTESIAN_POINT ( 'NONE',  ( 28.65937500061451715, -4.541064518000417216, -2.621784821875001281 ) ) ;
#71888 = ORIENTED_EDGE ( 'NONE', *, *, #9558, .T. ) ;
#71889 = CARTESIAN_POINT ( 'NONE',  ( 25.64062500061451644, 6.054752690667223547, 3.707466751127219781E-16 ) ) ;
#71890 = CARTESIAN_POINT ( 'NONE',  ( 27.45937500061451786, 4.541064518000418104, -2.621784821874998173 ) ) ;
#71891 = DIRECTION ( 'NONE',  ( -1.000000000000000000, -0.000000000000000000, -0.000000000000000000 ) ) ;
#71892 = CARTESIAN_POINT ( 'NONE',  ( 14.66249999999999964, 2.886751345948126879, 4.999999999999999112 ) ) ;
#71893 = CARTESIAN_POINT ( 'NONE',  ( 11.91562500061451857, -6.054752690667223547, -1.112240025338166033E-15 ) ) ;
#71894 = CARTESIAN_POINT ( 'NONE',  ( 30.00000000000000000, 0.000000000000000000, 0.000000000000000000 ) ) ;
#71895 = CARTESIAN_POINT ( 'NONE',  ( 1.071796769724490783, 19.41740381056767006, -34.00000000000000000 ) ) ;
#71896 = CARTESIAN_POINT ( 'NONE',  ( 29.05312500061451431, -4.541064518000417216, -2.621784821875001281 ) ) ;
#71897 = CARTESIAN_POINT ( 'NONE',  ( 16.23750000122903359, -4.330127018922194537, 2.499999999999995559 ) ) ;
#71898 = CARTESIAN_POINT ( 'NONE',  ( 15.22500000122903074, 2.886751345948193936, 4.999999999999883649 ) ) ;
#71899 = CARTESIAN_POINT ( 'NONE',  ( 14.48437500061451821, 4.119189519843966529, 2.378215178124999607 ) ) ;
#71900 = CARTESIAN_POINT ( 'NONE',  ( 4.828125000614518214, 6.421520780324663323E-16, -5.243569643749999010 ) ) ;
#71901 = CARTESIAN_POINT ( 'NONE',  ( 22.28437500061451715, -4.541064518000419881, 2.621784821874995952 ) ) ;
#71902 = CARTESIAN_POINT ( 'NONE',  ( 9.001249775931846008E-16, 17.72187500061451715, 34.90005215228797653 ) ) ;
#71903 = CARTESIAN_POINT ( 'NONE',  ( 22.32187500061451502, -6.054752690667223547, -1.112240025338166033E-15 ) ) ;
#71904 = CARTESIAN_POINT ( 'NONE',  ( 28.73437500061451644, 6.421520780324663323E-16, -5.243569643749999010 ) ) ;
#71905 = CARTESIAN_POINT ( 'NONE',  ( -2.121784821874999949, 19.78437500061451715, 26.32496088578401938 ) ) ;
#71906 = CARTESIAN_POINT ( 'NONE',  ( 11.54062500061451857, -3.027376345333610441, -5.243569643749999898 ) ) ;
#71907 = CARTESIAN_POINT ( 'NONE',  ( 2.000000000000001332, 17.11250000122903359, 33.46410161513774995 ) ) ;
#71908 = CARTESIAN_POINT ( 'NONE',  ( 8.146875000614516082, 6.054752690667223547, 3.707466751127219781E-16 ) ) ;
#71909 = CARTESIAN_POINT ( 'NONE',  ( 3.867736846495323011, 3.168783417359460231, -3.937610184585229156 ) ) ;
#71910 = CARTESIAN_POINT ( 'NONE',  ( 10.00312500061451715, 0.000000000000000000, 5.243569643749999010 ) ) ;
#71911 = CARTESIAN_POINT ( 'NONE',  ( 13.50937500061451679, 4.541064518000418104, -2.621784821874998173 ) ) ;
#71912 = CARTESIAN_POINT ( 'NONE',  ( 6.037500001229035185, 6.123233995736764310E-16, -4.999999999999998224 ) ) ;
#71913 = CARTESIAN_POINT ( 'NONE',  ( 22.42500000122903359, 2.886751345948126879, 4.999999999999999112 ) ) ;
#71914 = CARTESIAN_POINT ( 'NONE',  ( 9.159375000614515372, 0.000000000000000000, 5.243569643749999010 ) ) ;
#71915 = CARTESIAN_POINT ( 'NONE',  ( 10.34062500061451750, 6.054752690667223547, 3.707466751127219781E-16 ) ) ;
#71916 = CARTESIAN_POINT ( 'NONE',  ( 24.73125000122903216, -4.330127018922194537, 2.499999999999995559 ) ) ;
#71917 = CARTESIAN_POINT ( 'NONE',  ( 21.38437500061451502, -4.541064518000419881, 2.621784821874995952 ) ) ;
#71918 = CARTESIAN_POINT ( 'NONE',  ( 25.42500000122902648, 2.886751345948095793, -5.000000000000055067 ) ) ;
#71919 = CARTESIAN_POINT ( 'NONE',  ( -3.182292052831501739, 3.860956188314066395, 32.43599349108946939 ) ) ;
#71920 = LINE ( 'NONE', #2851, #57283 ) ;
#71921 = CARTESIAN_POINT ( 'NONE',  ( 4.243569643749999010, 11.12187500061451928, -32.45002607614398471 ) ) ;
#71922 = CARTESIAN_POINT ( 'NONE',  ( 15.93750000122903110, 6.123233995736764310E-16, -4.999999999999998224 ) ) ;
#71923 = CARTESIAN_POINT ( 'NONE',  ( 4.243569643749999010, 15.11562500061451608, -32.45002607614398471 ) ) ;
#71924 = CARTESIAN_POINT ( 'NONE',  ( 16.42500000122903359, 2.886751345948129099, -4.999999999999998224 ) ) ;
#71925 = CARTESIAN_POINT ( 'NONE',  ( 10.67812500061451608, 6.421520780324663323E-16, -5.243569643749999010 ) ) ;
#71926 = ORIENTED_EDGE ( 'NONE', *, *, #47179, .F. ) ;
#71927 = CARTESIAN_POINT ( 'NONE',  ( 13.61250000000000071, 2.886751345948129099, -4.999999999999998224 ) ) ;
#71928 = CARTESIAN_POINT ( 'NONE',  ( 23.83125000122903359, -4.330127018922194537, 2.499999999999995559 ) ) ;
#71929 = CARTESIAN_POINT ( 'NONE',  ( 22.60312500061451857, 0.000000000000000000, 5.243569643749999010 ) ) ;
#71930 = CARTESIAN_POINT ( 'NONE',  ( 10.88437500061451679, 4.541064518000418104, 2.621784821874999949 ) ) ;
#71931 = CARTESIAN_POINT ( 'NONE',  ( -1.626862140677534273E-15, 16.83124999877096428, 34.00000000000000000 ) ) ;
#71932 = CARTESIAN_POINT ( 'NONE',  ( 9.187500001229034652, 6.123233995736764310E-16, -4.999999999999998224 ) ) ;
#71933 = CARTESIAN_POINT ( 'NONE',  ( 18.71250000122903145, 4.330127018922192761, -2.499999999999997780 ) ) ;
#71934 = CARTESIAN_POINT ( 'NONE',  ( 14.76562500061451821, 3.027376345333613106, -5.243569643749998122 ) ) ;
#71935 = CARTESIAN_POINT ( 'NONE',  ( 18.25312500061451715, -4.541064518000417216, -2.621784821875001281 ) ) ;
#71936 = CARTESIAN_POINT ( 'NONE',  ( 25.76250000122903216, -4.330127018922190985, -2.500000000000001332 ) ) ;
#71937 = ADVANCED_FACE ( 'NONE', ( #45462 ), #4849, .F. ) ;
#71938 = CARTESIAN_POINT ( 'NONE',  ( 28.91250000122903074, -4.330127018922190985, -2.500000000000001332 ) ) ;
#71939 = CARTESIAN_POINT ( 'NONE',  ( 22.53750000000000142, -2.886751345948125991, -5.000000000000000000 ) ) ;
#71940 = CARTESIAN_POINT ( 'NONE',  ( 3.756430356250000102, 13.54062499938548392, 30.00000000000000000 ) ) ;
#71941 = CARTESIAN_POINT ( 'NONE',  ( 25.35937500061451644, 0.000000000000000000, 5.243569643749999010 ) ) ;
#71942 = CARTESIAN_POINT ( 'NONE',  ( 12.30000000122903181, -2.886751345948125991, -5.000000000000000000 ) ) ;
#71943 = CARTESIAN_POINT ( 'NONE',  ( 29.67187500061451644, 3.027376345333613106, -5.243569643749998122 ) ) ;
#71944 = EDGE_CURVE ( 'NONE', #2861, #37056, #22551, .T. ) ;
#71945 = FACE_OUTER_BOUND ( 'NONE', #58935, .T. ) ;
#71946 = CARTESIAN_POINT ( 'NONE',  ( 6.046875000614519102, -3.027376345333614438, 5.243569643749998122 ) ) ;
#71947 = CARTESIAN_POINT ( 'NONE',  ( 25.94062500061451715, -3.027376345333610441, -5.243569643749999898 ) ) ;
#71948 = CARTESIAN_POINT ( 'NONE',  ( 2.655984681222220721E-16, 12.86562499938548321, 25.66244784525396483 ) ) ;
#71949 = CARTESIAN_POINT ( 'NONE',  ( 16.27499999999999858, 6.123233995736764310E-16, -4.999999999999998224 ) ) ;
#71950 = CARTESIAN_POINT ( 'NONE',  ( 10.84687500061451892, 6.054752690667223547, 3.707466751127219781E-16 ) ) ;
#71951 = CARTESIAN_POINT ( 'NONE',  ( 4.317513935836856831, -2.521720328239906550, 4.456045716080967445 ) ) ;
#71952 = CARTESIAN_POINT ( 'NONE',  ( 28.90312500061451217, 0.000000000000000000, 5.243569643749999010 ) ) ;
#71953 = CARTESIAN_POINT ( 'NONE',  ( 8.296875000614516438, -3.027376345333614438, 5.243569643749998122 ) ) ;
#71954 = CARTESIAN_POINT ( 'NONE',  ( 29.22187500061451715, 3.027376345333613106, -5.243569643749998122 ) ) ;
#71955 = CARTESIAN_POINT ( 'NONE',  ( 2.121784821875001281, 11.40312500061459566, 33.67503911421598417 ) ) ;
#71956 = CARTESIAN_POINT ( 'NONE',  ( 23.06250000000000355, 2.886751345948129099, -4.999999999999998224 ) ) ;
#71957 = ORIENTED_EDGE ( 'NONE', *, *, #43507, .T. ) ;
#71959 = EDGE_CURVE ( 'NONE', #45966, #29431, #55456, .T. ) ;
#71958 = CARTESIAN_POINT ( 'NONE',  ( -2.000000000000000000, 17.67500000000000071, -33.46410161513775705 ) ) ;
#71960 =( BOUNDED_CURVE ( )  B_SPLINE_CURVE ( 2, ( #22164, #44716, #33608, #56152, #12164, #46154, #45796 ),
 .UNSPECIFIED., .F., .F. ) 
 B_SPLINE_CURVE_WITH_KNOTS ( ( 3, 2, 2, 3 ),
 ( 0.1300000000000000322, 0.1333333333333333592, 0.1366666666666666585, 0.1400000000000000133 ),
 .UNSPECIFIED. ) 
 CURVE ( )  GEOMETRIC_REPRESENTATION_ITEM ( )  RATIONAL_B_SPLINE_CURVE ( ( 0.9999999999999988898, 0.8660254037844398178, 1.000000000000000000, 0.8660254037844387076, 1.000000000000000000, 0.8660254037844387076, 1.000000000000000000 ) ) 
 REPRESENTATION_ITEM ( '' )  );
#71961 = CARTESIAN_POINT ( 'NONE',  ( 3.487500000000000711, -2.886751345948129988, 4.999999999999997335 ) ) ;
#71962 = ORIENTED_EDGE ( 'NONE', *, *, #37402, .T. ) ;
#71963 = CARTESIAN_POINT ( 'NONE',  ( 17.80312500061451786, -4.541064518000417216, -2.621784821875001281 ) ) ;
#71964 = CARTESIAN_POINT ( 'NONE',  ( 11.91562500061451857, -6.054752690667223547, -1.112240025338166033E-15 ) ) ;
#71965 = CARTESIAN_POINT ( 'NONE',  ( 21.90937500061451715, 2.746126346562645981, -4.756430356249997438 ) ) ;
#71966 = CARTESIAN_POINT ( 'NONE',  ( 6.909375000614518036, 0.000000000000000000, 5.243569643749999010 ) ) ;
#71967 = CARTESIAN_POINT ( 'NONE',  ( 19.35000000122903430, -2.886751345948129988, 4.999999999999997335 ) ) ;
#71968 = DIRECTION ( 'NONE',  ( -0.000000000000000000, -1.000000000000000000, -0.000000000000000000 ) ) ;
#71969 = CARTESIAN_POINT ( 'NONE',  ( 7.321875000614516793, 3.027376345333611329, 5.243569643749999010 ) ) ;
#71970 = CARTESIAN_POINT ( 'NONE',  ( 14.29687500061451821, -3.027376345333610441, -5.243569643749999898 ) ) ;
#71971 = CARTESIAN_POINT ( 'NONE',  ( 23.93437500061451573, 4.541064518000418104, 2.621784821874999949 ) ) ;
#71972 = VECTOR ( 'NONE', #3256, 1000.000000000000000 ) ;
#71973 = VERTEX_POINT ( 'NONE', #66534 ) ;
#71974 = CARTESIAN_POINT ( 'NONE',  ( 13.08750000000000036, -2.886751345948125991, -5.000000000000000000 ) ) ;
#71975 = CARTESIAN_POINT ( 'NONE',  ( 17.25937500061451502, 0.000000000000000000, 5.243569643749999010 ) ) ;
#71976 = CARTESIAN_POINT ( 'NONE',  ( 10.02187500061451964, 3.027376345333611329, 5.243569643749999010 ) ) ;
#71977 = CARTESIAN_POINT ( 'NONE',  ( 2.655984681222220721E-16, 14.55312499938548321, 25.66244784525396483 ) ) ;
#71978 = CARTESIAN_POINT ( 'NONE',  ( 21.89999999999999858, 0.000000000000000000, 4.999999999999998224 ) ) ;
#71979 = CARTESIAN_POINT ( 'NONE',  ( -8.484601909799255319E-16, 17.78750000000000142, 34.61880215351700940 ) ) ;
#71980 = CARTESIAN_POINT ( 'NONE',  ( -2.121784821874999949, 10.33437500061451786, -33.67503911421598417 ) ) ;
#71981 = CARTESIAN_POINT ( 'NONE',  ( 23.18437500061451573, -4.119189519843968306, 2.378215178124996054 ) ) ;
#71982 = CARTESIAN_POINT ( 'NONE',  ( 12.02812500061451573, 6.421520780324663323E-16, -5.243569643749999010 ) ) ;
#71983 = CARTESIAN_POINT ( 'NONE',  ( 28.13437500061451502, -4.541064518000419881, 2.621784821874995952 ) ) ;
#71984 = CARTESIAN_POINT ( 'NONE',  ( 13.25625000122903074, 4.330127018922192761, -2.499999999999997780 ) ) ;
#71985 = CARTESIAN_POINT ( 'NONE',  ( 27.87187500061451573, 3.027376345333613106, -5.243569643749998122 ) ) ;
#71986 = CARTESIAN_POINT ( 'NONE',  ( 13.16249999999999964, 2.886751345948129099, -4.999999999999998224 ) ) ;
#71987 = CARTESIAN_POINT ( 'NONE',  ( 3.999999999999999112, 16.73750000122903359, 30.00000000000000000 ) ) ;
#71988 = CARTESIAN_POINT ( 'NONE',  ( 11.21250000122903501, 0.000000000000000000, 4.999999999999998224 ) ) ;
#71989 = CARTESIAN_POINT ( 'NONE',  ( 21.83437500061451786, -4.541064518000419881, 2.621784821874995952 ) ) ;
#71990 = CARTESIAN_POINT ( 'NONE',  ( 16.32187500061451502, 3.027376345333611329, 5.243569643749999010 ) ) ;
#71991 = CARTESIAN_POINT ( 'NONE',  ( 4.017893810940423194, 2.976003446579597256, -4.317231760934856943 ) ) ;
#71992 = EDGE_LOOP ( 'NONE', ( #59581, #17603, #9712, #64718 ) ) ;
#71993 = CARTESIAN_POINT ( 'NONE',  ( 16.37812500061451715, -4.541064518000419881, 2.621784821874995952 ) ) ;
#71994 = CARTESIAN_POINT ( 'NONE',  ( 28.08750000122903145, 6.123233995736764310E-16, -4.999999999999998224 ) ) ;
#71995 = CARTESIAN_POINT ( 'NONE',  ( 14.55937500061451573, 0.000000000000000000, 5.243569643749999010 ) ) ;
#71996 = CARTESIAN_POINT ( 'NONE',  ( 27.13125000122903430, 6.123233995736764310E-16, -4.999999999999998224 ) ) ;
#71997 = CARTESIAN_POINT ( 'NONE',  ( 20.01562500061451644, -6.054752690667223547, -1.112240025338166033E-15 ) ) ;
#71998 = CARTESIAN_POINT ( 'NONE',  ( 28.35937500061451289, 4.541064518000418104, -2.621784821874998173 ) ) ;
#71999 = CARTESIAN_POINT ( 'NONE',  ( -4.243569643749999898, 13.50312500061451715, 30.00000000000000000 ) ) ;
#72000 = CARTESIAN_POINT ( 'NONE',  ( 18.12187500061451573, 3.027376345333611329, 5.243569643749999010 ) ) ;
#72001 = CARTESIAN_POINT ( 'NONE',  ( 13.65000000122903323, -2.886751345948125991, -5.000000000000000000 ) ) ;
#72002 = CARTESIAN_POINT ( 'NONE',  ( 10.28437500061451715, 5.824947211148865298E-16, -4.756430356249998326 ) ) ;
#72003 = CARTESIAN_POINT ( 'NONE',  ( 4.243569643749999898, 18.73437500061451644, -30.00000000000000000 ) ) ;
#72004 = CARTESIAN_POINT ( 'NONE',  ( 21.19687500061451502, 6.054752690667223547, 3.707466751127219781E-16 ) ) ;
#72005 = CARTESIAN_POINT ( 'NONE',  ( 22.72500000122903430, 2.886751345948129099, -4.999999999999998224 ) ) ;
#72006 = CARTESIAN_POINT ( 'NONE',  ( 17.03437500061451715, 6.421520780324663323E-16, -5.243569643749999010 ) ) ;
#72007 = CARTESIAN_POINT ( 'NONE',  ( 13.45312500061451466, 4.541064518000418104, -2.621784821874998173 ) ) ;
#72008 = CARTESIAN_POINT ( 'NONE',  ( 4.243569643749999898, 11.98437500061451821, 30.00000000000000000 ) ) ;
#72009 = CARTESIAN_POINT ( 'NONE',  ( 16.49062500061451786, -3.027376345333610441, -5.243569643749999898 ) ) ;
#72010 = VERTEX_POINT ( 'NONE', #21823 ) ;
#72011 = ORIENTED_EDGE ( 'NONE', *, *, #59196, .T. ) ;
#72012 = CARTESIAN_POINT ( 'NONE',  ( 24.00000000000000000, 4.330127018922192761, -2.499999999999997780 ) ) ;
#72013 = CARTESIAN_POINT ( 'NONE',  ( 4.243569643749999010, 18.32187500061451502, -32.45002607614398471 ) ) ;
#72014 = CARTESIAN_POINT ( 'NONE',  ( 24.25312500061451715, 4.541064518000418104, -2.621784821874998173 ) ) ;
#72015 = CARTESIAN_POINT ( 'NONE',  ( 5.578125000614518214, -4.541064518000419881, 2.621784821874995952 ) ) ;
#72016 = CARTESIAN_POINT ( 'NONE',  ( 18.11250000122903359, -4.330127018922190985, -2.500000000000001332 ) ) ;
#72017 = CARTESIAN_POINT ( 'NONE',  ( 22.67812500061451431, -4.541064518000419881, 2.621784821874995952 ) ) ;
#72018 = CARTESIAN_POINT ( 'NONE',  ( 23.66250000000000142, 2.886751345948126879, 4.999999999999999112 ) ) ;
#72019 = CARTESIAN_POINT ( 'NONE',  ( 25.64062500061451644, 6.054752690667223547, 3.707466751127219781E-16 ) ) ;
#72020 = CARTESIAN_POINT ( 'NONE',  ( 4.528125000614516615, 4.541064518000418104, 2.621784821874999949 ) ) ;
#72021 = ORIENTED_EDGE ( 'NONE', *, *, #28241, .T. ) ;
#72022 = CARTESIAN_POINT ( 'NONE',  ( 22.19062500061451715, -3.027376345333614438, 5.243569643749998122 ) ) ;
#72023 = CARTESIAN_POINT ( 'NONE',  ( -1.071796769724490561, 13.02634618820330381, 26.00000000000000000 ) ) ;
#72024 = CARTESIAN_POINT ( 'NONE',  ( 11.37187500061451750, 2.746126346562643317, 4.756430356249998326 ) ) ;
#72025 = CARTESIAN_POINT ( 'NONE',  ( 4.000000000000000000, 18.83749999999999858, 32.30940107675849760 ) ) ;
#72026 = CARTESIAN_POINT ( 'NONE',  ( 8.484601909799253346E-16, 13.92500000122903359, -25.38119784648299770 ) ) ;
#72027 = EDGE_CURVE ( 'NONE', #1784, #40656, #27022, .T. ) ;
#72028 = CARTESIAN_POINT ( 'NONE',  ( -2.000000000000000000, 10.13750000122903572, 26.53589838486224650 ) ) ;
#72029 = CARTESIAN_POINT ( 'NONE',  ( 10.72500000000000142, -4.330127018922194537, 2.499999999999995559 ) ) ;
#72030 = CARTESIAN_POINT ( 'NONE',  ( 12.23437500061451821, 4.541064518000418104, 2.621784821874999949 ) ) ;
#72031 = CARTESIAN_POINT ( 'NONE',  ( 7.050000001229036251, 5.773502691896255534, 3.535250795749688894E-16 ) ) ;
#72032 = CARTESIAN_POINT ( 'NONE',  ( 13.80937500061451750, -4.541064518000417216, -2.621784821875001281 ) ) ;
#72033 = CARTESIAN_POINT ( 'NONE',  ( 6.984375000614516438, -4.541064518000419881, 2.621784821874995952 ) ) ;
#72034 = FACE_OUTER_BOUND ( 'NONE', #24114, .T. ) ;
#72035 = CARTESIAN_POINT ( 'NONE',  ( -0.7368805616696195715, 9.859898480082234684, 25.82089837893477480 ) ) ;
#72036 = CARTESIAN_POINT ( 'NONE',  ( 13.58437500061451786, 4.541064518000418104, 2.621784821874999949 ) ) ;
#72037 = CARTESIAN_POINT ( 'NONE',  ( 3.684201729119676916, 3.380333950832448142, 4.008536514702806919 ) ) ;
#72038 = CARTESIAN_POINT ( 'NONE',  ( 21.96562500061451573, 3.027376345333613106, -5.243569643749998122 ) ) ;
#72039 = LINE ( 'NONE', #45058, #62810 ) ;
#72040 = CARTESIAN_POINT ( 'NONE',  ( 24.23437500061451644, 6.421520780324663323E-16, -5.243569643749999010 ) ) ;
#72041 = CARTESIAN_POINT ( 'NONE',  ( 29.58750000122903501, 4.330127018922191873, 2.499999999999999556 ) ) ;
#72042 = CARTESIAN_POINT ( 'NONE',  ( 19.80937500061451217, 2.746126346562643317, 4.756430356249998326 ) ) ;
#72043 = CARTESIAN_POINT ( 'NONE',  ( 24.25312500061451715, 4.541064518000418104, -2.621784821874998173 ) ) ;
#72044 = CARTESIAN_POINT ( 'NONE',  ( 18.77812500061451573, 6.421520780324663323E-16, -5.243569643749999010 ) ) ;
#72045 = CARTESIAN_POINT ( 'NONE',  ( 14.98125000122903216, 6.123233995736764310E-16, -4.999999999999998224 ) ) ;
#72046 = CARTESIAN_POINT ( 'NONE',  ( 14.07187500061451679, 3.027376345333611329, 5.243569643749999010 ) ) ;
#72047 = CARTESIAN_POINT ( 'NONE',  ( 30.00000000000000000, 0.000000000000000000, 4.999999999999998224 ) ) ;
#72048 = CARTESIAN_POINT ( 'NONE',  ( 28.23750000122903359, 4.330127018922191873, 2.499999999999999556 ) ) ;
#72049 = CARTESIAN_POINT ( 'NONE',  ( 4.021875000614516082, 3.027376345333613106, -5.243569643749998122 ) ) ;
#72050 = CARTESIAN_POINT ( 'NONE',  ( 13.39687500061451608, -3.027376345333610441, -5.243569643749999898 ) ) ;
#72051 = CARTESIAN_POINT ( 'NONE',  ( 21.89999999999999858, 0.000000000000000000, 4.999999999999998224 ) ) ;
#72052 = CARTESIAN_POINT ( 'NONE',  ( 4.537500001229034297, -4.330127018922194537, 2.499999999999995559 ) ) ;
#72053 = CARTESIAN_POINT ( 'NONE',  ( 25.13437500061451502, 6.421520780324663323E-16, -5.243569643749999010 ) ) ;
#72054 = CARTESIAN_POINT ( 'NONE',  ( 17.25937500061451502, 0.000000000000000000, 5.243569643749999010 ) ) ;
#72055 = CARTESIAN_POINT ( 'NONE',  ( -3.756430356249999214, 15.64062499938548179, 27.83122392262697531 ) ) ;
#72056 = CARTESIAN_POINT ( 'NONE',  ( 29.25000000000000000, -4.330127018922190985, -2.500000000000001332 ) ) ;
#72057 = CARTESIAN_POINT ( 'NONE',  ( 6.412500000000001421, 2.886751345948129099, -4.999999999999998224 ) ) ;
#72058 = CARTESIAN_POINT ( 'NONE',  ( 28.95937500061451431, 0.000000000000000000, 4.756430356249998326 ) ) ;
#72059 = CARTESIAN_POINT ( 'NONE',  ( 19.90312500061451573, 0.000000000000000000, 5.243569643749999010 ) ) ;
#72060 = CARTESIAN_POINT ( 'NONE',  ( 8.587500000000002132, -2.886751345948125991, -5.000000000000000000 ) ) ;
#72061 = CARTESIAN_POINT ( 'NONE',  ( 5.015625000614518214, 3.027376345333611329, 5.243569643749999010 ) ) ;
#72062 = CARTESIAN_POINT ( 'NONE',  ( 19.46249999999999858, 2.886751345948129099, -4.999999999999998224 ) ) ;
#72063 = CARTESIAN_POINT ( 'NONE',  ( 2.000000000000000444, 16.56874999877096499, 26.53589838486224650 ) ) ;
#72064 = CARTESIAN_POINT ( 'NONE',  ( 22.08750000122903501, -4.330127018922194537, 2.499999999999995559 ) ) ;
#72065 = CARTESIAN_POINT ( 'NONE',  ( 5.959992197959415705, 8.030459126529553515, 29.19994738672135526 ) ) ;
#72066 = CARTESIAN_POINT ( 'NONE',  ( 28.73437500061451644, 6.421520780324663323E-16, -5.243569643749999010 ) ) ;
#72067 = VERTEX_POINT ( 'NONE', #67282 ) ;
#72068 = CARTESIAN_POINT ( 'NONE',  ( 17.54062500061451502, 6.054752690667223547, 3.707466751127219781E-16 ) ) ;
#72069 = CARTESIAN_POINT ( 'NONE',  ( 24.62812500061451715, 6.421520780324663323E-16, -5.243569643749999010 ) ) ;
#72070 = CARTESIAN_POINT ( 'NONE',  ( 25.77187500061451075, 3.027376345333611329, 5.243569643749999010 ) ) ;
#72071 = CARTESIAN_POINT ( 'NONE',  ( 6.000000000000001776, 4.330127018922192761, -2.499999999999997780 ) ) ;
#72072 = CARTESIAN_POINT ( 'NONE',  ( 9.590625000614517504, -3.027376345333614438, 5.243569643749998122 ) ) ;
#72073 = CARTESIAN_POINT ( 'NONE',  ( 25.60312500061451502, 4.541064518000418104, -2.621784821874998173 ) ) ;
#72074 = CARTESIAN_POINT ( 'NONE',  ( 14.74687500061451573, -3.027376345333610441, -5.243569643749999898 ) ) ;
#72075 = CARTESIAN_POINT ( 'NONE',  ( 18.64687500061451786, -3.027376345333614438, 5.243569643749998122 ) ) ;
#72076 = CARTESIAN_POINT ( 'NONE',  ( 9.001249775931846008E-16, 19.46562500061451573, 34.90005215228797653 ) ) ;
#72077 = CARTESIAN_POINT ( 'NONE',  ( 24.97500000122903430, 2.886751345948129099, -4.999999999999998224 ) ) ;
#72078 = CARTESIAN_POINT ( 'NONE',  ( 16.65937500061452070, 4.119189519843966529, -2.378215178124998275 ) ) ;
#72079 = CARTESIAN_POINT ( 'NONE',  ( 11.35312500061451679, 0.000000000000000000, 5.243569643749999010 ) ) ;
#72080 = CARTESIAN_POINT ( 'NONE',  ( 8.146875000614516082, 6.054752690667223547, 3.707466751127219781E-16 ) ) ;
#72081 = CARTESIAN_POINT ( 'NONE',  ( 7.771875000614516971, 3.027376345333611329, 5.243569643749999010 ) ) ;
#72082 = VERTEX_POINT ( 'NONE', #50998 ) ;
#72083 = CARTESIAN_POINT ( 'NONE',  ( 26.78437500061451360, -4.541064518000419881, 2.621784821874995952 ) ) ;
#72084 = CARTESIAN_POINT ( 'NONE',  ( 18.70312500061451644, -4.541064518000417216, -2.621784821875001281 ) ) ;
#72085 = CARTESIAN_POINT ( 'NONE',  ( 29.36250000122903003, -4.330127018922190985, -2.500000000000001332 ) ) ;
#72086 = EDGE_CURVE ( 'NONE', #23724, #40333, #28113, .T. ) ;
#72087 = CARTESIAN_POINT ( 'NONE',  ( 3.946875000614517681, -3.027376345333610441, -5.243569643749999898 ) ) ;
#72088 = CARTESIAN_POINT ( 'NONE',  ( 23.44687500061451502, 6.054752690667223547, 3.707466751127219781E-16 ) ) ;
#72089 = CARTESIAN_POINT ( 'NONE',  ( 18.81562500061452070, 3.027376345333613106, -5.243569643749998122 ) ) ;
#72090 = CARTESIAN_POINT ( 'NONE',  ( 2.000000000000001332, 11.15000000000000213, 33.46410161513774995 ) ) ;
#72091 = CARTESIAN_POINT ( 'NONE',  ( 24.06562500061451715, -6.054752690667223547, -1.112240025338166033E-15 ) ) ;
#72092 = CARTESIAN_POINT ( 'NONE',  ( 4.425000001229032698, 2.886751345948126879, 4.999999999999999112 ) ) ;
#72093 = ORIENTED_EDGE ( 'NONE', *, *, #65868, .F. ) ;
#72094 = CARTESIAN_POINT ( 'NONE',  ( 29.39999999999999858, 4.330127018922192761, -2.499999999999997780 ) ) ;
#72095 = CARTESIAN_POINT ( 'NONE',  ( 4.000000000000000000, 15.68750000000000000, -27.69059892324149530 ) ) ;
#72096 = CARTESIAN_POINT ( 'NONE',  ( -3.756430356250000102, 15.67812499938548143, 30.00000000000000000 ) ) ;
#72097 = CARTESIAN_POINT ( 'NONE',  ( 4.471875000614518925, 3.027376345333613106, -5.243569643749998122 ) ) ;
#72098 = FACE_OUTER_BOUND ( 'NONE', #32910, .T. ) ;
#72099 = CARTESIAN_POINT ( 'NONE',  ( 13.41562500061451502, 3.027376345333613106, -5.243569643749998122 ) ) ;
#72100 = CARTESIAN_POINT ( 'NONE',  ( 6.871875000614517504, 3.027376345333611329, 5.243569643749999010 ) ) ;
#72101 = CARTESIAN_POINT ( 'NONE',  ( 25.31250000122903288, -4.330127018922190985, -2.500000000000001332 ) ) ;
#72102 = CARTESIAN_POINT ( 'NONE',  ( 16.05937500061451573, -4.541064518000417216, -2.621784821875001281 ) ) ;
#72103 = CARTESIAN_POINT ( 'NONE',  ( 28.94062500061452070, -3.027376345333614438, 5.243569643749998122 ) ) ;
#72104 = CARTESIAN_POINT ( 'NONE',  ( 30.00000000000000000, 0.000000000000000000, 0.000000000000000000 ) ) ;
#72105 = VECTOR ( 'NONE', #1101, 1000.000000000000000 ) ;
#72106 = CARTESIAN_POINT ( 'NONE',  ( 4.040625000614517681, 6.054752690667223547, 3.707466751127219781E-16 ) ) ;
#72107 = CARTESIAN_POINT ( 'NONE',  ( 14.57812500061451644, -4.541064518000419881, 2.621784821874995952 ) ) ;
#72108 = EDGE_LOOP ( 'NONE', ( #32117, #40892, #38544, #10134 ) ) ;
#72109 = CARTESIAN_POINT ( 'NONE',  ( 10.11562500061451608, -6.054752690667223547, -1.112240025338166033E-15 ) ) ;
#72110 = CARTESIAN_POINT ( 'NONE',  ( 8.390625000614518214, -3.027376345333610441, -5.243569643749999898 ) ) ;
#72111 = CARTESIAN_POINT ( 'NONE',  ( 18.23437500061451999, -4.119189519843968306, 2.378215178124996054 ) ) ;
#72112 = CARTESIAN_POINT ( 'NONE',  ( 8.062500000000000000, -5.773502691896255534, -1.060575238724906372E-15 ) ) ;
#72113 = EDGE_CURVE ( 'NONE', #26808, #6811, #48153, .T. ) ;
#72114 = CARTESIAN_POINT ( 'NONE',  ( 5.212500001229032343, 4.330127018922192761, -2.499999999999997780 ) ) ;
#72115 = CARTESIAN_POINT ( 'NONE',  ( 19.04999999999999716, 4.330127018922192761, -2.499999999999997780 ) ) ;
#72116 =( BOUNDED_CURVE ( )  B_SPLINE_CURVE ( 2, ( #24562, #59631, #43023, #70725, #30110, #25666, #37105 ),
 .UNSPECIFIED., .F., .F. ) 
 B_SPLINE_CURVE_WITH_KNOTS ( ( 3, 2, 2, 3 ),
 ( 0.2800000000000000266, 0.2833333333333333259, 0.2866666666666667362, 0.2900000000000000355 ),
 .UNSPECIFIED. ) 
 CURVE ( )  GEOMETRIC_REPRESENTATION_ITEM ( )  RATIONAL_B_SPLINE_CURVE ( ( 1.000000000000000000, 0.8660254037844387076, 1.000000000000000000, 0.8660254037844387076, 1.000000000000000000, 0.8660254037844364872, 1.000000000000002220 ) ) 
 REPRESENTATION_ITEM ( '' )  );
#72117 = CARTESIAN_POINT ( 'NONE',  ( 17.89687500061451431, -3.027376345333610441, -5.243569643749999898 ) ) ;
#72118 = CARTESIAN_POINT ( 'NONE',  ( 13.95000000122903572, -2.886751345948129988, 4.999999999999997335 ) ) ;
#72119 = CARTESIAN_POINT ( 'NONE',  ( 20.77500000000000213, 6.123233995736764310E-16, -4.999999999999998224 ) ) ;
#72120 = CARTESIAN_POINT ( 'NONE',  ( 2.121784821874999061, 16.05312500061451786, -33.67503911421598417 ) ) ;
#72121 = CARTESIAN_POINT ( 'NONE',  ( 20.54999999999999716, 0.000000000000000000, 4.999999999999998224 ) ) ;
#72122 = AXIS2_PLACEMENT_3D ( 'NONE', #37328, #10349, #21057 ) ;
#72123 = CARTESIAN_POINT ( 'NONE',  ( 18.91875000122903216, -5.773502691896255534, -1.060575238724906372E-15 ) ) ;
#72124 = CARTESIAN_POINT ( 'NONE',  ( 28.75312500061451715, 4.541064518000418104, -2.621784821874998173 ) ) ;
#72125 = ADVANCED_FACE ( 'NONE', ( #11110, #18357 ), #46, .T. ) ;
#72126 = CARTESIAN_POINT ( 'NONE',  ( 28.27499999999999858, -4.330127018922194537, 2.499999999999995559 ) ) ;
#72127 = CARTESIAN_POINT ( 'NONE',  ( 1.071796769724484344, 16.08259618943233704, -25.99999999999999645 ) ) ;
#72128 = CARTESIAN_POINT ( 'NONE',  ( 13.92187500061451644, 3.027376345333613106, -5.243569643749998122 ) ) ;
#72129 = CARTESIAN_POINT ( 'NONE',  ( 26.06250000000000000, -5.773502691896255534, -1.060575238724906372E-15 ) ) ;
#72130 = CARTESIAN_POINT ( 'NONE',  ( 9.590625000614517504, -3.027376345333614438, 5.243569643749998122 ) ) ;
#72131 = CARTESIAN_POINT ( 'NONE',  ( 27.00937500061451502, 2.746126346562643317, 4.756430356249998326 ) ) ;
#72132 = CARTESIAN_POINT ( 'NONE',  ( 22.62187500061451573, 3.027376345333611329, 5.243569643749999010 ) ) ;
#72133 = CARTESIAN_POINT ( 'NONE',  ( 12.75937500061451502, -5.492252693125287522, -1.008910452111647106E-15 ) ) ;
#72134 = CARTESIAN_POINT ( 'NONE',  ( 7.228125000614517681, 4.541064518000418104, 2.621784821874999949 ) ) ;
#72135 = CARTESIAN_POINT ( 'NONE',  ( 12.94687500061451857, -3.027376345333610441, -5.243569643749999898 ) ) ;
#72136 = EDGE_LOOP ( 'NONE', ( #40284, #21516, #13505, #32764 ) ) ;
#72137 = CARTESIAN_POINT ( 'NONE',  ( 23.22187500061451715, -6.054752690667223547, -1.112240025338166033E-15 ) ) ;
#72138 = CARTESIAN_POINT ( 'NONE',  ( 2.067223061484678048, 4.558648060312520123, -33.43375747538831888 ) ) ;
#72139 = DIRECTION ( 'NONE',  ( -0.000000000000000000, -1.000000000000000000, -0.000000000000000000 ) ) ;
#72140 = CARTESIAN_POINT ( 'NONE',  ( 4.762499999999999289, 2.886751345948126879, 4.999999999999999112 ) ) ;
#72141 = CARTESIAN_POINT ( 'NONE',  ( 18.07500000122903216, -5.773502691896255534, -1.060575238724906372E-15 ) ) ;
#72142 = CARTESIAN_POINT ( 'NONE',  ( 0.000000000000000000, 27.50000000000000000, 30.00000000000000000 ) ) ;
#72143 = CARTESIAN_POINT ( 'NONE',  ( 19.16250000000000142, 2.886751345948060266, 5.000000000000114575 ) ) ;
#72144 = PRESENTATION_LAYER_ASSIGNMENT (  '', '', ( #39139 ) ) ;
#72145 = VERTEX_POINT ( 'NONE', #67994 ) ;
#72146 = CARTESIAN_POINT ( 'NONE',  ( 12.44999999999999929, 0.000000000000000000, 4.999999999999998224 ) ) ;
#72147 = CARTESIAN_POINT ( 'NONE',  ( 16.53750000000000142, -2.886751345948129988, 4.999999999999997335 ) ) ;
#72148 = CARTESIAN_POINT ( 'NONE',  ( 13.08750000122903323, -4.330127018922194537, 2.499999999999995559 ) ) ;
#72149 = CARTESIAN_POINT ( 'NONE',  ( 11.84062500061451750, -3.027376345333614438, 5.243569643749998122 ) ) ;
#72150 = VERTEX_POINT ( 'NONE', #10748 ) ;
#72151 = CARTESIAN_POINT ( 'NONE',  ( 10.08749999999999858, 5.773502691896255534, 3.535250795749688894E-16 ) ) ;
#72152 = CARTESIAN_POINT ( 'NONE',  ( 18.60000000122903430, -2.886751345948159742, -4.999999999999942268 ) ) ;
#72153 = CARTESIAN_POINT ( 'NONE',  ( -2.121784821874996840, 14.53437500061451715, -26.32496088578401583 ) ) ;
#72154 = CARTESIAN_POINT ( 'NONE',  ( 4.303125000614516971, -4.541064518000417216, -2.621784821875001281 ) ) ;
#72155 = CARTESIAN_POINT ( 'NONE',  ( 2.655984681222220721E-16, 13.65312499938548285, 25.66244784525396483 ) ) ;
#72156 = CARTESIAN_POINT ( 'NONE',  ( 9.862500000000000711, -5.773502691896255534, -1.060575238724906372E-15 ) ) ;
#72157 = LINE ( 'NONE', #33358, #9059 ) ;
#72158 = VERTEX_POINT ( 'NONE', #32556 ) ;
#72159 = CARTESIAN_POINT ( 'NONE',  ( 24.85312500061451502, 0.000000000000000000, 5.243569643749999010 ) ) ;
#72160 = CARTESIAN_POINT ( 'NONE',  ( 4.219924060640600771, -2.681835364526683474, 4.505860815252779261 ) ) ;
#72161 = CARTESIAN_POINT ( 'NONE',  ( -3.756430356250000102, 20.06562499938548072, 30.00000000000000000 ) ) ;
#72162 = CARTESIAN_POINT ( 'NONE',  ( 22.24687500061451217, -3.027376345333614438, 5.243569643749998122 ) ) ;
#72163 = CARTESIAN_POINT ( 'NONE',  ( 19.07812500061451644, -4.541064518000419881, 2.621784821874995952 ) ) ;
#72164 = CARTESIAN_POINT ( 'NONE',  ( -4.243569643749998122, 11.74062500061459424, -27.54997392385601174 ) ) ;
#72165 = CARTESIAN_POINT ( 'NONE',  ( 6.440625000614517148, -3.027376345333614438, 5.243569643749998122 ) ) ;
#72166 =( BOUNDED_CURVE ( )  B_SPLINE_CURVE ( 2, ( #31693, #54228, #15415, #37958, #37594, #60478, #32421 ),
 .UNSPECIFIED., .F., .F. ) 
 B_SPLINE_CURVE_WITH_KNOTS ( ( 3, 2, 2, 3 ),
 ( 0.08999999999999996891, 0.09333333333333329596, 0.09666666666666662300, 0.09999999999999995004 ),
 .UNSPECIFIED. ) 
 CURVE ( )  GEOMETRIC_REPRESENTATION_ITEM ( )  RATIONAL_B_SPLINE_CURVE ( ( 1.000000000000001110, 0.8660254037844374864, 1.000000000000000000, 0.8660254037844387076, 1.000000000000000000, 0.8660254037844409281, 0.9999999999999977796 ) ) 
 REPRESENTATION_ITEM ( '' )  );
#72167 = CARTESIAN_POINT ( 'NONE',  ( 3.440625000614518036, -3.027376345333610441, -5.243569643749999898 ) ) ;
#72168 = CARTESIAN_POINT ( 'NONE',  ( 25.17187500061451644, 2.746126346562645981, -4.756430356249997438 ) ) ;
#72169 = CARTESIAN_POINT ( 'NONE',  ( 21.96562500061451928, 3.027376345333612662, -5.243569643749998122 ) ) ;
#72170 = CARTESIAN_POINT ( 'NONE',  ( 9.196875000614518569, -2.746126346562646425, 4.756430356249996549 ) ) ;
#72171 = CARTESIAN_POINT ( 'NONE',  ( 2.655984681222220721E-16, 18.15312499938548285, 25.66244784525396483 ) ) ;
#72172 = CARTESIAN_POINT ( 'NONE',  ( 14.97187500061451892, 3.027376345333611329, 5.243569643749999010 ) ) ;
#72173 = CARTESIAN_POINT ( 'NONE',  ( 14.40937500061451715, 4.541064518000418104, -2.621784821874998173 ) ) ;
#72174 = CARTESIAN_POINT ( 'NONE',  ( 22.62187500061451573, 3.027376345333611329, 5.243569643749999010 ) ) ;
#72175 = ORIENTED_EDGE ( 'NONE', *, *, #64115, .T. ) ;
#72176 = CARTESIAN_POINT ( 'NONE',  ( 4.243569643749999898, 12.39687500061451786, 32.45002607614398471 ) ) ;
#72177 = CARTESIAN_POINT ( 'NONE',  ( 27.22499999999999787, 4.330127018922191873, 2.499999999999999556 ) ) ;
#72179 =( BOUNDED_CURVE ( )  B_SPLINE_CURVE ( 3, ( #72699, #44640, #67169, #16530 ),
 .UNSPECIFIED., .F., .F. ) 
 B_SPLINE_CURVE_WITH_KNOTS ( ( 4, 4 ),
 ( 3.595026063070182243, 3.642474834530476269 ),
 .UNSPECIFIED. ) 
 CURVE ( )  GEOMETRIC_REPRESENTATION_ITEM ( )  RATIONAL_B_SPLINE_CURVE ( ( 1.000000000000000000, 0.9998123933069705815, 0.9998123933069705815, 1.000000000000000000 ) ) 
 REPRESENTATION_ITEM ( '' )  );
#72178 = CARTESIAN_POINT ( 'NONE',  ( 27.55312500061451786, 0.000000000000000000, 5.243569643749999010 ) ) ;
#72180 = CARTESIAN_POINT ( 'NONE',  ( 27.44062500061451715, 6.054752690667223547, 3.707466751127219781E-16 ) ) ;
#72181 = CARTESIAN_POINT ( 'NONE',  ( 3.999999999999998668, 15.16250000000000142, 32.30940107675850470 ) ) ;
#72182 = CARTESIAN_POINT ( 'NONE',  ( 1.999999999999998668, 18.50000000000000000, 26.53589838486224650 ) ) ;
#72183 = CARTESIAN_POINT ( 'NONE',  ( 3.984375000614517326, 6.421520780324663323E-16, -5.243569643749999010 ) ) ;
#72184 = SHAPE_DEFINITION_REPRESENTATION ( #8981, #13196 ) ;
#72185 = CARTESIAN_POINT ( 'NONE',  ( 11.32500000122903394, -5.773502691896255534, -1.060575238724906372E-15 ) ) ;
#72186 = CARTESIAN_POINT ( 'NONE',  ( 10.16250000122903252, 4.330127018922192761, -2.499999999999997780 ) ) ;
#72187 = CARTESIAN_POINT ( 'NONE',  ( 28.98750000122903359, 6.123233995736764310E-16, -4.999999999999998224 ) ) ;
#72188 = CARTESIAN_POINT ( 'NONE',  ( 3.999999999999998668, 16.90624999877096712, 32.30940107675850470 ) ) ;
#72189 = CARTESIAN_POINT ( 'NONE',  ( 19.48125000122903216, 6.123233995736764310E-16, -4.999999999999998224 ) ) ;
#72190 = CARTESIAN_POINT ( 'NONE',  ( 12.98437500061451821, 6.421520780324663323E-16, -5.243569643749999010 ) ) ;
#72191 = CARTESIAN_POINT ( 'NONE',  ( 29.38125000122903074, 6.123233995736764310E-16, -4.999999999999998224 ) ) ;
#72192 = ORIENTED_EDGE ( 'NONE', *, *, #23389, .F. ) ;
#72193 = CARTESIAN_POINT ( 'NONE',  ( 19.00312500061451715, 0.000000000000000000, 5.243569643749999010 ) ) ;
#72194 = CARTESIAN_POINT ( 'NONE',  ( 14.29687500061451821, -3.027376345333610441, -5.243569643749999898 ) ) ;
#72195 = CARTESIAN_POINT ( 'NONE',  ( 4.640625000614518214, -3.027376345333614438, 5.243569643749998122 ) ) ;
#72196 = CARTESIAN_POINT ( 'NONE',  ( 22.77187500061451786, -6.054752690667223547, -1.112240025338166033E-15 ) ) ;
#72197 = CARTESIAN_POINT ( 'NONE',  ( 6.103125000614515905, -4.541064518000417216, -2.621784821875001281 ) ) ;
#72198 = CARTESIAN_POINT ( 'NONE',  ( 6.487500001229034474, 6.123233995736764310E-16, -4.999999999999998224 ) ) ;
#72200 = EDGE_CURVE ( 'NONE', #70765, #54526, #70843, .T. ) ;
#72199 = CARTESIAN_POINT ( 'NONE',  ( 4.987500001229032698, -4.330127018922194537, 2.499999999999995559 ) ) ;
#72201 = CARTESIAN_POINT ( 'NONE',  ( 23.39062500061451289, 6.054752690667223547, 3.707466751127219781E-16 ) ) ;
#72202 =( BOUNDED_CURVE ( )  B_SPLINE_CURVE ( 2, ( #39969, #34766, #63205, #62483, #62128, #12236, #67679, #7065, #45866 ),
 .UNSPECIFIED., .F., .F. ) 
 B_SPLINE_CURVE_WITH_KNOTS ( ( 3, 2, 2, 2, 3 ),
 ( 0.7934782608695651884, 0.7971014492753623060, 0.8043478260869565410, 0.8115942028985507761, 0.8152173913043478937 ),
 .UNSPECIFIED. ) 
 CURVE ( )  GEOMETRIC_REPRESENTATION_ITEM ( )  RATIONAL_B_SPLINE_CURVE ( ( 0.9330127018922194093, 0.9330127018922194093, 1.000000000000000000, 0.8660254037844387076, 1.000000000000000000, 0.8660254037844387076, 1.000000000000000000, 0.9330127018922182991, 0.9330127018922192983 ) ) 
 REPRESENTATION_ITEM ( '' )  );
#72203 = CARTESIAN_POINT ( 'NONE',  ( -2.000000000000000000, 18.68750000122903288, -33.46410161513775705 ) ) ;
#72204 = CARTESIAN_POINT ( 'NONE',  ( 8.400000001229035007, 5.773502691896255534, 3.535250795749688894E-16 ) ) ;
#72205 = CARTESIAN_POINT ( 'NONE',  ( 16.56562500061451715, 3.027376345333613106, -5.243569643749998122 ) ) ;
#72206 = CARTESIAN_POINT ( 'NONE',  ( 14.39062500061451821, 6.054752690667223547, 3.707466751127219781E-16 ) ) ;
#72207 = CARTESIAN_POINT ( 'NONE',  ( 27.12187500061451573, 2.746126346562643317, 4.756430356249998326 ) ) ;
#72208 = CARTESIAN_POINT ( 'NONE',  ( 16.23750000000000071, -2.886751345948125991, -5.000000000000000000 ) ) ;
#72209 = CARTESIAN_POINT ( 'NONE',  ( 11.66250000122903430, 0.000000000000000000, 4.999999999999998224 ) ) ;
#72210 = CARTESIAN_POINT ( 'NONE',  ( 8.165625000614516793, 3.027376345333611329, 5.243569643749999010 ) ) ;
#72211 = CARTESIAN_POINT ( 'NONE',  ( 11.80312500061451608, 0.000000000000000000, 5.243569643749999010 ) ) ;
#72212 = CARTESIAN_POINT ( 'NONE',  ( 19.76250000122903216, 0.000000000000000000, 4.999999999999998224 ) ) ;
#72213 = CARTESIAN_POINT ( 'NONE',  ( 4.243569643749999010, 14.72187500061451715, -32.45002607614398471 ) ) ;
#72214 = CARTESIAN_POINT ( 'NONE',  ( 19.58437500061451786, -4.541064518000419881, 2.621784821874995952 ) ) ;
#72215 = CARTESIAN_POINT ( 'NONE',  ( 9.825000000000001066, -4.330127018922194537, 2.499999999999995559 ) ) ;
#72216 = CARTESIAN_POINT ( 'NONE',  ( 5.175000001229033586, 2.886751345948129099, -4.999999999999998224 ) ) ;
#72217 = CARTESIAN_POINT ( 'NONE',  ( 3.271875000614519635, 3.027376345333611329, 5.243569643749999010 ) ) ;
#72218 = CARTESIAN_POINT ( 'NONE',  ( 20.93437500061451573, -4.541064518000419881, 2.621784821874995952 ) ) ;
#72219 = CARTESIAN_POINT ( 'NONE',  ( 27.56249999999999645, 2.886751345948164182, -4.999999999999937828 ) ) ;
#72220 = CARTESIAN_POINT ( 'NONE',  ( 16.15312500061451573, 4.541064518000418104, -2.621784821874998173 ) ) ;
#72221 = CARTESIAN_POINT ( 'NONE',  ( 11.64375000122903003, -2.886751345948129988, 4.999999999999997335 ) ) ;
#72222 = CARTESIAN_POINT ( 'NONE',  ( 13.27500000000000213, 4.330127018922191873, 2.499999999999999556 ) ) ;
#72223 = CARTESIAN_POINT ( 'NONE',  ( 27.49687500061451217, 6.054752690667223547, 3.707466751127219781E-16 ) ) ;
#72224 = CARTESIAN_POINT ( 'NONE',  ( 19.99687500061451217, -4.119189519843965641, -2.378215178125001383 ) ) ;
#72225 = CARTESIAN_POINT ( 'NONE',  ( 14.46562500061451750, 3.027376345333611329, 5.243569643749999010 ) ) ;
#72226 = CARTESIAN_POINT ( 'NONE',  ( 14.29687500061451821, -3.027376345333610441, -5.243569643749999898 ) ) ;
#72227 = VERTEX_POINT ( 'NONE', #49915 ) ;
#72228 = CARTESIAN_POINT ( 'NONE',  ( 22.31250000122903288, 4.330127018922192761, -2.499999999999997780 ) ) ;
#72229 = CARTESIAN_POINT ( 'NONE',  ( 22.15312500061451573, 0.000000000000000000, 5.243569643749999010 ) ) ;
#72230 = DIRECTION ( 'NONE',  ( 0.000000000000000000, 0.000000000000000000, -1.000000000000000000 ) ) ;
#72231 = CARTESIAN_POINT ( 'NONE',  ( 14.62500000000000000, 4.330127018922191873, 2.499999999999999556 ) ) ;
#72232 = EDGE_CURVE ( 'NONE', #14992, #61789, #70817, .T. ) ;
#72233 = CARTESIAN_POINT ( 'NONE',  ( 11.66249999999999964, -5.773502691896255534, -1.060575238724906372E-15 ) ) ;
#72234 = CARTESIAN_POINT ( 'NONE',  ( 22.98750000122903003, -4.330127018922194537, 2.499999999999995559 ) ) ;
#72235 = CARTESIAN_POINT ( 'NONE',  ( 17.54062500061451502, 6.054752690667223547, 3.707466751127219781E-16 ) ) ;
#72236 = ORIENTED_EDGE ( 'NONE', *, *, #17352, .T. ) ;
#72237 = CARTESIAN_POINT ( 'NONE',  ( 20.43749999999999645, 5.773502691896255534, 3.535250795749688894E-16 ) ) ;
#72238 = CARTESIAN_POINT ( 'NONE',  ( 20.55937500061451573, -4.541064518000417216, -2.621784821875001281 ) ) ;
#72239 = ORIENTED_EDGE ( 'NONE', *, *, #25043, .F. ) ;
#72240 = DIRECTION ( 'NONE',  ( -1.000000000000000000, -0.000000000000000000, -0.000000000000000000 ) ) ;
#72241 = CARTESIAN_POINT ( 'NONE',  ( 10.45312500061451644, 0.000000000000000000, 5.243569643749999010 ) ) ;
#72242 = CARTESIAN_POINT ( 'NONE',  ( 10.91249999999999964, 2.886751345948018077, -5.000000000000190070 ) ) ;
#72243 = CARTESIAN_POINT ( 'NONE',  ( 13.05937500061451573, 2.746126346562643317, 4.756430356249998326 ) ) ;
#72244 = CARTESIAN_POINT ( 'NONE',  ( 16.50000000000000000, 0.000000000000000000, 4.999999999999998224 ) ) ;
#72245 = CARTESIAN_POINT ( 'NONE',  ( 24.18750000000000355, -2.886751345948129988, 4.999999999999997335 ) ) ;
#72246 = CYLINDRICAL_SURFACE ( 'NONE', #5036, 4.999999999999998224 ) ;
#72247 = CARTESIAN_POINT ( 'NONE',  ( 3.459375000614519635, -4.541064518000417216, -2.621784821875001281 ) ) ;
#72248 = CARTESIAN_POINT ( 'NONE',  ( 27.49687500061451217, 6.054752690667223547, 3.707466751127219781E-16 ) ) ;
#72249 = ORIENTED_EDGE ( 'NONE', *, *, #46464, .T. ) ;
#72250 = CARTESIAN_POINT ( 'NONE',  ( 26.12812500061451360, 4.541064518000418104, 2.621784821874999949 ) ) ;
#72251 = CARTESIAN_POINT ( 'NONE',  ( 27.79687500061451999, -3.027376345333610441, -5.243569643749999898 ) ) ;
#72252 = LINE ( 'NONE', #9097, #36859 ) ;
#72253 = CARTESIAN_POINT ( 'NONE',  ( 14.73749999999999893, -2.886751345948129988, 4.999999999999997335 ) ) ;
#72254 = CARTESIAN_POINT ( 'NONE',  ( 10.64062500061451644, -3.027376345333610441, -5.243569643749999898 ) ) ;
#72255 = DIRECTION ( 'NONE',  ( 0.000000000000000000, 0.000000000000000000, -1.000000000000000000 ) ) ;
#72256 = CARTESIAN_POINT ( 'NONE',  ( 0.000000000000000000, 20.00000000000000000, -30.00000000000000000 ) ) ;
#72257 = CARTESIAN_POINT ( 'NONE',  ( 27.70312500061451289, -4.541064518000417216, -2.621784821875001281 ) ) ;
#72258 = CARTESIAN_POINT ( 'NONE',  ( 16.95000000122903216, 5.773502691896255534, 3.535250795749688894E-16 ) ) ;
#72259 = CARTESIAN_POINT ( 'NONE',  ( 28.99687500061451217, -4.119189519843965641, -2.378215178125001383 ) ) ;
#72260 = CARTESIAN_POINT ( 'NONE',  ( 15.38437500061451679, 4.119189519843966529, 2.378215178124999607 ) ) ;
#72261 = CARTESIAN_POINT ( 'NONE',  ( 6.065625000614516260, -6.054752690667223547, -1.112240025338166033E-15 ) ) ;
#72262 = CARTESIAN_POINT ( 'NONE',  ( 22.32187500061451502, -6.054752690667223547, -1.112240025338166033E-15 ) ) ;
#72263 = CARTESIAN_POINT ( 'NONE',  ( -4.243569643749997233, 15.84687500061451715, 32.45002607614398471 ) ) ;
#72264 = CARTESIAN_POINT ( 'NONE',  ( 20.97187500061451715, -6.054752690667223547, -1.112240025338166033E-15 ) ) ;
#72265 = CARTESIAN_POINT ( 'NONE',  ( 28.92187500061451644, 3.027376345333611329, 5.243569643749999010 ) ) ;
#72266 = CARTESIAN_POINT ( 'NONE',  ( -4.243569643749999898, 18.02187500061451786, 27.54997392385601529 ) ) ;
#72267 = CARTESIAN_POINT ( 'NONE',  ( 9.478125000614515017, 4.541064518000418104, 2.621784821874999949 ) ) ;
#72268 = CARTESIAN_POINT ( 'NONE',  ( 26.39999999999999858, 0.000000000000000000, 4.999999999999998224 ) ) ;
#72269 = CIRCLE ( 'NONE', #69923, 9.000000000000000000 ) ;
#72270 = CARTESIAN_POINT ( 'NONE',  ( 6.871875000614517504, 3.027376345333611329, 5.243569643749999010 ) ) ;
#72271 = CYLINDRICAL_SURFACE ( 'NONE', #13544, 3.999999999999996447 ) ;
#72272 = CARTESIAN_POINT ( 'NONE',  ( 6.928125000614516082, -4.541064518000419881, 2.621784821874995952 ) ) ;
#72273 = CARTESIAN_POINT ( 'NONE',  ( 11.25937500061451679, 4.541064518000418104, -2.621784821874998173 ) ) ;
#72274 = CARTESIAN_POINT ( 'NONE',  ( 3.450849747961474367, -3.618245071504076371, -3.795178659245230790 ) ) ;
#72275 = CARTESIAN_POINT ( 'NONE',  ( 22.38750000122903216, 4.330127018922191873, 2.499999999999999556 ) ) ;
#72276 = CARTESIAN_POINT ( 'NONE',  ( 7.321875000614516793, 3.027376345333611329, 5.243569643749999010 ) ) ;
#72277 = CARTESIAN_POINT ( 'NONE',  ( 10.64062500061451644, -3.027376345333610441, -5.243569643749999898 ) ) ;
#72278 = CARTESIAN_POINT ( 'NONE',  ( 25.74375000122903501, -2.886751345948125991, -5.000000000000000000 ) ) ;
#72279 = CARTESIAN_POINT ( 'NONE',  ( 19.20937500061451786, -4.541064518000417216, -2.621784821875001281 ) ) ;
#72280 = CARTESIAN_POINT ( 'NONE',  ( -2.482458701038963156, 4.346511033910187116, 33.14667641405304011 ) ) ;
#72281 = CARTESIAN_POINT ( 'NONE',  ( 29.03437500061451715, -4.541064518000419881, 2.621784821874995952 ) ) ;
#72282 = EDGE_CURVE ( 'NONE', #62319, #13801, #58486, .T. ) ;
#72283 = CARTESIAN_POINT ( 'NONE',  ( -4.243569643749999898, 12.65937500061451715, -30.00000000000000000 ) ) ;
#72284 = CARTESIAN_POINT ( 'NONE',  ( 14.55000000122903181, -2.886751345948125991, -5.000000000000000000 ) ) ;
#72285 = CARTESIAN_POINT ( 'NONE',  ( 4.243569643749999898, 15.97812500061451857, -30.00000000000000000 ) ) ;
#72286 = CARTESIAN_POINT ( 'NONE',  ( 14.36250000122903359, 0.000000000000000000, 4.999999999999998224 ) ) ;
#72287 = CARTESIAN_POINT ( 'NONE',  ( 9.478125000614515017, 4.541064518000418104, 2.621784821874999949 ) ) ;
#72288 = ORIENTED_EDGE ( 'NONE', *, *, #17583, .T. ) ;
#72289 = CARTESIAN_POINT ( 'NONE',  ( 13.79999999999999893, 0.000000000000000000, 4.999999999999998224 ) ) ;
#72290 = CARTESIAN_POINT ( 'NONE',  ( 10.29375000122902861, -2.886751345948019409, 5.000000000000189182 ) ) ;
#72291 = CARTESIAN_POINT ( 'NONE',  ( 21.81562500061451004, -6.054752690667223547, -1.112240025338166033E-15 ) ) ;
#72292 = CARTESIAN_POINT ( 'NONE',  ( 6.984375000614516438, -4.541064518000419881, 2.621784821874995952 ) ) ;
#72293 = CARTESIAN_POINT ( 'NONE',  ( 11.25000000122903288, -2.886751345948129988, 4.999999999999997335 ) ) ;
#72294 = CARTESIAN_POINT ( 'NONE',  ( 18.03750000122903430, -4.330127018922194537, 2.499999999999995559 ) ) ;
#72295 = CARTESIAN_POINT ( 'NONE',  ( 16.22812500061451857, 4.541064518000418104, 2.621784821874999949 ) ) ;
#72296 = CARTESIAN_POINT ( 'NONE',  ( 18.21562500061451573, -6.054752690667223547, -1.112240025338166033E-15 ) ) ;
#72297 = CARTESIAN_POINT ( 'NONE',  ( 24.90000000122903145, -2.886751345948125991, -5.000000000000000000 ) ) ;
#72298 = CARTESIAN_POINT ( 'NONE',  ( 27.78750000122903074, 4.330127018922191873, 2.499999999999999556 ) ) ;
#72299 = CARTESIAN_POINT ( 'NONE',  ( 23.43750000000000000, -2.886751345948125991, -5.000000000000000000 ) ) ;
#72300 = CARTESIAN_POINT ( 'NONE',  ( -3.756430356250001434, 13.80312499938548321, 32.16877607737301048 ) ) ;
#72301 = CARTESIAN_POINT ( 'NONE',  ( 26.40937500061451715, -4.541064518000417216, -2.621784821875001281 ) ) ;
#72302 = CARTESIAN_POINT ( 'NONE',  ( 65.00000000000000000, 6.363961030679004871, 6.363961030678849440 ) ) ;
#72303 = CARTESIAN_POINT ( 'NONE',  ( 13.42500000122903536, 2.886751345948126879, 4.999999999999999112 ) ) ;
#72304 = CARTESIAN_POINT ( 'NONE',  ( 27.79687500061451999, -3.027376345333610441, -5.243569643749999898 ) ) ;
#72305 = DIRECTION ( 'NONE',  ( 0.000000000000000000, -0.000000000000000000, -1.000000000000000000 ) ) ;
#72306 = CARTESIAN_POINT ( 'NONE',  ( 4.809375000614516615, -4.541064518000417216, -2.621784821875001281 ) ) ;
#72307 = CARTESIAN_POINT ( 'NONE',  ( 25.34062500061451217, -3.027376345333614438, 5.243569643749998122 ) ) ;
#72308 = CARTESIAN_POINT ( 'NONE',  ( -1.878215178124999163, 15.60312499938548392, 26.74683588394047007 ) ) ;
#72309 = CARTESIAN_POINT ( 'NONE',  ( 65.00000000000000000, 5.218601775200109039, -7.332543590861101634 ) ) ;
#72310 = CARTESIAN_POINT ( 'NONE',  ( 10.28437500061451715, 6.421520780324663323E-16, -5.243569643749999010 ) ) ;
#72311 = CARTESIAN_POINT ( 'NONE',  ( 4.270834433354036008, -2.600094210001211437, 4.505651273120875544 ) ) ;
#72312 = CARTESIAN_POINT ( 'NONE',  ( 3.009375000614516793, -4.541064518000417216, -2.621784821875001281 ) ) ;
#72313 = CARTESIAN_POINT ( 'NONE',  ( 9.609375000614518214, 0.000000000000000000, 5.243569643749999010 ) ) ;
#72314 = CARTESIAN_POINT ( 'NONE',  ( 28.54687500061451644, -3.027376345333614438, 5.243569643749998122 ) ) ;
#72315 = CARTESIAN_POINT ( 'NONE',  ( 2.121784821874999061, 12.90312500061459566, 26.32496088578401583 ) ) ;
#72316 = CARTESIAN_POINT ( 'NONE',  ( 20.28750000000000142, -2.886751345948125991, -5.000000000000000000 ) ) ;
#72317 = ORIENTED_EDGE ( 'NONE', *, *, #53813, .F. ) ;
#72318 = CARTESIAN_POINT ( 'NONE',  ( 28.91250000000000497, 2.886751345948129099, -4.999999999999998224 ) ) ;
#72319 = ADVANCED_FACE ( 'NONE', ( #69363 ), #25746, .T. ) ;
#72320 = CARTESIAN_POINT ( 'NONE',  ( 5.025000000000002132, 6.123233995736764310E-16, -4.999999999999998224 ) ) ;
#72321 = ORIENTED_EDGE ( 'NONE', *, *, #47314, .F. ) ;
#72322 = CARTESIAN_POINT ( 'NONE',  ( 16.90312500061451573, -4.541064518000417216, -2.621784821875001281 ) ) ;
#72323 = CARTESIAN_POINT ( 'NONE',  ( 8.165625000614516793, 3.027376345333611329, 5.243569643749999010 ) ) ;
#72324 = CARTESIAN_POINT ( 'NONE',  ( 20.97187500061451715, 5.824947211148865298E-16, -4.756430356249998326 ) ) ;
#72325 = CARTESIAN_POINT ( 'NONE',  ( 7.771875000614516971, 3.027376345333611329, 5.243569643749999010 ) ) ;
#72326 = CARTESIAN_POINT ( 'NONE',  ( 18.90000000122902790, -2.886751345948129988, 4.999999999999997335 ) ) ;
#72327 = CARTESIAN_POINT ( 'NONE',  ( 3.199564126591990743, -3.842561905972809555, -3.199564126591990743 ) ) ;
#72328 = CARTESIAN_POINT ( 'NONE',  ( 6.984375000614516438, -4.541064518000419881, 2.621784821874995952 ) ) ;
#72329 = CARTESIAN_POINT ( 'NONE',  ( 12.34687500061452070, -3.027376345333614438, 5.243569643749998122 ) ) ;
#72330 = CARTESIAN_POINT ( 'NONE',  ( 24.04687500061451644, -3.027376345333614438, 5.243569643749998122 ) ) ;
#72331 = CARTESIAN_POINT ( 'NONE',  ( 34.99999999999999289, 2.500000000000000444, 3.499999999999999112 ) ) ;
#72332 = ORIENTED_EDGE ( 'NONE', *, *, #45751, .F. ) ;
#72333 = CARTESIAN_POINT ( 'NONE',  ( 10.12500000000000178, 4.330127018922191873, 2.499999999999999556 ) ) ;
#72334 = CARTESIAN_POINT ( 'NONE',  ( 17.14687500061451786, 6.054752690667223547, 3.707466751127219781E-16 ) ) ;
#72335 = CARTESIAN_POINT ( 'NONE',  ( 8.746875000614515727, -3.027376345333614438, 5.243569643749998122 ) ) ;
#72336 = CARTESIAN_POINT ( 'NONE',  ( 1.878215178124997609, 14.36562499938548321, 33.25316411605952993 ) ) ;
#72337 = CARTESIAN_POINT ( 'NONE',  ( 21.82499999999999574, 4.330127018922191873, 2.499999999999999556 ) ) ;
#72338 = CARTESIAN_POINT ( 'NONE',  ( 2.828200636599751609E-16, 16.66249999999999787, 25.38119784648299415 ) ) ;
#72339 = CARTESIAN_POINT ( 'NONE',  ( 22.17187500061451644, 2.746126346562643317, 4.756430356249998326 ) ) ;
#72340 = CARTESIAN_POINT ( 'NONE',  ( 12.47812500061451502, 6.421520780324663323E-16, -5.243569643749999010 ) ) ;
#72341 = CARTESIAN_POINT ( 'NONE',  ( 28.95937500061451431, 0.000000000000000000, 5.243569643749999010 ) ) ;
#72342 = DIRECTION ( 'NONE',  ( 0.000000000000000000, -8.673617379884036705E-17, -1.000000000000000000 ) ) ;
#72343 = CARTESIAN_POINT ( 'NONE',  ( 29.44687500061451857, -3.027376345333614438, 5.243569643749998122 ) ) ;
#72344 = CARTESIAN_POINT ( 'NONE',  ( 10.68750000000000000, -2.886751345948129988, 4.999999999999997335 ) ) ;
#72345 = CARTESIAN_POINT ( 'NONE',  ( 1.999999999999998668, 15.91250000122903430, 26.53589838486224650 ) ) ;
#72346 = CARTESIAN_POINT ( 'NONE',  ( 7.987500001229032698, 4.330127018922191873, 2.499999999999999556 ) ) ;
#72347 = CARTESIAN_POINT ( 'NONE',  ( 20.44687500061451857, -3.027376345333614438, 5.243569643749998122 ) ) ;
#72348 = CARTESIAN_POINT ( 'NONE',  ( 14.89687500061451786, 6.054752690667223547, 3.707466751127219781E-16 ) ) ;
#72349 = CARTESIAN_POINT ( 'NONE',  ( -2.000000000000000000, 12.27500000000000036, 26.53589838486224650 ) ) ;
#72350 = VERTEX_POINT ( 'NONE', #46826 ) ;
#72351 = CARTESIAN_POINT ( 'NONE',  ( 17.80312500061451786, -4.541064518000417216, -2.621784821875001281 ) ) ;
#72352 = CARTESIAN_POINT ( 'NONE',  ( 27.90000000122903145, -2.886751345948129988, 4.999999999999997335 ) ) ;
#72353 = CARTESIAN_POINT ( 'NONE',  ( 16.28437500061452070, 4.541064518000418104, 2.621784821874999949 ) ) ;
#72354 = CARTESIAN_POINT ( 'NONE',  ( 5.800002967315412761, 8.146762937617081590, -31.58794104515360601 ) ) ;
#72355 = CARTESIAN_POINT ( 'NONE',  ( 17.54062500061451502, 6.054752690667223547, 3.707466751127219781E-16 ) ) ;
#72356 = CARTESIAN_POINT ( 'NONE',  ( 1.071796769724476572, 14.39509619066136636, -25.99999999999999289 ) ) ;
#72357 = CARTESIAN_POINT ( 'NONE',  ( 25.35937500061451644, 0.000000000000000000, 5.243569643749999010 ) ) ;
#72358 = CARTESIAN_POINT ( 'NONE',  ( 4.243569643749999898, 12.79062500061451679, 32.45002607614398471 ) ) ;
#72359 = CARTESIAN_POINT ( 'NONE',  ( 15.98437500061451821, -4.541064518000419881, 2.621784821874995952 ) ) ;
#72360 = CARTESIAN_POINT ( 'NONE',  ( 14.77500000122903501, 2.886751345948126879, 4.999999999999999112 ) ) ;
#72361 = CARTESIAN_POINT ( 'NONE',  ( 9.609375000614518214, 0.000000000000000000, 4.756430356249998326 ) ) ;
#72362 = CARTESIAN_POINT ( 'NONE',  ( -2.121784821874996840, 19.48437500061451644, -26.32496088578401583 ) ) ;
#72363 = CARTESIAN_POINT ( 'NONE',  ( 21.15937500061451715, 4.541064518000418104, -2.621784821874998173 ) ) ;
#72364 = CARTESIAN_POINT ( 'NONE',  ( 23.36250000122903359, 0.000000000000000000, 4.999999999999998224 ) ) ;
#72365 = EDGE_CURVE ( 'NONE', #16786, #50451, #66067, .T. ) ;
#72366 = CARTESIAN_POINT ( 'NONE',  ( 18.00937500061451502, 4.541064518000418104, -2.621784821874998173 ) ) ;
#72367 = CARTESIAN_POINT ( 'NONE',  ( 12.66562500061451502, 3.027376345333611329, 5.243569643749999010 ) ) ;
#72368 = CARTESIAN_POINT ( 'NONE',  ( -2.121784821874996840, 13.18437500061451750, 33.67503911421598417 ) ) ;
#72369 = CARTESIAN_POINT ( 'NONE',  ( 17.99062500061451786, 6.054752690667223547, 3.707466751127219781E-16 ) ) ;
#72370 = ORIENTED_EDGE ( 'NONE', *, *, #11236, .F. ) ;
#72371 = ORIENTED_EDGE ( 'NONE', *, *, #8883, .T. ) ;
#72372 = CARTESIAN_POINT ( 'NONE',  ( 20.58750000000000213, -2.886751345948129988, 4.999999999999997335 ) ) ;
#72373 = CARTESIAN_POINT ( 'NONE',  ( 28.31250000122903288, 0.000000000000000000, 4.999999999999998224 ) ) ;
#72374 = CARTESIAN_POINT ( 'NONE',  ( 25.22812500061451502, 4.541064518000418104, 2.621784821874999949 ) ) ;
#72375 = CARTESIAN_POINT ( 'NONE',  ( 5.053125000614517859, 0.000000000000000000, 5.243569643749999010 ) ) ;
#72376 = CARTESIAN_POINT ( 'NONE',  ( 17.85000000122903430, 5.773502691896255534, 3.535250795749688894E-16 ) ) ;
#72377 = CARTESIAN_POINT ( 'NONE',  ( 23.27812500061451573, 6.421520780324663323E-16, -5.243569643749999010 ) ) ;
#72378 = CARTESIAN_POINT ( 'NONE',  ( 22.16250000000000142, 2.886751345948129099, -4.999999999999998224 ) ) ;
#72379 = CARTESIAN_POINT ( 'NONE',  ( 25.71562500061451573, 3.027376345333611329, 5.243569643749999010 ) ) ;
#72380 = CARTESIAN_POINT ( 'NONE',  ( 6.215625000614517504, 3.027376345333613106, -5.243569643749998122 ) ) ;
#72381 = ORIENTED_EDGE ( 'NONE', *, *, #36827, .T. ) ;
#72382 = CARTESIAN_POINT ( 'NONE',  ( 29.32499999999999929, 6.123233995736764310E-16, -4.999999999999998224 ) ) ;
#72383 = CARTESIAN_POINT ( 'NONE',  ( 2.915625000614516793, -6.054752690667223547, -1.112240025338166033E-15 ) ) ;
#72384 = CARTESIAN_POINT ( 'NONE',  ( 12.00937500061451857, -4.119189519843965641, -2.378215178125001383 ) ) ;
#72385 = CARTESIAN_POINT ( 'NONE',  ( 3.999999999999999112, 14.48750000122903536, -30.00000000000000000 ) ) ;
#72386 = CARTESIAN_POINT ( 'NONE',  ( 2.121784821875001281, 18.20937500061451786, -26.32496088578401938 ) ) ;
#72387 = CARTESIAN_POINT ( 'NONE',  ( 11.88749999999999751, 5.773502691896255534, 3.535250795749688894E-16 ) ) ;
#72388 =( BOUNDED_CURVE ( )  B_SPLINE_CURVE ( 2, ( #57167, #18000, #62720, #45742, #6579, #68277, #7656 ),
 .UNSPECIFIED., .F., .F. ) 
 B_SPLINE_CURVE_WITH_KNOTS ( ( 3, 2, 2, 3 ),
 ( 0.1166666666666666824, 0.1194444444444444642, 0.1222222222222222182, 0.1250000000000000000 ),
 .UNSPECIFIED. ) 
 CURVE ( )  GEOMETRIC_REPRESENTATION_ITEM ( )  RATIONAL_B_SPLINE_CURVE ( ( 0.9999999999999993339, 0.8660254037844393737, 1.000000000000000000, 0.8660254037844387076, 1.000000000000000000, 0.8660254037844387076, 1.000000000000000000 ) ) 
 REPRESENTATION_ITEM ( '' )  );
#72389 = CARTESIAN_POINT ( 'NONE',  ( 9.309375000614517504, -4.541064518000417216, -2.621784821875001281 ) ) ;
#72390 = CARTESIAN_POINT ( 'NONE',  ( 6.450000001229034829, -2.886751345948125991, -5.000000000000000000 ) ) ;
#72391 = CARTESIAN_POINT ( 'NONE',  ( 12.19687500061451679, 6.054752690667223547, 3.707466751127219781E-16 ) ) ;
#72392 = CARTESIAN_POINT ( 'NONE',  ( 6.909375000614518036, 0.000000000000000000, 5.243569643749999010 ) ) ;
#72393 = CARTESIAN_POINT ( 'NONE',  ( 27.97500000000000142, 6.123233995736764310E-16, -4.999999999999998224 ) ) ;
#72394 = LINE ( 'NONE', #26609, #571 ) ;
#72395 = CARTESIAN_POINT ( 'NONE',  ( 11.33437500061451608, 4.541064518000418104, 2.621784821874999949 ) ) ;
#72396 = FACE_OUTER_BOUND ( 'NONE', #19337, .T. ) ;
#72397 = CARTESIAN_POINT ( 'NONE',  ( 20.65312500061451573, 4.541064518000418104, -2.621784821874998173 ) ) ;
#72398 = DIRECTION ( 'NONE',  ( -0.000000000000000000, -1.000000000000000000, -0.000000000000000000 ) ) ;
#72399 = CARTESIAN_POINT ( 'NONE',  ( 0.000000000000000000, 20.00000000000000000, -30.00000000000000000 ) ) ;
#72400 = CARTESIAN_POINT ( 'NONE',  ( 23.37187500061451573, 3.027376345333613106, -5.243569643749998122 ) ) ;
#72401 = CARTESIAN_POINT ( 'NONE',  ( 4.428044609675158227, 2.322158679919935409, 4.428044609675073850 ) ) ;
#72402 = CARTESIAN_POINT ( 'NONE',  ( 28.27500000122903145, 2.886751345948126879, 4.999999999999999112 ) ) ;
#72403 = CARTESIAN_POINT ( 'NONE',  ( 20.85937500061451644, -5.492252693125287522, -1.008910452111647106E-15 ) ) ;
#72404 = CARTESIAN_POINT ( 'NONE',  ( 24.29062500061451502, 6.054752690667223547, 3.707466751127219781E-16 ) ) ;
#72405 = CARTESIAN_POINT ( 'NONE',  ( 15.89062500061451289, -3.027376345333614438, 5.243569643749998122 ) ) ;
#72406 = CARTESIAN_POINT ( 'NONE',  ( 14.86875000122903323, -5.773502691896255534, -1.060575238724906372E-15 ) ) ;
#72407 = CARTESIAN_POINT ( 'NONE',  ( 14.44687500061451679, 6.054752690667223547, 3.707466751127219781E-16 ) ) ;
#72408 = CARTESIAN_POINT ( 'NONE',  ( 7.275000001229035007, -5.773502691896255534, -1.060575238724906372E-15 ) ) ;
#72409 = CARTESIAN_POINT ( 'NONE',  ( 24.52500000122903145, 2.886751345948129099, -4.999999999999998224 ) ) ;
#72410 = CARTESIAN_POINT ( 'NONE',  ( 4.546875000614517326, 6.054752690667223547, 3.707466751127219781E-16 ) ) ;
#72411 = CARTESIAN_POINT ( 'NONE',  ( 14.44687500061451679, 6.054752690667223547, 3.707466751127219781E-16 ) ) ;
#72412 = CARTESIAN_POINT ( 'NONE',  ( 16.19999999999999929, -4.330127018922190985, -2.500000000000001332 ) ) ;
#72413 = CARTESIAN_POINT ( 'NONE',  ( 21.78750000000000142, 5.773502691896255534, 3.535250795749688401E-16 ) ) ;
#72414 = CARTESIAN_POINT ( 'NONE',  ( 3.187500001229033764, -4.330127018922194537, 2.499999999999995559 ) ) ;
#72415 = CARTESIAN_POINT ( 'NONE',  ( 25.35937500061451644, 0.000000000000000000, 5.243569643749999010 ) ) ;
#72416 = CARTESIAN_POINT ( 'NONE',  ( 16.17187500061451644, 3.027376345333613106, -5.243569643749998122 ) ) ;
#72417 = CARTESIAN_POINT ( 'NONE',  ( -3.756430356250000102, 17.02812499938548285, 30.00000000000000000 ) ) ;
#72418 = CARTESIAN_POINT ( 'NONE',  ( 27.44999999999999929, -4.330127018922190985, -2.500000000000001332 ) ) ;
#72419 = CARTESIAN_POINT ( 'NONE',  ( 3.300000001229034918, -2.886751345948125991, -5.000000000000000000 ) ) ;
#72420 = CARTESIAN_POINT ( 'NONE',  ( 4.875000000000000888, -4.330127018922194537, 2.499999999999995559 ) ) ;
#72421 = CARTESIAN_POINT ( 'NONE',  ( 7.321875000614517681, -4.119189519843968306, 2.378215178124996054 ) ) ;
#72422 = CARTESIAN_POINT ( 'NONE',  ( 20.27812500061451573, 4.541064518000418104, 2.621784821874999949 ) ) ;
#72423 = CARTESIAN_POINT ( 'NONE',  ( 10.38750000000000107, -2.886751345948125991, -5.000000000000000000 ) ) ;
#72424 = CARTESIAN_POINT ( 'NONE',  ( 3.290625000614516793, -3.027376345333614438, 5.243569643749998122 ) ) ;
#72425 = CARTESIAN_POINT ( 'NONE',  ( 17.39999999999999858, 0.000000000000000000, 4.999999999999998224 ) ) ;
#72426 = CYLINDRICAL_SURFACE ( 'NONE', #69108, 4.999999999999998224 ) ;
#72427 = CARTESIAN_POINT ( 'NONE',  ( 20.17500000122903359, 2.886751345948126879, 4.999999999999999112 ) ) ;
#72428 = DIRECTION ( 'NONE',  ( 0.000000000000000000, 0.000000000000000000, -1.000000000000000000 ) ) ;
#72429 = CARTESIAN_POINT ( 'NONE',  ( 29.29687500061451644, 6.054752690667223547, 3.707466751127219781E-16 ) ) ;
#72430 = ORIENTED_EDGE ( 'NONE', *, *, #29578, .F. ) ;
#72431 = CARTESIAN_POINT ( 'NONE',  ( 17.24062500061451786, -3.027376345333614438, 5.243569643749998122 ) ) ;
#72432 = CARTESIAN_POINT ( 'NONE',  ( 25.04062500061451502, -3.027376345333610441, -5.243569643749999898 ) ) ;
#72433 = CARTESIAN_POINT ( 'NONE',  ( 21.98437500061451644, 6.421520780324663323E-16, -5.243569643749999010 ) ) ;
#72434 = CARTESIAN_POINT ( 'NONE',  ( 6.150000000000003020, 0.000000000000000000, 4.999999999999998224 ) ) ;
#72435 = CARTESIAN_POINT ( 'NONE',  ( 9.403125000614517504, 4.541064518000418104, -2.621784821874998173 ) ) ;
#72436 = CARTESIAN_POINT ( 'NONE',  ( 23.16562500061451502, -6.054752690667223547, -1.112240025338166033E-15 ) ) ;
#72437 = CARTESIAN_POINT ( 'NONE',  ( 15.19687500061451857, -3.027376345333610441, -5.243569643749999898 ) ) ;
#72438 = CARTESIAN_POINT ( 'NONE',  ( 19.20937500061451786, -4.541064518000417216, -2.621784821875001281 ) ) ;
#72439 = CARTESIAN_POINT ( 'NONE',  ( 2.000000000000001332, 11.71250000122903501, -26.53589838486224650 ) ) ;
#72440 = CARTESIAN_POINT ( 'NONE',  ( 9.001249775931846008E-16, 10.97187500061451715, 34.90005215228797653 ) ) ;
#72441 = CARTESIAN_POINT ( 'NONE',  ( 20.85000000122903430, -2.886751345948125991, -5.000000000000000000 ) ) ;
#72442 = CARTESIAN_POINT ( 'NONE',  ( 16.92187500061451999, -5.492252693125287522, -1.008910452111647106E-15 ) ) ;
#72443 = CARTESIAN_POINT ( 'NONE',  ( 10.79062500061451679, 6.054752690667223547, 3.707466751127219781E-16 ) ) ;
#72444 = CARTESIAN_POINT ( 'NONE',  ( 7.284375000614518036, 4.541064518000418104, 2.621784821874999949 ) ) ;
#72445 = CARTESIAN_POINT ( 'NONE',  ( 6.834375000614518747, 4.541064518000418104, 2.621784821874999949 ) ) ;
#72446 = ORIENTED_EDGE ( 'NONE', *, *, #57275, .T. ) ;
#72447 = CARTESIAN_POINT ( 'NONE',  ( 28.58437500061451786, -4.541064518000419881, 2.621784821874995952 ) ) ;
#72448 = CARTESIAN_POINT ( 'NONE',  ( 18.25312500061451715, -4.541064518000417216, -2.621784821875001281 ) ) ;
#72449 = CARTESIAN_POINT ( 'NONE',  ( 29.17500000122903714, 2.886751345948126879, 4.999999999999999112 ) ) ;
#72450 = EDGE_CURVE ( 'NONE', #47076, #29843, #25372, .T. ) ;
#72451 = CARTESIAN_POINT ( 'NONE',  ( 28.11562500061451431, -6.054752690667223547, -1.112240025338166033E-15 ) ) ;
#72452 = CARTESIAN_POINT ( 'NONE',  ( 24.68437500061451573, 6.421520780324663323E-16, -5.243569643749999010 ) ) ;
#72453 = CARTESIAN_POINT ( 'NONE',  ( 19.94062500061451715, -3.027376345333614438, 5.243569643749998122 ) ) ;
#72454 = CARTESIAN_POINT ( 'NONE',  ( -4.243569643749999898, 19.82187500061451857, 27.54997392385601529 ) ) ;
#72455 = CARTESIAN_POINT ( 'NONE',  ( 25.04062500061451502, -3.027376345333610441, -5.243569643749999898 ) ) ;
#72456 = CARTESIAN_POINT ( 'NONE',  ( 3.712500001229034563, -4.330127018922190985, -2.500000000000001332 ) ) ;
#72457 = VERTEX_POINT ( 'NONE', #2127 ) ;
#72458 = CARTESIAN_POINT ( 'NONE',  ( 28.46249999999999858, 2.886751345948129099, -4.999999999999998224 ) ) ;
#72459 = CARTESIAN_POINT ( 'NONE',  ( 3.999999999999998668, 15.76249999999999751, -32.30940107675850470 ) ) ;
#72460 = CARTESIAN_POINT ( 'NONE',  ( -7.967954043666661671E-16, 18.04062499938548214, 34.33755215474603517 ) ) ;
#72461 = CARTESIAN_POINT ( 'NONE',  ( 3.871875000614519280, -6.054752690667223547, -1.112240025338166033E-15 ) ) ;
#72462 = CARTESIAN_POINT ( 'NONE',  ( 12.44062500061451537, -3.027376345333610441, -5.243569643749999898 ) ) ;
#72463 = CARTESIAN_POINT ( 'NONE',  ( 6.271875000614517859, 3.027376345333613106, -5.243569643749998122 ) ) ;
#72464 = CARTESIAN_POINT ( 'NONE',  ( 23.62500000122902932, 2.886751345948129099, -4.999999999999998224 ) ) ;
#72465 = CARTESIAN_POINT ( 'NONE',  ( 14.82187500061451502, 3.027376345333612662, -5.243569643749998122 ) ) ;
#72466 = CARTESIAN_POINT ( 'NONE',  ( 2.971875000614517592, -6.054752690667223547, -1.112240025338166033E-15 ) ) ;
#72467 = CARTESIAN_POINT ( 'NONE',  ( -1.071796769724491005, 10.90759618943233455, 26.00000000000000355 ) ) ;
#72468 = CARTESIAN_POINT ( 'NONE',  ( 27.15937500061451360, 0.000000000000000000, 5.243569643749999010 ) ) ;
#72469 = CARTESIAN_POINT ( 'NONE',  ( 3.440625000614518036, -3.027376345333610441, -5.243569643749999898 ) ) ;
#72470 = CARTESIAN_POINT ( 'NONE',  ( 13.71562500061451750, -6.054752690667223547, -1.112240025338166033E-15 ) ) ;
#72471 = ORIENTED_EDGE ( 'NONE', *, *, #48761, .F. ) ;
#72472 = CARTESIAN_POINT ( 'NONE',  ( 11.27812500061451573, 4.541064518000418104, 2.621784821874999949 ) ) ;
#72473 = VECTOR ( 'NONE', #47949, 1000.000000000000000 ) ;
#72474 = CARTESIAN_POINT ( 'NONE',  ( 9.365625000614519635, 3.027376345333613106, -5.243569643749998122 ) ) ;
#72475 = CARTESIAN_POINT ( 'NONE',  ( 18.34687500061451715, -2.746126346562642428, -4.756430356249999214 ) ) ;
#72476 = CARTESIAN_POINT ( 'NONE',  ( 9.112500000000000711, 2.886751345948129099, -4.999999999999998224 ) ) ;
#72477 = CARTESIAN_POINT ( 'NONE',  ( 1.510657702057710734E-15, 19.43750000000000000, 26.00000000000000000 ) ) ;
#72478 = CARTESIAN_POINT ( 'NONE',  ( 16.80000000000000071, 4.330127018922192761, -2.499999999999997780 ) ) ;
#72479 = CARTESIAN_POINT ( 'NONE',  ( 18.90937500061451360, 4.541064518000418104, -2.621784821874998173 ) ) ;
#72480 = CARTESIAN_POINT ( 'NONE',  ( 12.75000000122903643, -2.886751345948125991, -5.000000000000000000 ) ) ;
#72481 = CARTESIAN_POINT ( 'NONE',  ( 19.76250000000000639, -5.773502691896255534, -1.060575238724906372E-15 ) ) ;
#72482 = CARTESIAN_POINT ( 'NONE',  ( 4.243569643749999898, 16.42812500061451786, -30.00000000000000000 ) ) ;
#72483 = FACE_OUTER_BOUND ( 'NONE', #64479, .T. ) ;
#72484 = CARTESIAN_POINT ( 'NONE',  ( 25.84687500061451360, -4.119189519843965641, -2.378215178125001383 ) ) ;
#72485 = CARTESIAN_POINT ( 'NONE',  ( 14.38125000122903252, -4.330127018922194537, 2.499999999999995559 ) ) ;
#72486 = CARTESIAN_POINT ( 'NONE',  ( 27.06562500061451004, 3.027376345333611329, 5.243569643749999010 ) ) ;
#72487 = CARTESIAN_POINT ( 'NONE',  ( 2.000000000000001332, 19.69999999999999929, 33.46410161513774995 ) ) ;
#72488 = DIRECTION ( 'NONE',  ( 0.000000000000000000, 0.000000000000000000, 1.000000000000000000 ) ) ;
#72489 = CARTESIAN_POINT ( 'NONE',  ( 25.91250000000000142, 2.886751345948126879, 4.999999999999999112 ) ) ;
#72490 = ADVANCED_FACE ( 'NONE', ( #30912 ), #58247, .T. ) ;
#72491 = CARTESIAN_POINT ( 'NONE',  ( 9.815625000614518925, 3.027376345333613106, -5.243569643749998122 ) ) ;
#72492 = CARTESIAN_POINT ( 'NONE',  ( 28.35937500061451644, 2.746126346562643317, 4.756430356249998326 ) ) ;
#72493 = CARTESIAN_POINT ( 'NONE',  ( 21.42187500061451644, -6.054752690667223547, -1.112240025338166033E-15 ) ) ;
#72494 = CARTESIAN_POINT ( 'NONE',  ( 14.29687500061451644, 4.119189519843966529, -2.378215178124998275 ) ) ;
#72495 = EDGE_CURVE ( 'NONE', #41056, #49222, #31282, .T. ) ;
#72496 = CARTESIAN_POINT ( 'NONE',  ( 8.240625000614516082, -3.027376345333614438, 5.243569643749998122 ) ) ;
#72497 = CARTESIAN_POINT ( 'NONE',  ( 9.646875000614516082, -3.027376345333614438, 5.243569643749998122 ) ) ;
#72498 = ORIENTED_EDGE ( 'NONE', *, *, #826, .T. ) ;
#72499 = CARTESIAN_POINT ( 'NONE',  ( 22.47187500061451715, 3.027376345333613106, -5.243569643749998122 ) ) ;
#72500 = CARTESIAN_POINT ( 'NONE',  ( 29.51249999999999929, 2.886751345948126879, 4.999999999999999112 ) ) ;
#72501 = CARTESIAN_POINT ( 'NONE',  ( 4.087500000000001243, -2.886751345948125991, -5.000000000000000000 ) ) ;
#72502 = CARTESIAN_POINT ( 'NONE',  ( 14.55000000122903181, -2.886751345948125991, -5.000000000000000000 ) ) ;
#72503 = FACE_OUTER_BOUND ( 'NONE', #32298, .T. ) ;
#72504 = CARTESIAN_POINT ( 'NONE',  ( 14.40000000122902790, -2.886751345948063374, 5.000000000000112799 ) ) ;
#72505 = ORIENTED_EDGE ( 'NONE', *, *, #50924, .T. ) ;
#72506 = CARTESIAN_POINT ( 'NONE',  ( 13.76250000000000107, 2.886751345948126879, 4.999999999999999112 ) ) ;
#72507 = CARTESIAN_POINT ( 'NONE',  ( 17.69999999999999929, 4.330127018922192761, -2.499999999999997780 ) ) ;
#72508 = EDGE_CURVE ( 'NONE', #8461, #16786, #14286, .T. ) ;
#72509 = CARTESIAN_POINT ( 'NONE',  ( 13.61250000122903359, -4.330127018922190985, -2.500000000000001332 ) ) ;
#72510 = CARTESIAN_POINT ( 'NONE',  ( 12.14062500061451821, 6.054752690667223547, 3.707466751127219781E-16 ) ) ;
#72511 = ORIENTED_EDGE ( 'NONE', *, *, #10210, .T. ) ;
#72512 = CARTESIAN_POINT ( 'NONE',  ( 8.550000000000002487, -4.330127018922190985, -2.500000000000001332 ) ) ;
#72513 = CARTESIAN_POINT ( 'NONE',  ( 26.39999999999999858, 0.000000000000000000, 4.999999999999998224 ) ) ;
#72514 = CARTESIAN_POINT ( 'NONE',  ( 4.243569643749999010, 14.27187500061451964, -32.45002607614398471 ) ) ;
#72515 = CARTESIAN_POINT ( 'NONE',  ( 27.33750000122903145, 4.330127018922191873, 2.499999999999999556 ) ) ;
#72516 = CARTESIAN_POINT ( 'NONE',  ( -7.967954043666661671E-16, 14.32812499938548356, 34.33755215474603517 ) ) ;
#72517 = CARTESIAN_POINT ( 'NONE',  ( 9.674999999999998934, 4.330127018922191873, 2.499999999999999556 ) ) ;
#72518 = DIRECTION ( 'NONE',  ( 0.000000000000000000, 0.000000000000000000, 1.000000000000000000 ) ) ;
#72519 = CIRCLE ( 'NONE', #15868, 1.500000000000000444 ) ;
#72520 = VERTEX_POINT ( 'NONE', #24638 ) ;
#72521 = CARTESIAN_POINT ( 'NONE',  ( 23.80312500061451786, 4.541064518000418104, -2.621784821874998173 ) ) ;
#72522 = CARTESIAN_POINT ( 'NONE',  ( 3.999999999999999112, 13.47500000000000142, -30.00000000000000000 ) ) ;
#72523 = CARTESIAN_POINT ( 'NONE',  ( 45.00000000000000000, 0.000000000000000000, 4.999999999999998224 ) ) ;
#72524 = CARTESIAN_POINT ( 'NONE',  ( 20.74687500061451573, 6.054752690667223547, 3.707466751127219781E-16 ) ) ;
#72525 = EDGE_CURVE ( 'NONE', #14829, #43953, #5236, .T. ) ;
#72526 = CARTESIAN_POINT ( 'NONE',  ( 17.24062500061451786, -3.027376345333614438, 5.243569643749998122 ) ) ;
#72527 = CARTESIAN_POINT ( 'NONE',  ( -3.000416591977282496E-16, 11.59062500061459389, -34.90005215228797653 ) ) ;
#72528 = CARTESIAN_POINT ( 'NONE',  ( 5.503125000614516260, 0.000000000000000000, 5.243569643749999010 ) ) ;
#72529 = CARTESIAN_POINT ( 'NONE',  ( 29.58750000122903501, 4.330127018922191873, 2.499999999999999556 ) ) ;
#72530 = CARTESIAN_POINT ( 'NONE',  ( 24.34687500061451715, 5.492252693125287522, 3.363034840372157021E-16 ) ) ;
#72531 = CARTESIAN_POINT ( 'NONE',  ( 18.10312500061451502, 0.000000000000000000, 5.243569643749999010 ) ) ;
#72532 = CARTESIAN_POINT ( 'NONE',  ( 7.696875000614516793, 5.492252693125287522, 3.363034840372157021E-16 ) ) ;
#72533 = CARTESIAN_POINT ( 'NONE',  ( -3.756430356249999214, 18.67812499938548143, 27.83122392262697531 ) ) ;
#72534 = CARTESIAN_POINT ( 'NONE',  ( 13.99687500061451928, 6.054752690667223547, 3.707466751127219781E-16 ) ) ;
#72535 = CARTESIAN_POINT ( 'NONE',  ( 14.78437500061451715, 6.421520780324663323E-16, -5.243569643749999010 ) ) ;
#72536 = CARTESIAN_POINT ( 'NONE',  ( 22.35937500061451644, -4.541064518000417216, -2.621784821875001281 ) ) ;
#72537 = VERTEX_POINT ( 'NONE', #19822 ) ;
#72538 = CARTESIAN_POINT ( 'NONE',  ( -2.121784821874996840, 12.28437500061451892, 33.67503911421598417 ) ) ;
#72539 = CARTESIAN_POINT ( 'NONE',  ( 3.515625000614516882, 3.027376345333613106, -5.243569643749998122 ) ) ;
#72540 = CARTESIAN_POINT ( 'NONE',  ( 27.14062500061451644, -3.027376345333614438, 5.243569643749998122 ) ) ;
#72541 = CARTESIAN_POINT ( 'NONE',  ( 26.46562500061451573, 3.027376345333613106, -5.243569643749998122 ) ) ;
#72542 = CARTESIAN_POINT ( 'NONE',  ( 17.34375000122903288, 5.773502691896255534, 3.535250795749688401E-16 ) ) ;
#72543 = CARTESIAN_POINT ( 'NONE',  ( -2.828200636599751609E-16, 17.18750000000000000, 25.38119784648299770 ) ) ;
#72544 = CARTESIAN_POINT ( 'NONE',  ( 4.246875000614519280, -3.027376345333614438, 5.243569643749998122 ) ) ;
#72545 = CARTESIAN_POINT ( 'NONE',  ( 12.33750000122903145, 6.123233995736764310E-16, -4.999999999999998224 ) ) ;
#72546 = AXIS2_PLACEMENT_3D ( 'NONE', #38509, #43689, #33325 ) ;
#72547 = CARTESIAN_POINT ( 'NONE',  ( 9.450000001229033941, -2.886751345948129988, 4.999999999999997335 ) ) ;
#72548 = CARTESIAN_POINT ( 'NONE',  ( 3.740625000614516527, -3.027376345333614438, 5.243569643749998122 ) ) ;
#72549 = CARTESIAN_POINT ( 'NONE',  ( -2.000000000000001776, 18.14374999877096428, 33.46410161513775705 ) ) ;
#72550 = CARTESIAN_POINT ( 'NONE',  ( 19.29375000122903216, -2.886751345948129988, 4.999999999999997335 ) ) ;
#72551 = CARTESIAN_POINT ( 'NONE',  ( 12.19687500061451679, 6.054752690667223547, 3.707466751127219781E-16 ) ) ;
#72552 = CARTESIAN_POINT ( 'NONE',  ( 26.51250000122903216, 0.000000000000000000, 4.999999999999998224 ) ) ;
#72553 = ORIENTED_EDGE ( 'NONE', *, *, #41935, .F. ) ;
#72554 = CARTESIAN_POINT ( 'NONE',  ( 20.69062500061451715, 6.054752690667223547, 3.707466751127219781E-16 ) ) ;
#72555 = CARTESIAN_POINT ( 'NONE',  ( 14.10937500061451644, 0.000000000000000000, 5.243569643749999010 ) ) ;
#72556 = CARTESIAN_POINT ( 'NONE',  ( 5.578125000614518214, -4.541064518000419881, 2.621784821874995952 ) ) ;
#72557 = CARTESIAN_POINT ( 'NONE',  ( 21.19687500061451502, 6.054752690667223547, 3.707466751127219781E-16 ) ) ;
#72558 = CARTESIAN_POINT ( 'NONE',  ( 4.678125000614516971, -4.541064518000419881, 2.621784821874995952 ) ) ;
#72559 = DIRECTION ( 'NONE',  ( -0.000000000000000000, -1.000000000000000000, -0.000000000000000000 ) ) ;
#72560 =( BOUNDED_SURFACE ( )  B_SPLINE_SURFACE ( 1, 2, ( 
 ( #14503, #54768, #20405, #49598, #9701, #66214, #37771, #43329, #10433, #32963, #4539, #31506, #25595, #15233, #54046, #32234, #3064, #48867, #32602, #42587, #8974, #55140, #4173, #65113, #25961, #27066, #48133, #66584, #72124, #71027, #26703, #71769, #49236, #21505, #14871, #44058, #15961, #70657, #38511, #20031, #37410, #59932, #9340, #31872, #3807, #26329, #71398, #39608, #55866, #17762, #62129, #27797, #44795, #72858, #50334, #33686, #45147, #443, #90, #56582, #16328, #34406, #22597, #66962, #28509, #811, #55500, #5979, #44434, #38882, #28869, #12237, #39970, #72486, #68043, #6339, #17413, #22952, #40322, #39244, #67680, #56934, #51048, #33328, #11521, #17051, #45513, #62484, #61399, #10793, #34043, #67329, #5255, #11882, #51408, #11161, #23318, #45868, #68401, #5624, #62844, #4896, #28160, #27430, #22241, #49962, #21872, #16688, #61758, #56230, #50688, #41766, #64295, #13682, #40689, #41057, #8153, #30324, #52854, #58015, #1534, #19581, #18124, #47671, #23680, #24041, #46227, #19211, #42137, #1171, #52491, #64663, #34768, #46591, #69845, #24768, #57301, #35495, #18851, #68766, #29594, #63207, #41412, #12602, #69133, #1902, #69492, #35135, #18492, #57660, #6706, #36226, #70206, #29239, #58742, #30680, #63570, #25130, #7066, #63928, #51772, #52131, #12958, #24406, #7423, #29951, #46956, #13313, #35852, #58375, #7787, #53212, #2253, #47311, #2608, #4083, #9616, #70576, #38045, #8886, #65027, #3356, #32147, #26613, #14418, #37324, #70944, #43971, #4452, #42869, #54680, #42504, #9252, #8515, #20315, #21414, #59847, #59474, #49150, #21053, #43604, #31044, #71679, #65762, #53582, #14048, #31419, #36953, #43242, #72038, #19951, #26244, #53959, #25878, #2978, #48417, #36588, #65391, #66125, #15504, #9977, #14782, #60570, #25506, #32514, #48781, #3717, #31787, #54326, #55051, #71306, #59109, #48051, #20683, #15144, #37681, #26981, #60204, #49510, #49872, #57485, #50244, #67239, #40511, #72397, #27703, #33239, #44342, #32875, #3, #33594, #39150, #1355, #18307, #60941, #72766, #16239, #1714, #46412, #29776, #24227, #68949, #29421, #22151, #57838, #66870, #28070, #66491, #52312, #10345, #56139, #16597, #44704, #7247, #61668, #4809, #21778, #38794, #40879, #50599, #55776, #61311, #6889, #63026, #10706, #63394, #5168, #11067, #5533, #12425, #51955, #22510, #46053, #68587, #15872, #38419, #17949, #34958, #23864, #12779, #55414, #35316, #27341, #19396, #19033, #42321, #53772, #3168, #63747, #64846, #25319, #13136, #3535, #41591, #47136, #2793, #31604, #52671, #58925, #2079, #64109, #35675, #13494, #46777, #36042, #14234, #36772, #42685, #69667, #59289, #58198, #31230, #8333, #36411, #41957, #58563, #8698, #7970, #54141, #7601, #30863, #64478, #69312, #65207, #24588, #25695, #30140, #48231, #30506, #47494, #19770, #53033, #2428, #24951, #70025, #13871, #53401, #47865, #70394, #70755, #20130, #41235, #14597, #18673, #37132, #59661, #9069, #10891, #37869, #61134, #16062, #26058, #26798, #10168, #14967, #20873, #37505, #32702, #60025, #60388, #43788, #60760, #54502, #3904, #55239, #48598, #71864, #10531, #65577, #31965, #44159, #66315, #9437, #26426, #4993, #71123, #16420, #21971, #48966, #4634, #21604, #27164, #15692, #43426, #66687, #27525, #20495, #38611, #49698, #72225, #50059, #33059, #9796, #55598, #15327, #4274, #72588, #71496, #61494, #44530, #65948, #32329, #54866, #49332, #21236, #38231, #67063, #38978, #33419, #55960, #43051, #45609, #16784, #51509, #23773, #5355, #6437, #67422, #39342, #51864, #35231, #62937, #22335, #17861, #29334, #40420, #45964, #63302, #62226, #23054, #6800, #909, #56327, #62582, #68143, #68497, #12331, #61855, #11262, #11979, #67776, #33784, #34866, #17507, #34138, #57393, #34502, #40068, #28608, #12694, #57030, #51144, #28971, #5716, #23417, #1266, #46325, #40789, #27893, #68860, #18216, #50427, #72953, #28252, #11622, #44887, #50783, #186, #544, #45242, #22691, #17150, #39708, #56677, #6075, #69226, #41152, #18587, #36323, #1993, #31140, #41861, #2708, #19308, #24861, #42597, #65123, #59203, #13051, #7160, #47408, #64757, #63660, #64023, #53681, #53309, #25224, #7883, #24504, #14513, #35590, #70666, #46688, #47048, #58109, #7516, #30047, #58838, #69582, #3076, #64391, #47770, #13781, #69938, #57752, #29689, #8611, #52587, #52226, #8248, #18944, #30778, #1630, #30419, #42232, #24137, #41503, #70306, #2344, #13402, #35950, #36682, #58470, #48142, #25604, #52947, #19679, #14147, #20042, #54777, #54416, #55149, #15971, #31516, #27076, #60667, #43702, #61044, #21514, #20782, #21148, #26338, #15242, #66223, #37419, #72496, #15602, #9349, #48877, #3817, #31882, #37779, #26711, #4547, #4183, #38143, #71038, #38521, #49245, #48511, #10081, #55512, #37046, #32611, #25970, #20413, #10442, #66970, #44068, #54057, #49607, #32972, #72134, #66595, #21881, #43338, #71780, #4905, #27441, #14880, #49971, #44441, #59571, #8984, #42961, #65490, #3452, #71407, #59942, #65860, #60299, #9710, #32244, #452, #51057, #39619, #23687, #45522, #62137, #68052, #22249, #5987, #56591, #28517, #51779, #16335, #22961, #23327, #45877, #67688, #17421, #16696, #1179, #39980, #61766, #5632, #33694, #11170, #17059, #62492, #34415, #34051, #11890, #50342, #68409, #56943, #27808, #6347, #34777, #38890, #28878, #5262, #72866, #62852, #46235, #819, #33337, #51418, #40331, #17771, #12246, #61408, #98, #57310, #6714, #29247, #67336, #10802, #55875, #44803, #39254, #56241, #28169, #50696, #22604, #45156, #11531, #7797, #24415, #30690, #52863, #30335, #18860, #2986, #24777, #41421, #47321, #1542, #58384, #35861, #2263, #31054, #68775, #69854, #2618, #25139, #47680, #24052, #1911, #42146, #64304, #13694, #63937, #35504, #53591, #52139, #8525, #57668, #58023, #7074, #46599 ),
 ( #19221, #7433, #63579, #58751, #36237, #69141, #19590, #12966, #18500, #29959, #8161, #53221, #41065, #13322, #52500, #25514, #59118, #46964, #70216, #69500, #41775, #63216, #64673, #18131, #14058, #36597, #40698, #12611, #35145, #29603, #65772, #65401, #66138, #26994, #42512, #38058, #71693, #54693, #72048, #32526, #31796, #32160, #37334, #26253, #4096, #48427, #10357, #26625, #20324, #59857, #14792, #42878, #48790, #37691, #15516, #15154, #49162, #8896, #49523, #60214, #59484, #21065, #66504, #48059, #43616, #36962, #31428, #21426, #4819, #55063, #65036, #60583, #43983, #9991, #4464, #32887, #54334, #9627, #15886, #38431, #25887, #60955, #55427, #70584, #19960, #53968, #3366, #14427, #9261, #70953, #3728, #71317, #20693, #43252, #11448, #62053, #50611, #34691, #56507, #15, #5900, #33251, #16971, #67606, #39527, #62772, #27353, #33968, #34326, #56858, #6264, #55789, #33607, #735, #22873, #45431, #22522, #67251, #12163, #10719, #40251, #16250, #16609, #38806, #5179, #61321, #28433, #44715, #23244, #50970, #67965, #366, #17338, #57222, #49884, #28792, #27716, #72409, #39897, #39165, #21791, #45795, #11079, #11809, #66883, #50256, #62410, #45069, #72780, #22163, #51333, #44357, #17690, #68330, #61680, #56151, #5545, #28083, #8077, #2180, #57588, #63850, #24331, #47237, #41692, #40611, #18053, #13241, #69054, #63132, #64215, #18774, #35418, #13604, #35779, #41340, #29880, #13974, #58302, #52416, #7711, #12528, #69419, #46880, #30245, #42063, #6635, #52778, #36150, #58669, #30609, #35061, #12885, #53137, #24693, #69770, #1824, #46515, #64586, #6991, #19506, #68693, #18416, #29522, #52057, #1461, #19138, #23967, #2536, #25056, #47599, #70128, #36512, #29164, #51696, #1100, #40982, #23608, #46153, #63497, #57943, #7350, #42790, #43529, #25428, #64950, #4010, #3640, #47971, #14342, #37973, #59032, #49433, #54972, #42429, #65683, #54605, #20604, #26164, #3273, #26533, #60494, #53505, #49073, #9539, #15071, #9900, #66051, #65311, #43163, #48339, #37245, #37608, #59394, #21341, #60130, #31340, #70864, #25801, #53881, #59766, #48703, #71601, #71226, #32073, #19876, #32436, #20976, #70499, #15429, #4378, #8434, #26907, #36876, #8804, #71967, #15798, #43896, #2897, #66420, #30970, #20238, #14701, #9173, #31708, #54243, #284, #72326, #49801, #22436, #27631, #21706, #22792, #50526, #67164, #45345, #44984, #73054, #61594, #45711, #67521, #10995, #16886, #44263, #27997, #5457, #39440, #649, #38338, #61960, #67879, #17251, #39811, #66796, #44635, #11723, #33882, #56427, #33515, #5095, #23157, #16167, #51246, #27268, #50164, #38719, #61239, #10633, #11364, #55701, #34239, #5816, #28347, #50884, #62327, #68245, #60867, #56773, #33163, #10270, #6178, #72694, #32803, #28707, #22076, #55339, #4734, #16525, #39077, #56064, #57134, #46069, #69686, #17608, #7989, #13514, #1013, #24245, #13153, #52330, #35333, #34974, #35695, #19051, #12083, #7620, #41253, #46794, #41609, #2096, #1372, #1732, #6905, #68968, #69331, #17965, #53052, #18689, #63042, #29436, #57503, #12442, #18324, #7265, #58215, #57856, #63765, #51612, #64128, #29794, #29077, #30156, #36061, #40168, #52690, #6543, #23519, #58582, #47514, #24607, #34604, #47154, #30525, #2446, #24969, #62687, #23882, #68604, #40526, #46429, #51973, #40898, #63411, #12797, #15615, #36429, #25340, #49984, #70043, #61422, #66984, #53422, #4561, #66609, #32624, #38157, #14252, #15984, #72509, #64497, #61057, #21526, #27089, #21897, #55525, #53790, #55164, #59306, #48251, #49621, #70414, #33350, #72148, #42341, #8717, #36791, #64864, #70774, #60680, #38534, #10094, #44082, #30880, #44454, #10456, #8351, #32985, #16348, #19416, #4919, #58943, #2812, #38903, #27822, #27454, #13889, #10816, #55888, #5276, #41976, #47885, #3186, #19790, #31249, #25713, #20150, #42704, #65226, #17785, #12261, #11184, #61780, #34429, #39633, #33709, #34791, #62506, #6001, #57324, #56958, #11905, #468, #57683, #6361, #22976, #28893, #56256, #39993, #17435, #51432, #12624, #50354, #834, #6728, #29262, #51792, #5646, #56605, #23701, #45891, #68423, #45538, #17073, #35159, #28182, #63230, #39268, #62151, #50710, #114, #22619, #23343, #67701, #46249, #40345, #62865, #1193, #68790, #7088, #72881, #18146, #45170, #22263, #40713, #11548, #44816, #67350, #16712, #34064, #28534, #51070, #68067, #2632, #24791, #52876, #35874, #58037, #8174, #7447, #8539, #46612, #2274, #58398, #31067, #64686, #12982, #36250, #63593, #30702, #69514, #63951, #13707, #41080, #46978, #1924, #35518, #69155, #69867, #30348, #7812, #25153, #19603, #24067, #53235, #53605, #18514, #47334, #29617, #52153, #18873, #47693, #70229, #1556, #58764, #42159, #41435, #19233, #13336, #14071, #41787, #64317, #36610, #59131, #29973, #52515, #24429, #29859, #1438, #57921, #52395, #23944, #57565, #51308, #12864, #22852, #57197, #22500, #7328, #39503, #62750, #23219, #67942, #16950, #50948, #39875, #28411, #346, #46493, #6612, #62387, #17315, #12509, #18033, #5879, #69032, #11786, #45407, #34303, #40589, #35037, #56834, #45772, #6242, #45049, #35395, #712, #63110, #28769, #17667, #62027, #68308, #67584, #40228, #12143, #6968, #29499, #52035, #11426, #18394, #1078, #33943, #56486, #34669, #29140, #51673, #23586, #46131, #68669, #40961, #63476, #63828, #41672, #31686, #19117, #42407, #37221, #8414, #47217, #64195, #13582, #69749, #53115, #64565, #19856, #19484, #2877, #35759, #53860, #42042, #13220, #47951, #20215, #1802, #25408, #58280, #7687, #48317, #24312, #59371, #18754, #14320, #25779, #36855, #64929, #59743, #58647, #13953, #3251, #70479, #52757, #59011, #36491, #8782, #31316, #30224, #2160, #30944, #36128, #24671, #70840, #53485, #30590, #42769, #65289, #14677, #25035, #9151, #46860, #47578, #69399, #8055 ) ),
 .UNSPECIFIED., .F., .F., .F. ) 
 B_SPLINE_SURFACE_WITH_KNOTS ( ( 2, 2 ),
 ( 3, 2, 2, 2, 2, 2, 2, 2, 2, 2, 2, 2, 2, 2, 2, 2, 2, 2, 2, 2, 2, 2, 2, 2, 2, 2, 2, 2, 2, 2, 2, 2, 2, 2, 2, 2, 2, 2, 2, 2, 2, 2, 2, 2, 2, 2, 2, 2, 2, 2, 2, 2, 2, 2, 2, 2, 2, 2, 2, 2, 2, 2, 2, 2, 2, 2, 2, 2, 2, 2, 2, 2, 2, 2, 2, 2, 2, 2, 2, 2, 2, 2, 2, 2, 2, 2, 2, 2, 2, 2, 2, 2, 2, 2, 2, 2, 2, 2, 2, 2, 2, 2, 2, 2, 2, 2, 2, 2, 2, 2, 2, 2, 2, 2, 2, 2, 2, 2, 2, 2, 2, 2, 2, 2, 2, 2, 2, 2, 2, 2, 2, 2, 2, 2, 2, 2, 2, 2, 2, 2, 2, 2, 2, 2, 2, 2, 2, 2, 2, 2, 2, 2, 2, 2, 2, 2, 2, 2, 2, 2, 2, 2, 2, 2, 2, 2, 2, 2, 2, 2, 2, 2, 2, 2, 2, 2, 2, 2, 2, 2, 2, 2, 2, 2, 2, 2, 2, 2, 2, 2, 2, 2, 2, 2, 2, 2, 2, 2, 2, 2, 2, 2, 2, 2, 2, 2, 2, 2, 2, 2, 2, 2, 2, 2, 2, 2, 2, 2, 2, 2, 2, 2, 2, 2, 2, 2, 2, 2, 2, 2, 2, 2, 2, 2, 2, 2, 2, 2, 2, 2, 2, 2, 2, 2, 2, 2, 2, 2, 2, 2, 2, 2, 2, 2, 2, 2, 2, 2, 2, 2, 2, 2, 2, 2, 2, 2, 2, 2, 2, 2, 2, 2, 2, 2, 2, 2, 2, 2, 2, 2, 2, 2, 2, 2, 2, 2, 2, 2, 2, 2, 2, 2, 2, 2, 2, 2, 2, 2, 2, 2, 2, 2, 2, 2, 2, 2, 2, 2, 2, 2, 2, 2, 2, 2, 2, 2, 2, 2, 2, 2, 2, 2, 2, 2, 2, 2, 2, 2, 2, 2, 2, 2, 2, 2, 2, 2, 2, 2, 2, 2, 2, 2, 2, 2, 2, 2, 2, 2, 2, 2, 2, 2, 2, 2, 2, 2, 2, 2, 2, 2, 3 ),
 ( 0.000000000000000000, 1.000000000000000000 ),
 ( 0.000000000000000000, 0.002777777777777777884, 0.005555555555555555768, 0.008333333333333333218, 0.01111111111111111154, 0.01388888888888888812, 0.01666666666666666644, 0.01944444444444444475, 0.02222222222222222307, 0.02500000000000000139, 0.02777777777777777624, 0.03055555555555555455, 0.03333333333333333287, 0.03611111111111110772, 0.03888888888888888951, 0.04166666666666666435, 0.04444444444444444614, 0.04722222222222222099, 0.05000000000000000278, 0.05277777777777777762, 0.05555555555555555247, 0.05833333333333333426, 0.06111111111111110911, 0.06388888888888888395, 0.06666666666666666574, 0.06944444444444444753, 0.07222222222222221544, 0.07499999999999999722, 0.07777777777777777901, 0.08055555555555556080, 0.08333333333333332871, 0.08611111111111111049, 0.08888888888888889228, 0.09166666666666666019, 0.09444444444444444198, 0.09722222222222222376, 0.1000000000000000056, 0.1027777777777777735, 0.1055555555555555552, 0.1083333333333333370, 0.1111111111111111049, 0.1138888888888888867, 0.1166666666666666685, 0.1194444444444444503, 0.1222222222222222182, 0.1250000000000000000, 0.1277777777777777679, 0.1305555555555555636, 0.1333333333333333315, 0.1361111111111110994, 0.1388888888888888951, 0.1416666666666666630, 0.1444444444444444309, 0.1472222222222222265, 0.1499999999999999944, 0.1527777777777777901, 0.1555555555555555580, 0.1583333333333333259, 0.1611111111111111216, 0.1638888888888888895, 0.1666666666666666574, 0.1694444444444444531, 0.1722222222222222210, 0.1749999999999999889, 0.1777777777777777846, 0.1805555555555555525, 0.1833333333333333204, 0.1861111111111111160, 0.1888888888888888840, 0.1916666666666666796, 0.1944444444444444475, 0.1972222222222222154, 0.2000000000000000111, 0.2027777777777777790, 0.2055555555555555469, 0.2083333333333333426, 0.2111111111111111105, 0.2138888888888888784, 0.2166666666666666741, 0.2194444444444444420, 0.2222222222222222099, 0.2250000000000000056, 0.2277777777777777735, 0.2305555555555555691, 0.2333333333333333370, 0.2361111111111111049, 0.2388888888888889006, 0.2416666666666666685, 0.2444444444444444364, 0.2472222222222222321, 0.2500000000000000000, 0.2527777777777777679, 0.2555555555555555358, 0.2583333333333333592, 0.2611111111111111271, 0.2638888888888888951, 0.2666666666666666630, 0.2694444444444444309, 0.2722222222222221988, 0.2750000000000000222, 0.2777777777777777901, 0.2805555555555555580, 0.2833333333333333259, 0.2861111111111110938, 0.2888888888888888618, 0.2916666666666666852, 0.2944444444444444531, 0.2972222222222222210, 0.2999999999999999889, 0.3027777777777777568, 0.3055555555555555802, 0.3083333333333333481, 0.3111111111111111160, 0.3138888888888888840, 0.3166666666666666519, 0.3194444444444444198, 0.3222222222222222432, 0.3250000000000000111, 0.3277777777777777790, 0.3305555555555555469, 0.3333333333333333148, 0.3361111111111111382, 0.3388888888888889062, 0.3416666666666666741, 0.3444444444444444420, 0.3472222222222222099, 0.3499999999999999778, 0.3527777777777778012, 0.3555555555555555691, 0.3583333333333333370, 0.3611111111111111049, 0.3638888888888888729, 0.3666666666666666408, 0.3694444444444444642, 0.3722222222222222321, 0.3750000000000000000, 0.3777777777777777679, 0.3805555555555555358, 0.3833333333333333592, 0.3861111111111111271, 0.3888888888888888951, 0.3916666666666666630, 0.3944444444444444309, 0.3972222222222221988, 0.4000000000000000222, 0.4027777777777777901, 0.4055555555555555580, 0.4083333333333333259, 0.4111111111111110938, 0.4138888888888888618, 0.4166666666666666852, 0.4194444444444444531, 0.4222222222222222210, 0.4249999999999999889, 0.4277777777777777568, 0.4305555555555555802, 0.4333333333333333481, 0.4361111111111111160, 0.4388888888888888840, 0.4416666666666666519, 0.4444444444444444198, 0.4472222222222222432, 0.4500000000000000111, 0.4527777777777777790, 0.4555555555555555469, 0.4583333333333333148, 0.4611111111111111382, 0.4638888888888889062, 0.4666666666666666741, 0.4694444444444444420, 0.4722222222222222099, 0.4749999999999999778, 0.4777777777777778012, 0.4805555555555555691, 0.4833333333333333370, 0.4861111111111111049, 0.4888888888888888729, 0.4916666666666666408, 0.4944444444444444642, 0.4972222222222222321, 0.5000000000000000000, 0.5027777777777777679, 0.5055555555555555358, 0.5083333333333333037, 0.5111111111111110716, 0.5138888888888888395, 0.5166666666666667185, 0.5194444444444444864, 0.5222222222222222543, 0.5250000000000000222, 0.5277777777777777901, 0.5305555555555555580, 0.5333333333333333259, 0.5361111111111110938, 0.5388888888888888618, 0.5416666666666666297, 0.5444444444444443976, 0.5472222222222222765, 0.5500000000000000444, 0.5527777777777778123, 0.5555555555555555802, 0.5583333333333333481, 0.5611111111111111160, 0.5638888888888888840, 0.5666666666666666519, 0.5694444444444444198, 0.5722222222222221877, 0.5749999999999999556, 0.5777777777777777235, 0.5805555555555556024, 0.5833333333333333703, 0.5861111111111111382, 0.5888888888888889062, 0.5916666666666666741, 0.5944444444444444420, 0.5972222222222222099, 0.5999999999999999778, 0.6027777777777777457, 0.6055555555555555136, 0.6083333333333332815, 0.6111111111111111605, 0.6138888888888889284, 0.6166666666666666963, 0.6194444444444444642, 0.6222222222222222321, 0.6250000000000000000, 0.6277777777777777679, 0.6305555555555555358, 0.6333333333333333037, 0.6361111111111110716, 0.6388888888888888395, 0.6416666666666667185, 0.6444444444444444864, 0.6472222222222222543, 0.6500000000000000222, 0.6527777777777777901, 0.6555555555555555580, 0.6583333333333333259, 0.6611111111111110938, 0.6638888888888888618, 0.6666666666666666297, 0.6694444444444443976, 0.6722222222222222765, 0.6750000000000000444, 0.6777777777777778123, 0.6805555555555555802, 0.6833333333333333481, 0.6861111111111111160, 0.6888888888888888840, 0.6916666666666666519, 0.6944444444444444198, 0.6972222222222221877, 0.6999999999999999556, 0.7027777777777777235, 0.7055555555555556024, 0.7083333333333333703, 0.7111111111111111382, 0.7138888888888889062, 0.7166666666666666741, 0.7194444444444444420, 0.7222222222222222099, 0.7249999999999999778, 0.7277777777777777457, 0.7305555555555555136, 0.7333333333333332815, 0.7361111111111111605, 0.7388888888888889284, 0.7416666666666666963, 0.7444444444444444642, 0.7472222222222222321, 0.7500000000000000000, 0.7527777777777777679, 0.7555555555555555358, 0.7583333333333333037, 0.7611111111111110716, 0.7638888888888888395, 0.7666666666666667185, 0.7694444444444444864, 0.7722222222222222543, 0.7750000000000000222, 0.7777777777777777901, 0.7805555555555555580, 0.7833333333333333259, 0.7861111111111110938, 0.7888888888888888618, 0.7916666666666666297, 0.7944444444444443976, 0.7972222222222222765, 0.8000000000000000444, 0.8027777777777778123, 0.8055555555555555802, 0.8083333333333333481, 0.8111111111111111160, 0.8138888888888888840, 0.8166666666666666519, 0.8194444444444444198, 0.8222222222222221877, 0.8249999999999999556, 0.8277777777777777235, 0.8305555555555556024, 0.8333333333333333703, 0.8361111111111111382, 0.8388888888888889062, 0.8416666666666666741, 0.8444444444444444420, 0.8472222222222222099, 0.8499999999999999778, 0.8527777777777777457, 0.8555555555555555136, 0.8583333333333332815, 0.8611111111111111605, 0.8638888888888889284, 0.8666666666666666963, 0.8694444444444444642, 0.8722222222222222321, 0.8750000000000000000, 0.8777777777777777679, 0.8805555555555555358, 0.8833333333333333037, 0.8861111111111110716, 0.8888888888888888395, 0.8916666666666667185, 0.8944444444444444864, 0.8972222222222222543, 0.9000000000000000222, 0.9027777777777777901, 0.9055555555555555580, 0.9083333333333333259, 0.9111111111111110938, 0.9138888888888888618, 0.9166666666666666297, 0.9194444444444443976, 0.9222222222222222765, 0.9250000000000000444, 0.9277777777777778123, 0.9305555555555555802, 0.9333333333333333481, 0.9361111111111111160, 0.9388888888888888840, 0.9416666666666666519, 0.9444444444444444198, 0.9472222222222221877, 0.9499999999999999556, 0.9527777777777777235, 0.9555555555555556024, 0.9583333333333333703, 0.9611111111111111382, 0.9638888888888889062, 0.9666666666666666741, 0.9694444444444444420, 0.9722222222222222099, 0.9749999999999999778, 0.9777777777777777457, 0.9805555555555555136, 0.9833333333333332815, 0.9861111111111111605, 0.9888888888888889284, 0.9916666666666666963, 0.9944444444444444642, 0.9972222222222222321, 1.000000000000000000 ),
 .UNSPECIFIED. ) 
 GEOMETRIC_REPRESENTATION_ITEM ( )  RATIONAL_B_SPLINE_SURFACE ( (
 ( 1.000000000000000000, 0.8660254037844387076, 1.000000000000000000, 0.8660254037844387076, 1.000000000000000000, 0.8660254037844387076, 1.000000000000000000, 0.8660254037844387076, 1.000000000000000000, 0.8660254037844387076, 1.000000000000000000, 0.8660254037844387076, 1.000000000000000000, 0.8660254037844387076, 1.000000000000000000, 0.8660254037844387076, 1.000000000000000000, 0.8660254037844387076, 1.000000000000000000, 0.8660254037844387076, 1.000000000000000000, 0.8660254037844387076, 1.000000000000000000, 0.8660254037844387076, 1.000000000000000000, 0.8660254037844387076, 1.000000000000000000, 0.8660254037844387076, 1.000000000000000000, 0.8660254037844387076, 1.000000000000000000, 0.8660254037844387076, 1.000000000000000000, 0.8660254037844387076, 1.000000000000000000, 0.8660254037844387076, 1.000000000000000000, 0.8660254037844387076, 1.000000000000000000, 0.8660254037844387076, 1.000000000000000000, 0.8660254037844387076, 1.000000000000000000, 0.8660254037844387076, 1.000000000000000000, 0.8660254037844387076, 1.000000000000000000, 0.8660254037844387076, 1.000000000000000000, 0.8660254037844387076, 1.000000000000000000, 0.8660254037844387076, 1.000000000000000000, 0.8660254037844387076, 1.000000000000000000, 0.8660254037844387076, 1.000000000000000000, 0.8660254037844387076, 1.000000000000000000, 0.8660254037844387076, 1.000000000000000000, 0.8660254037844387076, 1.000000000000000000, 0.8660254037844387076, 1.000000000000000000, 0.8660254037844387076, 1.000000000000000000, 0.8660254037844387076, 1.000000000000000000, 0.8660254037844387076, 1.000000000000000000, 0.8660254037844387076, 1.000000000000000000, 0.8660254037844387076, 1.000000000000000000, 0.8660254037844387076, 1.000000000000000000, 0.8660254037844387076, 1.000000000000000000, 0.8660254037844387076, 1.000000000000000000, 0.8660254037844387076, 1.000000000000000000, 0.8660254037844387076, 1.000000000000000000, 0.8660254037844387076, 1.000000000000000000, 0.8660254037844387076, 1.000000000000000000, 0.8660254037844387076, 1.000000000000000000, 0.8660254037844387076, 1.000000000000000000, 0.8660254037844387076, 1.000000000000000000, 0.8660254037844387076, 1.000000000000000000, 0.8660254037844387076, 1.000000000000000000, 0.8660254037844387076, 1.000000000000000000, 0.8660254037844387076, 1.000000000000000000, 0.8660254037844387076, 1.000000000000000000, 0.8660254037844387076, 1.000000000000000000, 0.8660254037844387076, 1.000000000000000000, 0.8660254037844387076, 1.000000000000000000, 0.8660254037844387076, 1.000000000000000000, 0.8660254037844387076, 1.000000000000000000, 0.8660254037844387076, 1.000000000000000000, 0.8660254037844387076, 1.000000000000000000, 0.8660254037844387076, 1.000000000000000000, 0.8660254037844387076, 1.000000000000000000, 0.8660254037844387076, 1.000000000000000000, 0.8660254037844387076, 1.000000000000000000, 0.8660254037844387076, 1.000000000000000000, 0.8660254037844387076, 1.000000000000000000, 0.8660254037844387076, 1.000000000000000000, 0.8660254037844387076, 1.000000000000000000, 0.8660254037844387076, 1.000000000000000000, 0.8660254037844387076, 1.000000000000000000, 0.8660254037844387076, 1.000000000000000000, 0.8660254037844387076, 1.000000000000000000, 0.8660254037844387076, 1.000000000000000000, 0.8660254037844387076, 1.000000000000000000, 0.8660254037844387076, 1.000000000000000000, 0.8660254037844387076, 1.000000000000000000, 0.8660254037844387076, 1.000000000000000000, 0.8660254037844387076, 1.000000000000000000, 0.8660254037844387076, 1.000000000000000000, 0.8660254037844387076, 1.000000000000000000, 0.8660254037844387076, 1.000000000000000000, 0.8660254037844387076, 1.000000000000000000, 0.8660254037844387076, 1.000000000000000000, 0.8660254037844387076, 1.000000000000000000, 0.8660254037844387076, 1.000000000000000000, 0.8660254037844387076, 1.000000000000000000, 0.8660254037844387076, 1.000000000000000000, 0.8660254037844387076, 1.000000000000000000, 0.8660254037844387076, 1.000000000000000000, 0.8660254037844387076, 1.000000000000000000, 0.8660254037844387076, 1.000000000000000000, 0.8660254037844387076, 1.000000000000000000, 0.8660254037844387076, 1.000000000000000000, 0.8660254037844387076, 1.000000000000000000, 0.8660254037844387076, 1.000000000000000000, 0.8660254037844387076, 1.000000000000000000, 0.8660254037844387076, 1.000000000000000000, 0.8660254037844387076, 1.000000000000000000, 0.8660254037844387076, 1.000000000000000000, 0.8660254037844387076, 1.000000000000000000, 0.8660254037844387076, 1.000000000000000000, 0.8660254037844387076, 1.000000000000000000, 0.8660254037844387076, 1.000000000000000000, 0.8660254037844387076, 1.000000000000000000, 0.8660254037844387076, 1.000000000000000000, 0.8660254037844387076, 1.000000000000000000, 0.8660254037844387076, 1.000000000000000000, 0.8660254037844387076, 1.000000000000000000, 0.8660254037844387076, 1.000000000000000000, 0.8660254037844387076, 1.000000000000000000, 0.8660254037844387076, 1.000000000000000000, 0.8660254037844387076, 1.000000000000000000, 0.8660254037844387076, 1.000000000000000000, 0.8660254037844387076, 1.000000000000000000, 0.8660254037844387076, 1.000000000000000000, 0.8660254037844387076, 1.000000000000000000, 0.8660254037844387076, 1.000000000000000000, 0.8660254037844387076, 1.000000000000000000, 0.8660254037844387076, 1.000000000000000000, 0.8660254037844387076, 1.000000000000000000, 0.8660254037844387076, 1.000000000000000000, 0.8660254037844387076, 1.000000000000000000, 0.8660254037844387076, 1.000000000000000000, 0.8660254037844387076, 1.000000000000000000, 0.8660254037844387076, 1.000000000000000000, 0.8660254037844387076, 1.000000000000000000, 0.8660254037844387076, 1.000000000000000000, 0.8660254037844387076, 1.000000000000000000, 0.8660254037844387076, 1.000000000000000000, 0.8660254037844387076, 1.000000000000000000, 0.8660254037844387076, 1.000000000000000000, 0.8660254037844387076, 1.000000000000000000, 0.8660254037844387076, 1.000000000000000000, 0.8660254037844387076, 1.000000000000000000, 0.8660254037844387076, 1.000000000000000000, 0.8660254037844387076, 1.000000000000000000, 0.8660254037844387076, 1.000000000000000000, 0.8660254037844387076, 1.000000000000000000, 0.8660254037844387076, 1.000000000000000000, 0.8660254037844387076, 1.000000000000000000, 0.8660254037844387076, 1.000000000000000000, 0.8660254037844387076, 1.000000000000000000, 0.8660254037844387076, 1.000000000000000000, 0.8660254037844387076, 1.000000000000000000, 0.8660254037844387076, 1.000000000000000000, 0.8660254037844387076, 1.000000000000000000, 0.8660254037844387076, 1.000000000000000000, 0.8660254037844387076, 1.000000000000000000, 0.8660254037844387076, 1.000000000000000000, 0.8660254037844387076, 1.000000000000000000, 0.8660254037844387076, 1.000000000000000000, 0.8660254037844387076, 1.000000000000000000, 0.8660254037844387076, 1.000000000000000000, 0.8660254037844387076, 1.000000000000000000, 0.8660254037844387076, 1.000000000000000000, 0.8660254037844387076, 1.000000000000000000, 0.8660254037844387076, 1.000000000000000000, 0.8660254037844387076, 1.000000000000000000, 0.8660254037844387076, 1.000000000000000000, 0.8660254037844387076, 1.000000000000000000, 0.8660254037844387076, 1.000000000000000000, 0.8660254037844387076, 1.000000000000000000, 0.8660254037844387076, 1.000000000000000000, 0.8660254037844387076, 1.000000000000000000, 0.8660254037844387076, 1.000000000000000000, 0.8660254037844387076, 1.000000000000000000, 0.8660254037844387076, 1.000000000000000000, 0.8660254037844387076, 1.000000000000000000, 0.8660254037844387076, 1.000000000000000000, 0.8660254037844387076, 1.000000000000000000, 0.8660254037844387076, 1.000000000000000000, 0.8660254037844387076, 1.000000000000000000, 0.8660254037844387076, 1.000000000000000000, 0.8660254037844387076, 1.000000000000000000, 0.8660254037844387076, 1.000000000000000000, 0.8660254037844387076, 1.000000000000000000, 0.8660254037844387076, 1.000000000000000000, 0.8660254037844387076, 1.000000000000000000, 0.8660254037844387076, 1.000000000000000000, 0.8660254037844387076, 1.000000000000000000, 0.8660254037844387076, 1.000000000000000000, 0.8660254037844387076, 1.000000000000000000, 0.8660254037844387076, 1.000000000000000000, 0.8660254037844387076, 1.000000000000000000, 0.8660254037844387076, 1.000000000000000000, 0.8660254037844387076, 1.000000000000000000, 0.8660254037844387076, 1.000000000000000000, 0.8660254037844387076, 1.000000000000000000, 0.8660254037844387076, 1.000000000000000000, 0.8660254037844387076, 1.000000000000000000, 0.8660254037844387076, 1.000000000000000000, 0.8660254037844387076, 1.000000000000000000, 0.8660254037844387076, 1.000000000000000000, 0.8660254037844387076, 1.000000000000000000, 0.8660254037844387076, 1.000000000000000000, 0.8660254037844387076, 1.000000000000000000, 0.8660254037844387076, 1.000000000000000000, 0.8660254037844387076, 1.000000000000000000, 0.8660254037844387076, 1.000000000000000000, 0.8660254037844387076, 1.000000000000000000, 0.8660254037844387076, 1.000000000000000000, 0.8660254037844387076, 1.000000000000000000, 0.8660254037844387076, 1.000000000000000000, 0.8660254037844387076, 1.000000000000000000, 0.8660254037844387076, 1.000000000000000000, 0.8660254037844387076, 1.000000000000000000, 0.8660254037844387076, 1.000000000000000000, 0.8660254037844387076, 1.000000000000000000, 0.8660254037844387076, 1.000000000000000000, 0.8660254037844387076, 1.000000000000000000, 0.8660254037844387076, 1.000000000000000000, 0.8660254037844387076, 1.000000000000000000, 0.8660254037844387076, 1.000000000000000000, 0.8660254037844387076, 1.000000000000000000, 0.8660254037844387076, 1.000000000000000000, 0.8660254037844387076, 1.000000000000000000, 0.8660254037844387076, 1.000000000000000000, 0.8660254037844387076, 1.000000000000000000, 0.8660254037844387076, 1.000000000000000000, 0.8660254037844387076, 1.000000000000000000, 0.8660254037844387076, 1.000000000000000000, 0.8660254037844387076, 1.000000000000000000, 0.8660254037844387076, 1.000000000000000000, 0.8660254037844387076, 1.000000000000000000, 0.8660254037844387076, 1.000000000000000000, 0.8660254037844387076, 1.000000000000000000, 0.8660254037844387076, 1.000000000000000000, 0.8660254037844387076, 1.000000000000000000, 0.8660254037844387076, 1.000000000000000000, 0.8660254037844387076, 1.000000000000000000, 0.8660254037844387076, 1.000000000000000000, 0.8660254037844387076, 1.000000000000000000, 0.8660254037844387076, 1.000000000000000000, 0.8660254037844387076, 1.000000000000000000, 0.8660254037844387076, 1.000000000000000000, 0.8660254037844387076, 1.000000000000000000, 0.8660254037844387076, 1.000000000000000000, 0.8660254037844387076, 1.000000000000000000, 0.8660254037844387076, 1.000000000000000000, 0.8660254037844387076, 1.000000000000000000, 0.8660254037844387076, 1.000000000000000000, 0.8660254037844387076, 1.000000000000000000, 0.8660254037844387076, 1.000000000000000000, 0.8660254037844387076, 1.000000000000000000, 0.8660254037844387076, 1.000000000000000000, 0.8660254037844387076, 1.000000000000000000, 0.8660254037844387076, 1.000000000000000000, 0.8660254037844387076, 1.000000000000000000, 0.8660254037844387076, 1.000000000000000000, 0.8660254037844387076, 1.000000000000000000, 0.8660254037844387076, 1.000000000000000000, 0.8660254037844387076, 1.000000000000000000, 0.8660254037844387076, 1.000000000000000000, 0.8660254037844387076, 1.000000000000000000, 0.8660254037844387076, 1.000000000000000000, 0.8660254037844387076, 1.000000000000000000, 0.8660254037844387076, 1.000000000000000000, 0.8660254037844387076, 1.000000000000000000, 0.8660254037844387076, 1.000000000000000000, 0.8660254037844387076, 1.000000000000000000, 0.8660254037844387076, 1.000000000000000000, 0.8660254037844387076, 1.000000000000000000, 0.8660254037844387076, 1.000000000000000000, 0.8660254037844387076, 1.000000000000000000, 0.8660254037844387076, 1.000000000000000000, 0.8660254037844387076, 1.000000000000000000, 0.8660254037844387076, 1.000000000000000000, 0.8660254037844387076, 1.000000000000000000, 0.8660254037844387076, 1.000000000000000000, 0.8660254037844387076, 1.000000000000000000, 0.8660254037844387076, 1.000000000000000000, 0.8660254037844387076, 1.000000000000000000, 0.8660254037844387076, 1.000000000000000000, 0.8660254037844387076, 1.000000000000000000, 0.8660254037844387076, 1.000000000000000000, 0.8660254037844387076, 1.000000000000000000, 0.8660254037844387076, 1.000000000000000000, 0.8660254037844387076, 1.000000000000000000, 0.8660254037844387076, 1.000000000000000000, 0.8660254037844387076, 1.000000000000000000, 0.8660254037844387076, 1.000000000000000000, 0.8660254037844387076, 1.000000000000000000, 0.8660254037844387076, 1.000000000000000000, 0.8660254037844387076, 1.000000000000000000, 0.8660254037844387076, 1.000000000000000000, 0.8660254037844387076, 1.000000000000000000, 0.8660254037844387076, 1.000000000000000000, 0.8660254037844387076, 1.000000000000000000, 0.8660254037844387076, 1.000000000000000000, 0.8660254037844387076, 1.000000000000000000, 0.8660254037844387076, 1.000000000000000000, 0.8660254037844387076, 1.000000000000000000, 0.8660254037844387076, 1.000000000000000000, 0.8660254037844387076, 1.000000000000000000, 0.8660254037844387076, 1.000000000000000000, 0.8660254037844387076, 1.000000000000000000, 0.8660254037844387076, 1.000000000000000000, 0.8660254037844387076, 1.000000000000000000, 0.8660254037844387076, 1.000000000000000000, 0.8660254037844387076, 1.000000000000000000, 0.8660254037844387076, 1.000000000000000000, 0.8660254037844387076, 1.000000000000000000, 0.8660254037844387076, 1.000000000000000000, 0.8660254037844387076, 1.000000000000000000, 0.8660254037844387076, 1.000000000000000000, 0.8660254037844387076, 1.000000000000000000, 0.8660254037844387076, 1.000000000000000000, 0.8660254037844387076, 1.000000000000000000, 0.8660254037844387076, 1.000000000000000000, 0.8660254037844387076, 1.000000000000000000, 0.8660254037844387076, 1.000000000000000000, 0.8660254037844387076, 1.000000000000000000, 0.8660254037844387076, 1.000000000000000000, 0.8660254037844387076, 1.000000000000000000, 0.8660254037844387076, 1.000000000000000000, 0.8660254037844387076, 1.000000000000000000, 0.8660254037844387076, 1.000000000000000000, 0.8660254037844387076, 1.000000000000000000, 0.8660254037844387076, 1.000000000000000000, 0.8660254037844387076, 1.000000000000000000, 0.8660254037844387076, 1.000000000000000000, 0.8660254037844387076, 1.000000000000000000, 0.8660254037844387076, 1.000000000000000000, 0.8660254037844387076, 1.000000000000000000, 0.8660254037844387076, 1.000000000000000000, 0.8660254037844387076, 1.000000000000000000, 0.8660254037844387076, 1.000000000000000000, 0.8660254037844387076, 1.000000000000000000, 0.8660254037844387076, 1.000000000000000000, 0.8660254037844387076, 1.000000000000000000, 0.8660254037844387076, 1.000000000000000000, 0.8660254037844387076, 1.000000000000000000, 0.8660254037844387076, 1.000000000000000000, 0.8660254037844387076, 1.000000000000000000, 0.8660254037844387076, 1.000000000000000000, 0.8660254037844387076, 1.000000000000000000, 0.8660254037844387076, 1.000000000000000000, 0.8660254037844387076, 1.000000000000000000, 0.8660254037844387076, 1.000000000000000000, 0.8660254037844387076, 1.000000000000000000, 0.8660254037844387076, 1.000000000000000000, 0.8660254037844387076, 1.000000000000000000, 0.8660254037844387076, 1.000000000000000000, 0.8660254037844387076, 1.000000000000000000, 0.8660254037844387076, 1.000000000000000000, 0.8660254037844387076, 1.000000000000000000, 0.8660254037844387076, 1.000000000000000000, 0.8660254037844387076, 1.000000000000000000, 0.8660254037844387076, 1.000000000000000000, 0.8660254037844387076, 1.000000000000000000, 0.8660254037844387076, 1.000000000000000000, 0.8660254037844387076, 1.000000000000000000, 0.8660254037844387076, 1.000000000000000000, 0.8660254037844387076, 1.000000000000000000, 0.8660254037844387076, 1.000000000000000000, 0.8660254037844387076, 1.000000000000000000, 0.8660254037844387076, 1.000000000000000000, 0.8660254037844387076, 1.000000000000000000, 0.8660254037844387076, 1.000000000000000000, 0.8660254037844387076, 1.000000000000000000, 0.8660254037844387076, 1.000000000000000000),
 ( 1.000000000000000000, 0.8660254037844387076, 1.000000000000000000, 0.8660254037844387076, 1.000000000000000000, 0.8660254037844387076, 1.000000000000000000, 0.8660254037844387076, 1.000000000000000000, 0.8660254037844387076, 1.000000000000000000, 0.8660254037844387076, 1.000000000000000000, 0.8660254037844387076, 1.000000000000000000, 0.8660254037844387076, 1.000000000000000000, 0.8660254037844387076, 1.000000000000000000, 0.8660254037844387076, 1.000000000000000000, 0.8660254037844387076, 1.000000000000000000, 0.8660254037844387076, 1.000000000000000000, 0.8660254037844387076, 1.000000000000000000, 0.8660254037844387076, 1.000000000000000000, 0.8660254037844387076, 1.000000000000000000, 0.8660254037844387076, 1.000000000000000000, 0.8660254037844387076, 1.000000000000000000, 0.8660254037844387076, 1.000000000000000000, 0.8660254037844387076, 1.000000000000000000, 0.8660254037844387076, 1.000000000000000000, 0.8660254037844387076, 1.000000000000000000, 0.8660254037844387076, 1.000000000000000000, 0.8660254037844387076, 1.000000000000000000, 0.8660254037844387076, 1.000000000000000000, 0.8660254037844387076, 1.000000000000000000, 0.8660254037844387076, 1.000000000000000000, 0.8660254037844387076, 1.000000000000000000, 0.8660254037844387076, 1.000000000000000000, 0.8660254037844387076, 1.000000000000000000, 0.8660254037844387076, 1.000000000000000000, 0.8660254037844387076, 1.000000000000000000, 0.8660254037844387076, 1.000000000000000000, 0.8660254037844387076, 1.000000000000000000, 0.8660254037844387076, 1.000000000000000000, 0.8660254037844387076, 1.000000000000000000, 0.8660254037844387076, 1.000000000000000000, 0.8660254037844387076, 1.000000000000000000, 0.8660254037844387076, 1.000000000000000000, 0.8660254037844387076, 1.000000000000000000, 0.8660254037844387076, 1.000000000000000000, 0.8660254037844387076, 1.000000000000000000, 0.8660254037844387076, 1.000000000000000000, 0.8660254037844387076, 1.000000000000000000, 0.8660254037844387076, 1.000000000000000000, 0.8660254037844387076, 1.000000000000000000, 0.8660254037844387076, 1.000000000000000000, 0.8660254037844387076, 1.000000000000000000, 0.8660254037844387076, 1.000000000000000000, 0.8660254037844387076, 1.000000000000000000, 0.8660254037844387076, 1.000000000000000000, 0.8660254037844387076, 1.000000000000000000, 0.8660254037844387076, 1.000000000000000000, 0.8660254037844387076, 1.000000000000000000, 0.8660254037844387076, 1.000000000000000000, 0.8660254037844387076, 1.000000000000000000, 0.8660254037844387076, 1.000000000000000000, 0.8660254037844387076, 1.000000000000000000, 0.8660254037844387076, 1.000000000000000000, 0.8660254037844387076, 1.000000000000000000, 0.8660254037844387076, 1.000000000000000000, 0.8660254037844387076, 1.000000000000000000, 0.8660254037844387076, 1.000000000000000000, 0.8660254037844387076, 1.000000000000000000, 0.8660254037844387076, 1.000000000000000000, 0.8660254037844387076, 1.000000000000000000, 0.8660254037844387076, 1.000000000000000000, 0.8660254037844387076, 1.000000000000000000, 0.8660254037844387076, 1.000000000000000000, 0.8660254037844387076, 1.000000000000000000, 0.8660254037844387076, 1.000000000000000000, 0.8660254037844387076, 1.000000000000000000, 0.8660254037844387076, 1.000000000000000000, 0.8660254037844387076, 1.000000000000000000, 0.8660254037844387076, 1.000000000000000000, 0.8660254037844387076, 1.000000000000000000, 0.8660254037844387076, 1.000000000000000000, 0.8660254037844387076, 1.000000000000000000, 0.8660254037844387076, 1.000000000000000000, 0.8660254037844387076, 1.000000000000000000, 0.8660254037844387076, 1.000000000000000000, 0.8660254037844387076, 1.000000000000000000, 0.8660254037844387076, 1.000000000000000000, 0.8660254037844387076, 1.000000000000000000, 0.8660254037844387076, 1.000000000000000000, 0.8660254037844387076, 1.000000000000000000, 0.8660254037844387076, 1.000000000000000000, 0.8660254037844387076, 1.000000000000000000, 0.8660254037844387076, 1.000000000000000000, 0.8660254037844387076, 1.000000000000000000, 0.8660254037844387076, 1.000000000000000000, 0.8660254037844387076, 1.000000000000000000, 0.8660254037844387076, 1.000000000000000000, 0.8660254037844387076, 1.000000000000000000, 0.8660254037844387076, 1.000000000000000000, 0.8660254037844387076, 1.000000000000000000, 0.8660254037844387076, 1.000000000000000000, 0.8660254037844387076, 1.000000000000000000, 0.8660254037844387076, 1.000000000000000000, 0.8660254037844387076, 1.000000000000000000, 0.8660254037844387076, 1.000000000000000000, 0.8660254037844387076, 1.000000000000000000, 0.8660254037844387076, 1.000000000000000000, 0.8660254037844387076, 1.000000000000000000, 0.8660254037844387076, 1.000000000000000000, 0.8660254037844387076, 1.000000000000000000, 0.8660254037844387076, 1.000000000000000000, 0.8660254037844387076, 1.000000000000000000, 0.8660254037844387076, 1.000000000000000000, 0.8660254037844387076, 1.000000000000000000, 0.8660254037844387076, 1.000000000000000000, 0.8660254037844387076, 1.000000000000000000, 0.8660254037844387076, 1.000000000000000000, 0.8660254037844387076, 1.000000000000000000, 0.8660254037844387076, 1.000000000000000000, 0.8660254037844387076, 1.000000000000000000, 0.8660254037844387076, 1.000000000000000000, 0.8660254037844387076, 1.000000000000000000, 0.8660254037844387076, 1.000000000000000000, 0.8660254037844387076, 1.000000000000000000, 0.8660254037844387076, 1.000000000000000000, 0.8660254037844387076, 1.000000000000000000, 0.8660254037844387076, 1.000000000000000000, 0.8660254037844387076, 1.000000000000000000, 0.8660254037844387076, 1.000000000000000000, 0.8660254037844387076, 1.000000000000000000, 0.8660254037844387076, 1.000000000000000000, 0.8660254037844387076, 1.000000000000000000, 0.8660254037844387076, 1.000000000000000000, 0.8660254037844387076, 1.000000000000000000, 0.8660254037844387076, 1.000000000000000000, 0.8660254037844387076, 1.000000000000000000, 0.8660254037844387076, 1.000000000000000000, 0.8660254037844387076, 1.000000000000000000, 0.8660254037844387076, 1.000000000000000000, 0.8660254037844387076, 1.000000000000000000, 0.8660254037844387076, 1.000000000000000000, 0.8660254037844387076, 1.000000000000000000, 0.8660254037844387076, 1.000000000000000000, 0.8660254037844387076, 1.000000000000000000, 0.8660254037844387076, 1.000000000000000000, 0.8660254037844387076, 1.000000000000000000, 0.8660254037844387076, 1.000000000000000000, 0.8660254037844387076, 1.000000000000000000, 0.8660254037844387076, 1.000000000000000000, 0.8660254037844387076, 1.000000000000000000, 0.8660254037844387076, 1.000000000000000000, 0.8660254037844387076, 1.000000000000000000, 0.8660254037844387076, 1.000000000000000000, 0.8660254037844387076, 1.000000000000000000, 0.8660254037844387076, 1.000000000000000000, 0.8660254037844387076, 1.000000000000000000, 0.8660254037844387076, 1.000000000000000000, 0.8660254037844387076, 1.000000000000000000, 0.8660254037844387076, 1.000000000000000000, 0.8660254037844387076, 1.000000000000000000, 0.8660254037844387076, 1.000000000000000000, 0.8660254037844387076, 1.000000000000000000, 0.8660254037844387076, 1.000000000000000000, 0.8660254037844387076, 1.000000000000000000, 0.8660254037844387076, 1.000000000000000000, 0.8660254037844387076, 1.000000000000000000, 0.8660254037844387076, 1.000000000000000000, 0.8660254037844387076, 1.000000000000000000, 0.8660254037844387076, 1.000000000000000000, 0.8660254037844387076, 1.000000000000000000, 0.8660254037844387076, 1.000000000000000000, 0.8660254037844387076, 1.000000000000000000, 0.8660254037844387076, 1.000000000000000000, 0.8660254037844387076, 1.000000000000000000, 0.8660254037844387076, 1.000000000000000000, 0.8660254037844387076, 1.000000000000000000, 0.8660254037844387076, 1.000000000000000000, 0.8660254037844387076, 1.000000000000000000, 0.8660254037844387076, 1.000000000000000000, 0.8660254037844387076, 1.000000000000000000, 0.8660254037844387076, 1.000000000000000000, 0.8660254037844387076, 1.000000000000000000, 0.8660254037844387076, 1.000000000000000000, 0.8660254037844387076, 1.000000000000000000, 0.8660254037844387076, 1.000000000000000000, 0.8660254037844387076, 1.000000000000000000, 0.8660254037844387076, 1.000000000000000000, 0.8660254037844387076, 1.000000000000000000, 0.8660254037844387076, 1.000000000000000000, 0.8660254037844387076, 1.000000000000000000, 0.8660254037844387076, 1.000000000000000000, 0.8660254037844387076, 1.000000000000000000, 0.8660254037844387076, 1.000000000000000000, 0.8660254037844387076, 1.000000000000000000, 0.8660254037844387076, 1.000000000000000000, 0.8660254037844387076, 1.000000000000000000, 0.8660254037844387076, 1.000000000000000000, 0.8660254037844387076, 1.000000000000000000, 0.8660254037844387076, 1.000000000000000000, 0.8660254037844387076, 1.000000000000000000, 0.8660254037844387076, 1.000000000000000000, 0.8660254037844387076, 1.000000000000000000, 0.8660254037844387076, 1.000000000000000000, 0.8660254037844387076, 1.000000000000000000, 0.8660254037844387076, 1.000000000000000000, 0.8660254037844387076, 1.000000000000000000, 0.8660254037844387076, 1.000000000000000000, 0.8660254037844387076, 1.000000000000000000, 0.8660254037844387076, 1.000000000000000000, 0.8660254037844387076, 1.000000000000000000, 0.8660254037844387076, 1.000000000000000000, 0.8660254037844387076, 1.000000000000000000, 0.8660254037844387076, 1.000000000000000000, 0.8660254037844387076, 1.000000000000000000, 0.8660254037844387076, 1.000000000000000000, 0.8660254037844387076, 1.000000000000000000, 0.8660254037844387076, 1.000000000000000000, 0.8660254037844387076, 1.000000000000000000, 0.8660254037844387076, 1.000000000000000000, 0.8660254037844387076, 1.000000000000000000, 0.8660254037844387076, 1.000000000000000000, 0.8660254037844387076, 1.000000000000000000, 0.8660254037844387076, 1.000000000000000000, 0.8660254037844387076, 1.000000000000000000, 0.8660254037844387076, 1.000000000000000000, 0.8660254037844387076, 1.000000000000000000, 0.8660254037844387076, 1.000000000000000000, 0.8660254037844387076, 1.000000000000000000, 0.8660254037844387076, 1.000000000000000000, 0.8660254037844387076, 1.000000000000000000, 0.8660254037844387076, 1.000000000000000000, 0.8660254037844387076, 1.000000000000000000, 0.8660254037844387076, 1.000000000000000000, 0.8660254037844387076, 1.000000000000000000, 0.8660254037844387076, 1.000000000000000000, 0.8660254037844387076, 1.000000000000000000, 0.8660254037844387076, 1.000000000000000000, 0.8660254037844387076, 1.000000000000000000, 0.8660254037844387076, 1.000000000000000000, 0.8660254037844387076, 1.000000000000000000, 0.8660254037844387076, 1.000000000000000000, 0.8660254037844387076, 1.000000000000000000, 0.8660254037844387076, 1.000000000000000000, 0.8660254037844387076, 1.000000000000000000, 0.8660254037844387076, 1.000000000000000000, 0.8660254037844387076, 1.000000000000000000, 0.8660254037844387076, 1.000000000000000000, 0.8660254037844387076, 1.000000000000000000, 0.8660254037844387076, 1.000000000000000000, 0.8660254037844387076, 1.000000000000000000, 0.8660254037844387076, 1.000000000000000000, 0.8660254037844387076, 1.000000000000000000, 0.8660254037844387076, 1.000000000000000000, 0.8660254037844387076, 1.000000000000000000, 0.8660254037844387076, 1.000000000000000000, 0.8660254037844387076, 1.000000000000000000, 0.8660254037844387076, 1.000000000000000000, 0.8660254037844387076, 1.000000000000000000, 0.8660254037844387076, 1.000000000000000000, 0.8660254037844387076, 1.000000000000000000, 0.8660254037844387076, 1.000000000000000000, 0.8660254037844387076, 1.000000000000000000, 0.8660254037844387076, 1.000000000000000000, 0.8660254037844387076, 1.000000000000000000, 0.8660254037844387076, 1.000000000000000000, 0.8660254037844387076, 1.000000000000000000, 0.8660254037844387076, 1.000000000000000000, 0.8660254037844387076, 1.000000000000000000, 0.8660254037844387076, 1.000000000000000000, 0.8660254037844387076, 1.000000000000000000, 0.8660254037844387076, 1.000000000000000000, 0.8660254037844387076, 1.000000000000000000, 0.8660254037844387076, 1.000000000000000000, 0.8660254037844387076, 1.000000000000000000, 0.8660254037844387076, 1.000000000000000000, 0.8660254037844387076, 1.000000000000000000, 0.8660254037844387076, 1.000000000000000000, 0.8660254037844387076, 1.000000000000000000, 0.8660254037844387076, 1.000000000000000000, 0.8660254037844387076, 1.000000000000000000, 0.8660254037844387076, 1.000000000000000000, 0.8660254037844387076, 1.000000000000000000, 0.8660254037844387076, 1.000000000000000000, 0.8660254037844387076, 1.000000000000000000, 0.8660254037844387076, 1.000000000000000000, 0.8660254037844387076, 1.000000000000000000, 0.8660254037844387076, 1.000000000000000000, 0.8660254037844387076, 1.000000000000000000, 0.8660254037844387076, 1.000000000000000000, 0.8660254037844387076, 1.000000000000000000, 0.8660254037844387076, 1.000000000000000000, 0.8660254037844387076, 1.000000000000000000, 0.8660254037844387076, 1.000000000000000000, 0.8660254037844387076, 1.000000000000000000, 0.8660254037844387076, 1.000000000000000000, 0.8660254037844387076, 1.000000000000000000, 0.8660254037844387076, 1.000000000000000000, 0.8660254037844387076, 1.000000000000000000, 0.8660254037844387076, 1.000000000000000000, 0.8660254037844387076, 1.000000000000000000, 0.8660254037844387076, 1.000000000000000000, 0.8660254037844387076, 1.000000000000000000, 0.8660254037844387076, 1.000000000000000000, 0.8660254037844387076, 1.000000000000000000, 0.8660254037844387076, 1.000000000000000000, 0.8660254037844387076, 1.000000000000000000, 0.8660254037844387076, 1.000000000000000000, 0.8660254037844387076, 1.000000000000000000, 0.8660254037844387076, 1.000000000000000000, 0.8660254037844387076, 1.000000000000000000, 0.8660254037844387076, 1.000000000000000000, 0.8660254037844387076, 1.000000000000000000, 0.8660254037844387076, 1.000000000000000000, 0.8660254037844387076, 1.000000000000000000, 0.8660254037844387076, 1.000000000000000000, 0.8660254037844387076, 1.000000000000000000, 0.8660254037844387076, 1.000000000000000000, 0.8660254037844387076, 1.000000000000000000, 0.8660254037844387076, 1.000000000000000000, 0.8660254037844387076, 1.000000000000000000, 0.8660254037844387076, 1.000000000000000000, 0.8660254037844387076, 1.000000000000000000, 0.8660254037844387076, 1.000000000000000000, 0.8660254037844387076, 1.000000000000000000, 0.8660254037844387076, 1.000000000000000000, 0.8660254037844387076, 1.000000000000000000, 0.8660254037844387076, 1.000000000000000000, 0.8660254037844387076, 1.000000000000000000, 0.8660254037844387076, 1.000000000000000000, 0.8660254037844387076, 1.000000000000000000, 0.8660254037844387076, 1.000000000000000000, 0.8660254037844387076, 1.000000000000000000, 0.8660254037844387076, 1.000000000000000000, 0.8660254037844387076, 1.000000000000000000, 0.8660254037844387076, 1.000000000000000000, 0.8660254037844387076, 1.000000000000000000, 0.8660254037844387076, 1.000000000000000000, 0.8660254037844387076, 1.000000000000000000, 0.8660254037844387076, 1.000000000000000000, 0.8660254037844387076, 1.000000000000000000, 0.8660254037844387076, 1.000000000000000000, 0.8660254037844387076, 1.000000000000000000, 0.8660254037844387076, 1.000000000000000000, 0.8660254037844387076, 1.000000000000000000, 0.8660254037844387076, 1.000000000000000000, 0.8660254037844387076, 1.000000000000000000, 0.8660254037844387076, 1.000000000000000000, 0.8660254037844387076, 1.000000000000000000, 0.8660254037844387076, 1.000000000000000000, 0.8660254037844387076, 1.000000000000000000, 0.8660254037844387076, 1.000000000000000000, 0.8660254037844387076, 1.000000000000000000, 0.8660254037844387076, 1.000000000000000000, 0.8660254037844387076, 1.000000000000000000, 0.8660254037844387076, 1.000000000000000000, 0.8660254037844387076, 1.000000000000000000, 0.8660254037844387076, 1.000000000000000000, 0.8660254037844387076, 1.000000000000000000, 0.8660254037844387076, 1.000000000000000000, 0.8660254037844387076, 1.000000000000000000, 0.8660254037844387076, 1.000000000000000000, 0.8660254037844387076, 1.000000000000000000, 0.8660254037844387076, 1.000000000000000000, 0.8660254037844387076, 1.000000000000000000, 0.8660254037844387076, 1.000000000000000000) ) ) 
 REPRESENTATION_ITEM ( '' )  SURFACE ( )  );
#72561 = CARTESIAN_POINT ( 'NONE',  ( 6.750000001229033764, -2.886751345948129988, 4.999999999999997335 ) ) ;
#72562 = CARTESIAN_POINT ( 'NONE',  ( 20.20312500061451644, 4.541064518000418104, -2.621784821874998173 ) ) ;
#72563 = CARTESIAN_POINT ( 'NONE',  ( 7.800000001229035362, -2.886751345948125991, -5.000000000000000000 ) ) ;
#72564 = CARTESIAN_POINT ( 'NONE',  ( 17.24062500061451786, -3.027376345333614438, 5.243569643749998122 ) ) ;
#72565 = CARTESIAN_POINT ( 'NONE',  ( 16.11562500061451786, 3.027376345333613106, -5.243569643749998122 ) ) ;
#72566 = CARTESIAN_POINT ( 'NONE',  ( 25.50937500061451502, -4.119189519843965641, -2.378215178125001383 ) ) ;
#72567 = CARTESIAN_POINT ( 'NONE',  ( 15.37500000000000000, 6.123233995736764310E-16, -4.999999999999998224 ) ) ;
#72568 = CARTESIAN_POINT ( 'NONE',  ( 10.50000000122903465, -2.886751345948125991, -5.000000000000000000 ) ) ;
#72569 = CARTESIAN_POINT ( 'NONE',  ( 8.803125000614517859, -4.541064518000417216, -2.621784821875001281 ) ) ;
#72570 = CARTESIAN_POINT ( 'NONE',  ( 10.71562500061451928, 3.027376345333613106, -5.243569643749998122 ) ) ;
#72571 = CARTESIAN_POINT ( 'NONE',  ( 21.48750000122903003, 4.330127018922191873, 2.499999999999999556 ) ) ;
#72572 = CARTESIAN_POINT ( 'NONE',  ( 27.29999999999999716, 0.000000000000000000, 4.999999999999998224 ) ) ;
#72573 = AXIS2_PLACEMENT_3D ( 'NONE', #30909, #36819, #37183 ) ;
#72574 = CARTESIAN_POINT ( 'NONE',  ( 2.121784821875001281, 12.80937500061451928, -26.32496088578401938 ) ) ;
#72575 = CARTESIAN_POINT ( 'NONE',  ( 9.750000000000001776, 0.000000000000000000, 4.999999999999998224 ) ) ;
#72576 = CARTESIAN_POINT ( 'NONE',  ( 6.412500001229036073, -4.330127018922190985, -2.500000000000001332 ) ) ;
#72577 = VECTOR ( 'NONE', #58856, 1000.000000000000000 ) ;
#72578 = CARTESIAN_POINT ( 'NONE',  ( 4.096875000614518925, 6.054752690667223547, 3.707466751127219781E-16 ) ) ;
#72579 = CARTESIAN_POINT ( 'NONE',  ( 19.77187500061451786, 3.027376345333613106, -5.243569643749998122 ) ) ;
#72580 = LINE ( 'NONE', #67415, #26857 ) ;
#72581 = AXIS2_PLACEMENT_3D ( 'NONE', #15153, #15515, #54692 ) ;
#72582 = CARTESIAN_POINT ( 'NONE',  ( 15.74062500061451608, 6.054752690667223547, 3.707466751127219781E-16 ) ) ;
#72583 = CARTESIAN_POINT ( 'NONE',  ( 12.35625000122903394, 4.330127018922192761, -2.499999999999997780 ) ) ;
#72584 = CARTESIAN_POINT ( 'NONE',  ( -1.071796769724479903, 20.86115380933863150, 34.00000000000000711 ) ) ;
#72585 = CARTESIAN_POINT ( 'NONE',  ( -3.999999999999997335, 15.53750000000000142, 32.30940107675850470 ) ) ;
#72586 = CARTESIAN_POINT ( 'NONE',  ( 29.18437500061451573, 6.421520780324663323E-16, -5.243569643749999010 ) ) ;
#72587 = CARTESIAN_POINT ( 'NONE',  ( 21.87187500061451573, 5.824947211148865298E-16, -4.756430356249998326 ) ) ;
#72588 = CARTESIAN_POINT ( 'NONE',  ( 14.20312500061451644, -4.541064518000417216, -2.621784821875001281 ) ) ;
#72589 = VECTOR ( 'NONE', #22421, 1000.000000000000000 ) ;
#72590 = CARTESIAN_POINT ( 'NONE',  ( 11.55937500061451928, -4.541064518000417216, -2.621784821875001281 ) ) ;
#72591 = ORIENTED_EDGE ( 'NONE', *, *, #48506, .T. ) ;
#72592 = CARTESIAN_POINT ( 'NONE',  ( 9.449999999999999289, -4.330127018922190985, -2.500000000000001332 ) ) ;
#72593 = CARTESIAN_POINT ( 'NONE',  ( 21.59062500061451928, 6.054752690667223547, 3.707466751127219781E-16 ) ) ;
#72594 = CARTESIAN_POINT ( 'NONE',  ( 17.55000000122903003, -2.886751345948063374, 5.000000000000112799 ) ) ;
#72595 = CARTESIAN_POINT ( 'NONE',  ( 28.61250000122903359, 4.330127018922192761, -2.499999999999997780 ) ) ;
#72596 = CARTESIAN_POINT ( 'NONE',  ( 12.07499999999999929, -4.330127018922194537, 2.499999999999995559 ) ) ;
#72597 = CARTESIAN_POINT ( 'NONE',  ( 20.88750000122903572, 6.123233995736764310E-16, -4.999999999999998224 ) ) ;
#72598 = CARTESIAN_POINT ( 'NONE',  ( 16.26562500061451289, 3.027376345333611329, 5.243569643749999010 ) ) ;
#72599 = CARTESIAN_POINT ( 'NONE',  ( 13.95937500061451608, 2.746126346562643317, 4.756430356249998326 ) ) ;
#72600 = VERTEX_POINT ( 'NONE', #36823 ) ;
#72601 = CARTESIAN_POINT ( 'NONE',  ( 20.81250000000000000, 2.886751345948129099, -4.999999999999998224 ) ) ;
#72602 = EDGE_CURVE ( 'NONE', #24717, #69279, #42008, .T. ) ;
#72603 =( BOUNDED_CURVE ( )  B_SPLINE_CURVE ( 2, ( #59719, #8757, #25381, #26858, #71555, #70454, #20930 ),
 .UNSPECIFIED., .F., .F. ) 
 B_SPLINE_CURVE_WITH_KNOTS ( ( 3, 2, 2, 3 ),
 ( 0.9599999999999999645, 0.9633333333333333748, 0.9666666666666666741, 0.9699999999999999734 ),
 .UNSPECIFIED. ) 
 CURVE ( )  GEOMETRIC_REPRESENTATION_ITEM ( )  RATIONAL_B_SPLINE_CURVE ( ( 1.000000000000000000, 0.8660254037844387076, 1.000000000000000000, 0.8660254037844387076, 1.000000000000000000, 0.8660254037844387076, 1.000000000000000000 ) ) 
 REPRESENTATION_ITEM ( '' )  );
#72604 = CARTESIAN_POINT ( 'NONE',  ( 20.78437500061451715, 4.541064518000418104, 2.621784821874999949 ) ) ;
#72605 = CARTESIAN_POINT ( 'NONE',  ( 27.36562500061451786, 3.027376345333613106, -5.243569643749998122 ) ) ;
#72606 = ORIENTED_EDGE ( 'NONE', *, *, #21587, .T. ) ;
#72607 = CARTESIAN_POINT ( 'NONE',  ( 14.36250000122903359, 0.000000000000000000, 4.999999999999998224 ) ) ;
#72608 = CARTESIAN_POINT ( 'NONE',  ( 10.79062500061451679, 6.054752690667223547, 3.707466751127219781E-16 ) ) ;
#72609 = CARTESIAN_POINT ( 'NONE',  ( 30.00000000000000000, 0.000000000000000000, 4.999999999999998224 ) ) ;
#72610 = CARTESIAN_POINT ( 'NONE',  ( 17.77499999999999858, 4.330127018922191873, 2.499999999999999556 ) ) ;
#72611 = CARTESIAN_POINT ( 'NONE',  ( 23.40000000000000213, -4.330127018922190985, -2.500000000000001332 ) ) ;
#72612 = FACE_OUTER_BOUND ( 'NONE', #55977, .T. ) ;
#72613 = CARTESIAN_POINT ( 'NONE',  ( 4.809375000614516615, -4.541064518000417216, -2.621784821875001281 ) ) ;
#72614 = CARTESIAN_POINT ( 'NONE',  ( 28.13437500061451502, -4.541064518000419881, 2.621784821874995952 ) ) ;
#72615 = ORIENTED_EDGE ( 'NONE', *, *, #32398, .T. ) ;
#72616 = CARTESIAN_POINT ( 'NONE',  ( 24.66562500061451502, 3.027376345333613106, -5.243569643749998122 ) ) ;
#72617 = CARTESIAN_POINT ( 'NONE',  ( 24.45937500061451786, 0.000000000000000000, 5.243569643749999010 ) ) ;
#72618 = CARTESIAN_POINT ( 'NONE',  ( -3.000416591977282496E-16, 19.69062500061459176, -34.90005215228797653 ) ) ;
#72619 = CARTESIAN_POINT ( 'NONE',  ( 14.24999999999999822, 0.000000000000000000, 4.999999999999998224 ) ) ;
#72620 = CARTESIAN_POINT ( 'NONE',  ( 8.090625000614515727, 6.054752690667223547, 3.707466751127219781E-16 ) ) ;
#72621 = CARTESIAN_POINT ( 'NONE',  ( 3.761592534273730415, 3.294057342109477649, 3.962396521687911566 ) ) ;
#72622 = CARTESIAN_POINT ( 'NONE',  ( 19.65000000000000213, 0.000000000000000000, 4.999999999999998224 ) ) ;
#72623 = CARTESIAN_POINT ( 'NONE',  ( 26.24062500061451431, -3.027376345333614438, 5.243569643749998122 ) ) ;
#72624 = CARTESIAN_POINT ( 'NONE',  ( 17.17500000122903359, -5.773502691896255534, -1.060575238724906372E-15 ) ) ;
#72625 = CYLINDRICAL_SURFACE ( 'NONE', #14724, 4.000000000000000000 ) ;
#72626 = CARTESIAN_POINT ( 'NONE',  ( 16.17187500061451644, 2.746126346562645981, -4.756430356249997438 ) ) ;
#72627 = CARTESIAN_POINT ( 'NONE',  ( 3.703125000614516882, 0.000000000000000000, 5.243569643749999010 ) ) ;
#72628 = CARTESIAN_POINT ( 'NONE',  ( 21.08437500061451786, 6.421520780324663323E-16, -5.243569643749999010 ) ) ;
#72629 = CARTESIAN_POINT ( 'NONE',  ( -2.121784821874996840, 15.88437500061451857, 33.67503911421598417 ) ) ;
#72630 = CARTESIAN_POINT ( 'NONE',  ( 21.15937500061451715, 4.541064518000418104, -2.621784821874998173 ) ) ;
#72631 = CARTESIAN_POINT ( 'NONE',  ( 28.54687500061451644, -3.027376345333614438, 5.243569643749998122 ) ) ;
#72632 = CARTESIAN_POINT ( 'NONE',  ( 10.65000000000000036, 0.000000000000000000, 4.999999999999998224 ) ) ;
#72633 = CARTESIAN_POINT ( 'NONE',  ( 10.00312500061451715, 0.000000000000000000, 5.243569643749999010 ) ) ;
#72634 = CARTESIAN_POINT ( 'NONE',  ( 1.071796769724495668, 17.09509619066136921, 34.00000000000000000 ) ) ;
#72635 = CARTESIAN_POINT ( 'NONE',  ( 6.346875000614517148, 6.054752690667223547, 3.707466751127219781E-16 ) ) ;
#72636 = CARTESIAN_POINT ( 'NONE',  ( 8.315625000614515372, -6.054752690667223547, -1.112240025338166033E-15 ) ) ;
#72637 = CARTESIAN_POINT ( 'NONE',  ( 12.15937500061451892, 4.541064518000418104, -2.621784821874998173 ) ) ;
#72638 = PRESENTATION_STYLE_ASSIGNMENT (( #56010 ) ) ;
#72639 = CARTESIAN_POINT ( 'NONE',  ( 19.95000000122903572, -2.886751345948125991, -5.000000000000000000 ) ) ;
#72640 = CARTESIAN_POINT ( 'NONE',  ( 7.921875000614517326, -6.054752690667223547, -1.112240025338166033E-15 ) ) ;
#72641 = CARTESIAN_POINT ( 'NONE',  ( 9.703125000614514661, -4.541064518000417216, -2.621784821875001281 ) ) ;
#72642 = CARTESIAN_POINT ( 'NONE',  ( 8.128125000614515372, 4.541064518000418104, 2.621784821874999949 ) ) ;
#72643 = CARTESIAN_POINT ( 'NONE',  ( 25.10625000122903216, 0.000000000000000000, 4.999999999999998224 ) ) ;
#72644 = CARTESIAN_POINT ( 'NONE',  ( 18.30937500061451928, -4.541064518000417216, -2.621784821875001281 ) ) ;
#72645 = CARTESIAN_POINT ( 'NONE',  ( -5.810221930991193690E-16, 11.45000000122903216, 26.00000000000000355 ) ) ;
#72646 = CARTESIAN_POINT ( 'NONE',  ( 26.50312500061451360, 4.541064518000418104, -2.621784821874998173 ) ) ;
#72647 = VECTOR ( 'NONE', #19237, 1000.000000000000000 ) ;
#72648 = CARTESIAN_POINT ( 'NONE',  ( 11.87812500061451537, -4.541064518000419881, 2.621784821874995952 ) ) ;
#72649 = EDGE_CURVE ( 'NONE', #12632, #49222, #8030, .T. ) ;
#72650 = CARTESIAN_POINT ( 'NONE',  ( 28.54687500061451644, -3.027376345333614438, 5.243569643749998122 ) ) ;
#72651 = CARTESIAN_POINT ( 'NONE',  ( 2.121784821874999061, 12.05937500061451750, -33.67503911421598417 ) ) ;
#72652 = CARTESIAN_POINT ( 'NONE',  ( 11.77500000122903501, -5.773502691896255534, -1.060575238724906372E-15 ) ) ;
#72653 = CARTESIAN_POINT ( 'NONE',  ( 4.243569643749999010, 15.56562500061451715, -32.45002607614398471 ) ) ;
#72654 = CARTESIAN_POINT ( 'NONE',  ( 14.58750000122903323, 6.123233995736764310E-16, -4.999999999999998224 ) ) ;
#72655 = CARTESIAN_POINT ( 'NONE',  ( 9.665625000614515017, -6.054752690667223547, -1.112240025338166033E-15 ) ) ;
#72656 = AXIS2_PLACEMENT_3D ( 'NONE', #29966, #52507, #13700 ) ;
#72657 = CARTESIAN_POINT ( 'NONE',  ( 12.59999999999999964, -4.330127018922190985, -2.500000000000001332 ) ) ;
#72658 = CARTESIAN_POINT ( 'NONE',  ( 10.48125000122903216, 6.123233995736764310E-16, -4.999999999999998224 ) ) ;
#72659 = CARTESIAN_POINT ( 'NONE',  ( 23.57812500061451289, -4.541064518000419881, 2.621784821874995952 ) ) ;
#72660 = CARTESIAN_POINT ( 'NONE',  ( 7.584375000614516082, 6.421520780324663323E-16, -5.243569643749999010 ) ) ;
#72661 = EDGE_CURVE ( 'NONE', #62948, #39309, #55032, .T. ) ;
#72662 = CARTESIAN_POINT ( 'NONE',  ( 10.08750000122903323, 6.123233995736764310E-16, -4.999999999999998224 ) ) ;
#72663 = CARTESIAN_POINT ( 'NONE',  ( 17.77500000122903145, 2.886751345948129099, -4.999999999999998224 ) ) ;
#72664 = CARTESIAN_POINT ( 'NONE',  ( 16.15312500061451573, 4.541064518000418104, -2.621784821874998173 ) ) ;
#72665 = CARTESIAN_POINT ( 'NONE',  ( 18.89062500061451644, 6.054752690667223547, 3.707466751127219781E-16 ) ) ;
#72666 = CARTESIAN_POINT ( 'NONE',  ( 26.51250000122903216, 0.000000000000000000, 4.999999999999998224 ) ) ;
#72667 = CARTESIAN_POINT ( 'NONE',  ( 27.60000000122903430, -2.886751345948125991, -5.000000000000000000 ) ) ;
#72668 = CARTESIAN_POINT ( 'NONE',  ( 22.12500000000000000, 6.123233995736764310E-16, -4.999999999999998224 ) ) ;
#72669 = CARTESIAN_POINT ( 'NONE',  ( -1.878215178125001827, 13.39062499938548356, 33.25316411605952283 ) ) ;
#72670 = CARTESIAN_POINT ( 'NONE',  ( 25.32187500061451857, 3.027376345333611329, 5.243569643749999010 ) ) ;
#72671 = CARTESIAN_POINT ( 'NONE',  ( 18.33750000122903501, 4.330127018922191873, 2.499999999999999556 ) ) ;
#72672 = CARTESIAN_POINT ( 'NONE',  ( 12.86250000122903359, 4.330127018922192761, -2.499999999999997780 ) ) ;
#72673 = CARTESIAN_POINT ( 'NONE',  ( 27.68437500061451573, -4.541064518000419881, 2.621784821874995952 ) ) ;
#72674 = CARTESIAN_POINT ( 'NONE',  ( 4.284375000614518925, -4.541064518000419881, 2.621784821874995952 ) ) ;
#72675 = CARTESIAN_POINT ( 'NONE',  ( 23.91562500061451502, 3.027376345333611329, 5.243569643749999010 ) ) ;
#72676 = CARTESIAN_POINT ( 'NONE',  ( 3.756430356249998770, 14.06562499938548250, 32.16877607737301759 ) ) ;
#72677 = CARTESIAN_POINT ( 'NONE',  ( -3.999999999999999112, 15.33124999877096606, 27.69059892324149530 ) ) ;
#72678 = AXIS2_PLACEMENT_3D ( 'NONE', #33026, #21570, #61461 ) ;
#72679 = CARTESIAN_POINT ( 'NONE',  ( 10.54687500061451644, -3.027376345333614438, 5.243569643749998122 ) ) ;
#72680 = CARTESIAN_POINT ( 'NONE',  ( 30.00000000000000000, 6.123233995736764310E-16, -4.999999999999998224 ) ) ;
#72681 = CARTESIAN_POINT ( 'NONE',  ( 2.971875000614517592, -6.054752690667223547, -1.112240025338166033E-15 ) ) ;
#72682 = CARTESIAN_POINT ( 'NONE',  ( 6.796875000614516438, 6.054752690667223547, 3.707466751127219781E-16 ) ) ;
#72683 = CARTESIAN_POINT ( 'NONE',  ( 29.14687500061451075, -3.027376345333610441, -5.243569643749999898 ) ) ;
#72684 = CARTESIAN_POINT ( 'NONE',  ( -4.243569643749999898, 10.31562500061459531, 27.54997392385601529 ) ) ;
#72685 = CARTESIAN_POINT ( 'NONE',  ( 20.32499999999999929, 6.123233995736764310E-16, -4.999999999999998224 ) ) ;
#72686 = ORIENTED_EDGE ( 'NONE', *, *, #40409, .F. ) ;
#72687 = CARTESIAN_POINT ( 'NONE',  ( 28.16249999999999787, 2.886751345948126879, 4.999999999999999112 ) ) ;
#72688 = CARTESIAN_POINT ( 'NONE',  ( 29.10937500061451644, -4.541064518000417216, -2.621784821875001281 ) ) ;
#72689 = VERTEX_POINT ( 'NONE', #71912 ) ;
#72690 = CARTESIAN_POINT ( 'NONE',  ( 18.81562500061452070, 3.027376345333613106, -5.243569643749998122 ) ) ;
#72691 = CARTESIAN_POINT ( 'NONE',  ( 7.228125000614517681, 4.541064518000418104, 2.621784821874999949 ) ) ;
#72692 = CARTESIAN_POINT ( 'NONE',  ( 21.23437500061451644, -2.746126346562646425, 4.756430356249996549 ) ) ;
#72693 = CARTESIAN_POINT ( 'NONE',  ( 5.221875000614519813, -6.054752690667223547, -1.112240025338166033E-15 ) ) ;
#72694 = CARTESIAN_POINT ( 'NONE',  ( 16.87500000122903288, 2.886751345948129099, -4.999999999999998224 ) ) ;
#72695 = CARTESIAN_POINT ( 'NONE',  ( 1.071796769724491893, 13.83259618943233527, -26.00000000000000355 ) ) ;
#72696 = CARTESIAN_POINT ( 'NONE',  ( 6.009375000614519458, 0.000000000000000000, 5.243569643749999010 ) ) ;
#72697 = CARTESIAN_POINT ( 'NONE',  ( 12.23437500061451821, 4.541064518000418104, 2.621784821874999949 ) ) ;
#72698 = CARTESIAN_POINT ( 'NONE',  ( 20.63437500061451857, 6.421520780324663323E-16, -5.243569643749999010 ) ) ;
#72699 = CARTESIAN_POINT ( 'NONE',  ( 4.494741915665277254, -2.190272839526016924, 4.494741915664858922 ) ) ;
#72700 = ORIENTED_EDGE ( 'NONE', *, *, #68253, .F. ) ;
#72701 = CARTESIAN_POINT ( 'NONE',  ( 11.36250000000000071, 2.886751345948129099, -4.999999999999998224 ) ) ;
#72702 = CARTESIAN_POINT ( 'NONE',  ( 6.084375000614518747, -4.541064518000419881, 2.621784821874995952 ) ) ;
#72703 = CARTESIAN_POINT ( 'NONE',  ( -1.878215178124999163, 14.59062499938548463, 26.74683588394047007 ) ) ;
#72704 = CARTESIAN_POINT ( 'NONE',  ( 22.12500000000000000, 6.123233995736764310E-16, -4.999999999999998224 ) ) ;
#72705 = CARTESIAN_POINT ( 'NONE',  ( 17.76562500061451644, -6.054752690667223547, -1.112240025338166033E-15 ) ) ;
#72706 = CARTESIAN_POINT ( 'NONE',  ( -4.000000000000000000, 18.12500000000000355, 30.00000000000000000 ) ) ;
#72707 = CARTESIAN_POINT ( 'NONE',  ( -2.121784821874996840, 10.93437500061451928, -26.32496088578401583 ) ) ;
#72708 = CARTESIAN_POINT ( 'NONE',  ( 21.23437500061451644, 4.119189519843966529, 2.378215178124999607 ) ) ;
#72709 = CARTESIAN_POINT ( 'NONE',  ( 11.50312500061451892, -4.541064518000417216, -2.621784821875001281 ) ) ;
#72710 = CARTESIAN_POINT ( 'NONE',  ( 29.48437500061451644, -4.541064518000419881, 2.621784821874995952 ) ) ;
#72711 = DIRECTION ( 'NONE',  ( 0.000000000000000000, 0.000000000000000000, 1.000000000000000000 ) ) ;
#72712 = CARTESIAN_POINT ( 'NONE',  ( 29.63437500061451502, 6.421520780324663323E-16, -5.243569643749999010 ) ) ;
#72713 = CARTESIAN_POINT ( 'NONE',  ( 10.01250000000000107, 2.886751345948129099, -4.999999999999998224 ) ) ;
#72714 = CARTESIAN_POINT ( 'NONE',  ( -1.999999999999997113, 15.68750000122903465, 33.46410161513775705 ) ) ;
#72715 = CARTESIAN_POINT ( 'NONE',  ( 8.587500001229035007, -4.330127018922194537, 2.499999999999995559 ) ) ;
#72716 = CARTESIAN_POINT ( 'NONE',  ( 20.85937500061451644, 0.000000000000000000, 5.243569643749999010 ) ) ;
#72717 = CARTESIAN_POINT ( 'NONE',  ( 13.24687500061451750, -3.027376345333614438, 5.243569643749998122 ) ) ;
#72718 = CARTESIAN_POINT ( 'NONE',  ( 1.592000809091587073E-14, 16.85000000122903785, 26.00000000000000000 ) ) ;
#72719 = VERTEX_POINT ( 'NONE', #10580 ) ;
#72720 = CARTESIAN_POINT ( 'NONE',  ( 14.09062500061451750, -3.027376345333614438, 5.243569643749998122 ) ) ;
#72721 = CARTESIAN_POINT ( 'NONE',  ( 26.51250000122903216, 0.000000000000000000, 4.999999999999998224 ) ) ;
#72722 = CARTESIAN_POINT ( 'NONE',  ( 14.89687500061451786, 6.054752690667223547, 3.707466751127219781E-16 ) ) ;
#72723 = CARTESIAN_POINT ( 'NONE',  ( 3.979525575715637586, 9.178911176227741109, -25.49336387293115180 ) ) ;
#72724 = CARTESIAN_POINT ( 'NONE',  ( 16.15312500061451573, 4.541064518000418104, -2.621784821874998173 ) ) ;
#72725 = CARTESIAN_POINT ( 'NONE',  ( 0.000000000000000000, 0.000000000000000000, 50.00000000000000000 ) ) ;
#72726 = CARTESIAN_POINT ( 'NONE',  ( 26.29687500061451644, -3.027376345333614438, 5.243569643749998122 ) ) ;
#72727 = CARTESIAN_POINT ( 'NONE',  ( 2.121784821874999061, 10.20312500061451821, 26.32496088578401583 ) ) ;
#72728 = CARTESIAN_POINT ( 'NONE',  ( 15.08437500061451786, -4.541064518000419881, 2.621784821874995952 ) ) ;
#72729 = CARTESIAN_POINT ( 'NONE',  ( 14.28750000122903430, 4.330127018922191873, 2.499999999999999556 ) ) ;
#72730 = CARTESIAN_POINT ( 'NONE',  ( 8.971875000614515372, 2.746126346562645981, -4.756430356249997438 ) ) ;
#72731 = CARTESIAN_POINT ( 'NONE',  ( 19.43437500061451928, 4.541064518000418104, 2.621784821874999949 ) ) ;
#72732 = CARTESIAN_POINT ( 'NONE',  ( 20.70000000122903216, -2.886751345948129988, 4.999999999999997335 ) ) ;
#72733 = CARTESIAN_POINT ( 'NONE',  ( 17.52187500061451431, 3.027376345333613106, -5.243569643749998122 ) ) ;
#72734 = CARTESIAN_POINT ( 'NONE',  ( -4.243569643749999898, 12.65937500061451715, 30.00000000000000000 ) ) ;
#72735 = VECTOR ( 'NONE', #60658, 1000.000000000000000 ) ;
#72736 = CARTESIAN_POINT ( 'NONE',  ( 17.76562500061451644, -6.054752690667223547, -1.112240025338166033E-15 ) ) ;
#72737 = ORIENTED_EDGE ( 'NONE', *, *, #66497, .T. ) ;
#72738 = ORIENTED_EDGE ( 'NONE', *, *, #1197, .F. ) ;
#72739 = CARTESIAN_POINT ( 'NONE',  ( 19.53749999999999432, 5.773502691896255534, 3.535250795749688894E-16 ) ) ;
#72740 = DIRECTION ( 'NONE',  ( 0.000000000000000000, 0.000000000000000000, 1.000000000000000000 ) ) ;
#72741 = CARTESIAN_POINT ( 'NONE',  ( 23.61562500061451431, -6.054752690667223547, -1.112240025338166033E-15 ) ) ;
#72742 = CARTESIAN_POINT ( 'NONE',  ( 4.490625000614516971, 6.054752690667223547, 3.707466751127219781E-16 ) ) ;
#72743 = EDGE_CURVE ( 'NONE', #27832, #55926, #12765, .T. ) ;
#72744 = CARTESIAN_POINT ( 'NONE',  ( 16.27500000122903501, -5.773502691896255534, -1.060575238724906372E-15 ) ) ;
#72745 = CARTESIAN_POINT ( 'NONE',  ( 22.79062500061451502, -3.027376345333610441, -5.243569643749999898 ) ) ;
#72746 = CARTESIAN_POINT ( 'NONE',  ( 21.56250000000000000, -5.773502691896255534, -1.060575238724906372E-15 ) ) ;
#72747 = CARTESIAN_POINT ( 'NONE',  ( 25.22812500061451502, 4.541064518000418104, 2.621784821874999949 ) ) ;
#72748 = CARTESIAN_POINT ( 'NONE',  ( 5.803125000614517859, 4.541064518000418104, -2.621784821874998173 ) ) ;
#72749 = ORIENTED_EDGE ( 'NONE', *, *, #23832, .F. ) ;
#72750 = CARTESIAN_POINT ( 'NONE',  ( 29.28749999999999787, -2.886751345948125991, -5.000000000000000000 ) ) ;
#72751 = CARTESIAN_POINT ( 'NONE',  ( 17.25000000000000000, 4.330127018922192761, -2.499999999999997780 ) ) ;
#72752 = CARTESIAN_POINT ( 'NONE',  ( 12.34687500061452070, -2.746126346562646425, 4.756430356249996549 ) ) ;
#72753 = CARTESIAN_POINT ( 'NONE',  ( 23.25000000000000000, 0.000000000000000000, 4.999999999999998224 ) ) ;
#72754 = CARTESIAN_POINT ( 'NONE',  ( 1.999999999999998668, 12.31250000122903465, -33.46410161513775705 ) ) ;
#72755 = CARTESIAN_POINT ( 'NONE',  ( -2.121784821874999949, 17.53437500061451715, -33.67503911421598417 ) ) ;
#72756 = CARTESIAN_POINT ( 'NONE',  ( 8.362500000000002487, 2.886751345948126879, 4.999999999999999112 ) ) ;
#72757 = CARTESIAN_POINT ( 'NONE',  ( 5.962500001229033231, -4.330127018922190985, -2.500000000000001332 ) ) ;
#72758 = CARTESIAN_POINT ( 'NONE',  ( 11.89687500061451608, -3.027376345333614438, 5.243569643749998122 ) ) ;
#72759 = CARTESIAN_POINT ( 'NONE',  ( 24.60000000122903430, 5.773502691896255534, 3.535250795749688401E-16 ) ) ;
#72760 = CARTESIAN_POINT ( 'NONE',  ( 4.584375000614516971, 4.541064518000418104, 2.621784821874999949 ) ) ;
#72761 = CARTESIAN_POINT ( 'NONE',  ( 13.01250000122903394, 0.000000000000000000, 4.999999999999998224 ) ) ;
#72762 = VECTOR ( 'NONE', #5058, 1000.000000000000000 ) ;
#72763 = CYLINDRICAL_SURFACE ( 'NONE', #54826, 4.000000000000000000 ) ;
#72764 = CARTESIAN_POINT ( 'NONE',  ( 10.28437500061451715, 6.421520780324663323E-16, -5.243569643749999010 ) ) ;
#72765 = CARTESIAN_POINT ( 'NONE',  ( 4.000000000000000000, 14.00000000122903465, -27.69059892324149885 ) ) ;
#72766 = CARTESIAN_POINT ( 'NONE',  ( 20.24062500061451431, 6.054752690667223547, 3.707466751127219781E-16 ) ) ;
#72767 = CARTESIAN_POINT ( 'NONE',  ( 16.53750000000000142, -2.886751345948130876, 4.999999999999996447 ) ) ;
#72768 = CARTESIAN_POINT ( 'NONE',  ( -4.243569643749999898, 18.41562500061459318, 27.54997392385601529 ) ) ;
#72769 = CARTESIAN_POINT ( 'NONE',  ( 23.14687500061451786, -3.027376345333614438, 5.243569643749998122 ) ) ;
#72770 = CARTESIAN_POINT ( 'NONE',  ( 7.320879633048903241E-15, 17.63749999999999574, 26.00000000000000355 ) ) ;
#72771 = ADVANCED_FACE ( 'NONE', ( #20182 ), #27577, .F. ) ;
#72772 = CARTESIAN_POINT ( 'NONE',  ( 28.61250000122903359, 4.330127018922192761, -2.499999999999997780 ) ) ;
#72773 = CARTESIAN_POINT ( 'NONE',  ( 21.12187500061451217, 4.119189519843966529, 2.378215178124999607 ) ) ;
#72774 = CARTESIAN_POINT ( 'NONE',  ( 24.66562500061451502, 3.027376345333613106, -5.243569643749998122 ) ) ;
#72775 = CARTESIAN_POINT ( 'NONE',  ( 16.71562500061451573, 3.027376345333611329, 5.243569643749999010 ) ) ;
#72776 = CARTESIAN_POINT ( 'NONE',  ( 13.10625000122903394, -4.330127018922190985, -2.500000000000001332 ) ) ;
#72777 = CARTESIAN_POINT ( 'NONE',  ( 13.20937500061451786, 0.000000000000000000, 5.243569643749999010 ) ) ;
#72778 = CARTESIAN_POINT ( 'NONE',  ( 7.434375000614515727, -2.746126346562641984, -4.756430356249999214 ) ) ;
#72779 = AXIS2_PLACEMENT_3D ( 'NONE', #7245, #7599, #2076 ) ;
#72780 = CARTESIAN_POINT ( 'NONE',  ( 24.11250000122903359, 4.330127018922192761, -2.499999999999997780 ) ) ;
#72781 = DIRECTION ( 'NONE',  ( -0.000000000000000000, -1.000000000000000000, -0.000000000000000000 ) ) ;
#72782 = CARTESIAN_POINT ( 'NONE',  ( 13.09687500061451892, 6.054752690667223547, 3.707466751127219781E-16 ) ) ;
#72783 = DIRECTION ( 'NONE',  ( 1.000000000000000000, 0.000000000000000000, 0.000000000000000000 ) ) ;
#72784 = CARTESIAN_POINT ( 'NONE',  ( 3.112500000000000711, -5.773502691896255534, -1.060575238724906372E-15 ) ) ;
#72785 = CARTESIAN_POINT ( 'NONE',  ( 1.626862140677534273E-15, 12.12500000122903465, 34.00000000000000000 ) ) ;
#72786 = CARTESIAN_POINT ( 'NONE',  ( 24.83437500061451431, 4.541064518000418104, 2.621784821874999949 ) ) ;
#72787 = CARTESIAN_POINT ( 'NONE',  ( 17.70937500061451431, 0.000000000000000000, 5.243569643749999010 ) ) ;
#72788 = CARTESIAN_POINT ( 'NONE',  ( -3.756430356250001434, 16.16562499938548569, 32.16877607737301048 ) ) ;
#72789 = CARTESIAN_POINT ( 'NONE',  ( 28.94999999999999929, 4.330127018922192761, -2.499999999999997780 ) ) ;
#72790 = CARTESIAN_POINT ( 'NONE',  ( 3.600000001229033408, -2.886751345948129988, 4.999999999999997335 ) ) ;
#72791 = CARTESIAN_POINT ( 'NONE',  ( 5.812500000000001776, -5.773502691896255534, -1.060575238724906372E-15 ) ) ;
#72792 = CARTESIAN_POINT ( 'NONE',  ( 29.07187500061451502, -5.492252693125287522, -1.008910452111647106E-15 ) ) ;
#72793 = CARTESIAN_POINT ( 'NONE',  ( 20.01562500061451644, -6.054752690667223547, -1.112240025338166033E-15 ) ) ;
#72794 = CARTESIAN_POINT ( 'NONE',  ( 9.637499999999999289, 5.773502691896255534, 3.535250795749688894E-16 ) ) ;
#72795 = PLANE ( 'NONE',  #5419 ) ;
#72796 = CARTESIAN_POINT ( 'NONE',  ( 16.87500000000000000, 4.330127018922191873, 2.499999999999999556 ) ) ;
#72797 = CARTESIAN_POINT ( 'NONE',  ( -2.121784821874996840, 11.77812500061451750, 33.67503911421598417 ) ) ;
#72798 = CARTESIAN_POINT ( 'NONE',  ( 14.55000000000000071, 4.330127018922192761, -2.499999999999997780 ) ) ;
#72799 = CARTESIAN_POINT ( 'NONE',  ( 19.76250000122903216, 0.000000000000000000, 4.999999999999998224 ) ) ;
#72800 = DIRECTION ( 'NONE',  ( -1.000000000000000000, -0.000000000000000000, -0.000000000000000000 ) ) ;
#72801 = CARTESIAN_POINT ( 'NONE',  ( 27.38437500061451857, 6.421520780324663323E-16, -5.243569643749999010 ) ) ;
#72802 = ORIENTED_EDGE ( 'NONE', *, *, #36502, .F. ) ;
#72803 = CARTESIAN_POINT ( 'NONE',  ( 16.90312500061451573, -4.541064518000417216, -2.621784821875001281 ) ) ;
#72804 = CARTESIAN_POINT ( 'NONE',  ( 21.92812500061451431, 6.421520780324663323E-16, -5.243569643749999010 ) ) ;
#72805 = CARTESIAN_POINT ( 'NONE',  ( 23.25937500061451857, -4.541064518000417216, -2.621784821875001281 ) ) ;
#72806 = CARTESIAN_POINT ( 'NONE',  ( 7.087499999999999467, -2.886751345948129988, 4.999999999999997335 ) ) ;
#72807 = CARTESIAN_POINT ( 'NONE',  ( 10.67812500061451608, 6.421520780324663323E-16, -5.243569643749999010 ) ) ;
#72808 = CARTESIAN_POINT ( 'NONE',  ( 25.41562500061451146, -6.054752690667223547, -1.112240025338166033E-15 ) ) ;
#72809 = CARTESIAN_POINT ( 'NONE',  ( 13.92187500061451644, 3.027376345333613106, -5.243569643749998122 ) ) ;
#72810 = CARTESIAN_POINT ( 'NONE',  ( 19.09687500061451360, -3.027376345333614438, 5.243569643749998122 ) ) ;
#72811 = CARTESIAN_POINT ( 'NONE',  ( 1.999999999999998668, 12.31250000122903465, -33.46410161513775705 ) ) ;
#72812 = CARTESIAN_POINT ( 'NONE',  ( 4.243569643749999898, 11.08437500061451786, 30.00000000000000000 ) ) ;
#72813 = CARTESIAN_POINT ( 'NONE',  ( 20.96250000122903145, 4.330127018922192761, -2.499999999999997780 ) ) ;
#72814 = CARTESIAN_POINT ( 'NONE',  ( 16.24687500061451573, 5.492252693125287522, 3.363034840372157021E-16 ) ) ;
#72815 = CARTESIAN_POINT ( 'NONE',  ( 12.47812500061451502, 6.421520780324663323E-16, -5.243569643749999010 ) ) ;
#72816 = CARTESIAN_POINT ( 'NONE',  ( 5.859375000614519102, 4.541064518000418104, -2.621784821874998173 ) ) ;
#72817 = CARTESIAN_POINT ( 'NONE',  ( 6.234375000614519102, 6.421520780324663323E-16, -5.243569643749999010 ) ) ;
#72818 = ORIENTED_EDGE ( 'NONE', *, *, #10883, .T. ) ;
#72819 = CARTESIAN_POINT ( 'NONE',  ( 28.73437500061451644, 6.421520780324663323E-16, -5.243569643749999010 ) ) ;
#72820 = CARTESIAN_POINT ( 'NONE',  ( 18.51562500061451289, 3.027376345333611329, 5.243569643749999010 ) ) ;
#72821 = CARTESIAN_POINT ( 'NONE',  ( 28.72500000122903074, 2.886751345948126879, 4.999999999999999112 ) ) ;
#72822 = CARTESIAN_POINT ( 'NONE',  ( 27.06562500061451004, 3.027376345333611329, 5.243569643749999010 ) ) ;
#72823 = CARTESIAN_POINT ( 'NONE',  ( 23.82187500061451502, 3.027376345333613106, -5.243569643749998122 ) ) ;
#72824 = CARTESIAN_POINT ( 'NONE',  ( 18.85312500061451502, 4.541064518000418104, -2.621784821874998173 ) ) ;
#72825 = CARTESIAN_POINT ( 'NONE',  ( 8.484601909799253346E-16, 10.21250000000000213, 34.61880215351700230 ) ) ;
#72826 = CARTESIAN_POINT ( 'NONE',  ( 24.32812500061451289, 4.541064518000418104, 2.621784821874999949 ) ) ;
#72827 = CARTESIAN_POINT ( 'NONE',  ( 5.662500001229035185, 4.330127018922192761, -2.499999999999997780 ) ) ;
#72828 = ORIENTED_EDGE ( 'NONE', *, *, #60362, .T. ) ;
#72829 = CARTESIAN_POINT ( 'NONE',  ( 27.82499999999999929, -4.330127018922194537, 2.499999999999995559 ) ) ;
#72830 = CARTESIAN_POINT ( 'NONE',  ( -3.999999999999999556, 16.36250000000000071, -32.30940107675850470 ) ) ;
#72831 = CARTESIAN_POINT ( 'NONE',  ( 1.878215178124997609, 17.17812499938548498, 33.25316411605952993 ) ) ;
#72832 = CARTESIAN_POINT ( 'NONE',  ( 4.659375000614518925, 0.000000000000000000, 5.243569643749999010 ) ) ;
#72833 = CARTESIAN_POINT ( 'NONE',  ( 12.25312500061451537, 0.000000000000000000, 5.243569643749999010 ) ) ;
#72834 = CARTESIAN_POINT ( 'NONE',  ( 6.909375000614518036, 0.000000000000000000, 5.243569643749999010 ) ) ;
#72835 = CARTESIAN_POINT ( 'NONE',  ( 25.08750000122903145, 4.330127018922191873, 2.499999999999999556 ) ) ;
#72836 = VECTOR ( 'NONE', #69001, 1000.000000000000000 ) ;
#72837 = CARTESIAN_POINT ( 'NONE',  ( 15.19687500061451679, -3.027376345333610441, -5.243569643749999898 ) ) ;
#72838 = CARTESIAN_POINT ( 'NONE',  ( 29.12812500061451715, 6.421520780324663323E-16, -5.243569643749999010 ) ) ;
#72839 = CARTESIAN_POINT ( 'NONE',  ( 28.94999999999999929, 4.330127018922192761, -2.499999999999997780 ) ) ;
#72840 = CARTESIAN_POINT ( 'NONE',  ( 25.47187500061451715, -6.054752690667223547, -1.112240025338166033E-15 ) ) ;
#72841 = CARTESIAN_POINT ( 'NONE',  ( 2.915625000614516793, -6.054752690667223547, -1.112240025338166033E-15 ) ) ;
#72842 = CARTESIAN_POINT ( 'NONE',  ( 12.74062500061451786, -3.027376345333614438, 5.243569643749998122 ) ) ;
#72843 =( BOUNDED_CURVE ( )  B_SPLINE_CURVE ( 2, ( #66308, #38223, #11254, #21965, #50420, #21597, #10524 ),
 .UNSPECIFIED., .F., .F. ) 
 B_SPLINE_CURVE_WITH_KNOTS ( ( 3, 2, 2, 3 ),
 ( 0.9166666666666666297, 0.9194444444444443976, 0.9222222222222221655, 0.9249999999999999334 ),
 .UNSPECIFIED. ) 
 CURVE ( )  GEOMETRIC_REPRESENTATION_ITEM ( )  RATIONAL_B_SPLINE_CURVE ( ( 1.000000000000000000, 0.8660254037844387076, 1.000000000000000000, 0.8660254037844387076, 1.000000000000000000, 0.8660254037844440367, 0.9999999999999946709 ) ) 
 REPRESENTATION_ITEM ( '' )  );
#72844 = EDGE_LOOP ( 'NONE', ( #4435, #64040, #22693, #37239 ) ) ;
#72845 = CARTESIAN_POINT ( 'NONE',  ( 10.49062500061451431, -3.027376345333614438, 5.243569643749998122 ) ) ;
#72846 = CARTESIAN_POINT ( 'NONE',  ( 7.790625000614518569, -3.027376345333614438, 5.243569643749998122 ) ) ;
#72847 = CARTESIAN_POINT ( 'NONE',  ( 18.72187500061451360, -5.492252693125287522, -1.008910452111647106E-15 ) ) ;
#72848 = DIRECTION ( 'NONE',  ( -0.000000000000000000, -1.000000000000000000, -0.000000000000000000 ) ) ;
#72849 = CARTESIAN_POINT ( 'NONE',  ( 16.19999999999999929, -4.330127018922190985, -2.500000000000001332 ) ) ;
#72850 = CARTESIAN_POINT ( 'NONE',  ( 15.68437500061451573, 6.421520780324663323E-16, -5.243569643749999010 ) ) ;
#72851 = CARTESIAN_POINT ( 'NONE',  ( 14.47500000122903430, -5.773502691896255534, -1.060575238724906372E-15 ) ) ;
#72852 = CARTESIAN_POINT ( 'NONE',  ( 19.23749999999999716, -2.886751345948129988, 4.999999999999997335 ) ) ;
#72853 = CARTESIAN_POINT ( 'NONE',  ( 21.15937500061451715, 4.541064518000418104, -2.621784821874998173 ) ) ;
#72854 = CARTESIAN_POINT ( 'NONE',  ( -2.121784821874999949, 13.87812500061451715, -33.67503911421598417 ) ) ;
#72855 = CARTESIAN_POINT ( 'NONE',  ( 21.44999999999999929, 0.000000000000000000, 4.999999999999998224 ) ) ;
#72856 = CARTESIAN_POINT ( 'NONE',  ( 25.02187500061451431, 5.824947211148865298E-16, -4.756430356249998326 ) ) ;
#72857 = CARTESIAN_POINT ( 'NONE',  ( 20.69999999999999929, -4.330127018922190985, -2.500000000000001332 ) ) ;
#72858 = CARTESIAN_POINT ( 'NONE',  ( 27.81562500061452070, 3.027376345333613106, -5.243569643749998122 ) ) ;
#72859 = CARTESIAN_POINT ( 'NONE',  ( -1.487416814333745711E-14, 16.06250000000000000, -26.00000000000000000 ) ) ;
#72860 = CARTESIAN_POINT ( 'NONE',  ( 27.75000000000000000, 0.000000000000000000, 4.999999999999998224 ) ) ;
#72861 = ADVANCED_FACE ( 'NONE', ( #66740 ), #42737, .F. ) ;
#72862 = CARTESIAN_POINT ( 'NONE',  ( 9.028125000614517504, 4.541064518000418104, 2.621784821874999949 ) ) ;
#72863 = CARTESIAN_POINT ( 'NONE',  ( 28.47187500061451715, -4.119189519843968306, 2.378215178124996054 ) ) ;
#72864 = CARTESIAN_POINT ( 'NONE',  ( 20.55937500061451573, -4.541064518000417216, -2.621784821875001281 ) ) ;
#72865 = CARTESIAN_POINT ( 'NONE',  ( 13.73437500061451289, -2.746126346562641984, -4.756430356249999214 ) ) ;
#72866 = CARTESIAN_POINT ( 'NONE',  ( 4.978125000614518569, 4.541064518000418104, 2.621784821874999949 ) ) ;
#72867 = CARTESIAN_POINT ( 'NONE',  ( 10.50937500061451679, 0.000000000000000000, 5.243569643749999010 ) ) ;
#72868 = ORIENTED_EDGE ( 'NONE', *, *, #66396, .T. ) ;
#72869 = CARTESIAN_POINT ( 'NONE',  ( 21.60937500061451644, 4.541064518000418104, -2.621784821874998173 ) ) ;
#72870 = CARTESIAN_POINT ( 'NONE',  ( 1.347985686992486443, 4.821799686897913162, -26.22451506405455390 ) ) ;
#72871 = CARTESIAN_POINT ( 'NONE',  ( 28.64999999999999858, 0.000000000000000000, 4.999999999999998224 ) ) ;
#72872 = CARTESIAN_POINT ( 'NONE',  ( 4.500000000000000888, -4.330127018922190985, -2.500000000000001332 ) ) ;
#72873 = AXIS2_PLACEMENT_3D ( 'NONE', #41292, #1411, #47551 ) ;
#72874 = CARTESIAN_POINT ( 'NONE',  ( 14.88750000122903394, -4.330127018922194537, 2.499999999999995559 ) ) ;
#72875 = CARTESIAN_POINT ( 'NONE',  ( 18.13125000122903074, 6.123233995736764310E-16, -4.999999999999998224 ) ) ;
#72876 = CARTESIAN_POINT ( 'NONE',  ( 19.20000000000000284, 0.000000000000000000, 4.999999999999998224 ) ) ;
#72877 = ORIENTED_EDGE ( 'NONE', *, *, #9144, .T. ) ;
#72878 = CARTESIAN_POINT ( 'NONE',  ( 13.83749999999999858, -2.886751345948129988, 4.999999999999997335 ) ) ;
#72879 = CARTESIAN_POINT ( 'NONE',  ( 26.35312500061451857, -4.541064518000417216, -2.621784821875001281 ) ) ;
#72880 = CARTESIAN_POINT ( 'NONE',  ( 17.39999999999999858, 0.000000000000000000, 4.999999999999998224 ) ) ;
#72881 = CARTESIAN_POINT ( 'NONE',  ( 9.825000001229033941, 2.886751345948126879, 4.999999999999999112 ) ) ;
#72882 = CARTESIAN_POINT ( 'NONE',  ( 9.665625000614515017, -6.054752690667223547, -1.112240025338166033E-15 ) ) ;
#72883 = AXIS2_PLACEMENT_3D ( 'NONE', #65482, #44059, #32964 ) ;
#72884 = CARTESIAN_POINT ( 'NONE',  ( 9.562500000000001776, 2.886751345948129099, -4.999999999999998224 ) ) ;
#72885 = CARTESIAN_POINT ( 'NONE',  ( 18.41250000122903430, 0.000000000000000000, 4.999999999999998224 ) ) ;
#72886 = CARTESIAN_POINT ( 'NONE',  ( -4.243569643749999898, 15.35937500061451644, -30.00000000000000000 ) ) ;
#72887 = CARTESIAN_POINT ( 'NONE',  ( 27.63750000122903216, 6.123233995736764310E-16, -4.999999999999998224 ) ) ;
#72888 = CARTESIAN_POINT ( 'NONE',  ( 1.878215178125000495, 15.41562499938548392, 26.74683588394047007 ) ) ;
#72889 = CARTESIAN_POINT ( 'NONE',  ( 7.500000000000000000, 0.000000000000000000, 4.999999999999998224 ) ) ;
#72890 = CARTESIAN_POINT ( 'NONE',  ( -3.999999999999997335, 12.83750000000000213, 32.30940107675850470 ) ) ;
#72891 = EDGE_LOOP ( 'NONE', ( #63403, #46209 ) ) ;
#72892 = CARTESIAN_POINT ( 'NONE',  ( 24.02812500061451573, -4.541064518000419881, 2.621784821874995952 ) ) ;
#72893 = CARTESIAN_POINT ( 'NONE',  ( 4.080569135018654592, -2.889455923578380769, -4.080569135022440896 ) ) ;
#72894 = CARTESIAN_POINT ( 'NONE',  ( 21.19687500061451502, 6.054752690667223547, 3.707466751127219781E-16 ) ) ;
#72895 = CARTESIAN_POINT ( 'NONE',  ( 15.74062500061451608, 6.054752690667223547, 3.707466751127219781E-16 ) ) ;
#72896 = CARTESIAN_POINT ( 'NONE',  ( 2.121784821875001281, 11.40312500061459389, -26.32496088578401938 ) ) ;
#72897 = CARTESIAN_POINT ( 'NONE',  ( 7.040625000614517681, -3.027376345333610441, -5.243569643749999898 ) ) ;
#72898 = CARTESIAN_POINT ( 'NONE',  ( 28.61250000122903359, 4.330127018922192761, -2.499999999999997780 ) ) ;
#72899 = CARTESIAN_POINT ( 'NONE',  ( 23.70937500061451786, -4.119189519843965641, -2.378215178125001383 ) ) ;
#72900 = CARTESIAN_POINT ( 'NONE',  ( 19.49062500061451786, -3.027376345333614438, 5.243569643749998122 ) ) ;
#72901 = CARTESIAN_POINT ( 'NONE',  ( 3.999999999999999112, 11.33750000122903501, -30.00000000000000000 ) ) ;
#72902 = CARTESIAN_POINT ( 'NONE',  ( 2.655984681222220721E-16, 19.50312499938548427, 25.66244784525396483 ) ) ;
#72903 = CARTESIAN_POINT ( 'NONE',  ( 15.19687500061451857, -3.027376345333610441, -5.243569643749999898 ) ) ;
#72904 = CARTESIAN_POINT ( 'NONE',  ( 14.10937500061451644, 0.000000000000000000, 5.243569643749999010 ) ) ;
#72905 = CARTESIAN_POINT ( 'NONE',  ( 23.03437500061451715, 4.541064518000418104, 2.621784821874999949 ) ) ;
#72906 = VERTEX_POINT ( 'NONE', #38280 ) ;
#72907 = CARTESIAN_POINT ( 'NONE',  ( 3.028125000614518392, 6.421520780324663323E-16, -5.243569643749999010 ) ) ;
#72908 = CARTESIAN_POINT ( 'NONE',  ( 26.24062500061451431, -3.027376345333614438, 5.243569643749998122 ) ) ;
#72909 = CARTESIAN_POINT ( 'NONE',  ( 25.71562500061451573, 3.027376345333611329, 5.243569643749999010 ) ) ;
#72910 = CARTESIAN_POINT ( 'NONE',  ( 7.631250001229033408, -4.330127018922194537, 2.499999999999995559 ) ) ;
#72911 = CARTESIAN_POINT ( 'NONE',  ( -3.999999999999999556, 16.36250000000000071, 27.69059892324149530 ) ) ;
#72912 = CARTESIAN_POINT ( 'NONE',  ( 5.071875000614519458, 3.027376345333611329, 5.243569643749999010 ) ) ;
#72913 = CARTESIAN_POINT ( 'NONE',  ( 11.28750000122903252, -4.330127018922194537, 2.499999999999995559 ) ) ;
#72914 = CARTESIAN_POINT ( 'NONE',  ( 7.912500001229033408, 4.330127018922192761, -2.499999999999997780 ) ) ;
#72915 = CARTESIAN_POINT ( 'NONE',  ( 29.21250000122903145, 0.000000000000000000, 4.999999999999998224 ) ) ;
#72916 = CARTESIAN_POINT ( 'NONE',  ( 3.999999999999998668, 17.35624999877096641, 32.30940107675850470 ) ) ;
#72917 = CARTESIAN_POINT ( 'NONE',  ( 18.46875000122902932, -5.773502691896255534, -1.060575238724906372E-15 ) ) ;
#72918 = CARTESIAN_POINT ( 'NONE',  ( 11.10937500061451644, -4.541064518000417216, -2.621784821875001281 ) ) ;
#72919 = CARTESIAN_POINT ( 'NONE',  ( -2.000000000000001776, 17.69374999877096855, 33.46410161513775705 ) ) ;
#72920 = EDGE_LOOP ( 'NONE', ( #32950, #13381, #68447, #8572 ) ) ;
#72921 = CARTESIAN_POINT ( 'NONE',  ( 19.11562500061451431, -6.054752690667223547, -1.112240025338166033E-15 ) ) ;
#72922 = CARTESIAN_POINT ( 'NONE',  ( 13.92187500061451644, 3.027376345333613106, -5.243569643749998122 ) ) ;
#72923 = CARTESIAN_POINT ( 'NONE',  ( 4.415625000614518569, 3.027376345333613106, -5.243569643749998122 ) ) ;
#72924 = CARTESIAN_POINT ( 'NONE',  ( 22.58437500061451431, 4.541064518000418104, 2.621784821874999949 ) ) ;
#72925 = CARTESIAN_POINT ( 'NONE',  ( 10.39687500061451786, 6.054752690667223547, 3.707466751127219781E-16 ) ) ;
#72926 = CARTESIAN_POINT ( 'NONE',  ( 4.228125000614517681, -4.541064518000419881, 2.621784821874995952 ) ) ;
#72927 = CARTESIAN_POINT ( 'NONE',  ( 20.85000000000000142, 4.330127018922192761, -2.499999999999997780 ) ) ;
#72928 = CARTESIAN_POINT ( 'NONE',  ( 4.950000001229033941, -2.886751345948129988, 4.999999999999997335 ) ) ;
#72929 = CARTESIAN_POINT ( 'NONE',  ( 21.21562500061451573, 3.027376345333611329, 5.243569643749999010 ) ) ;
#72930 = CARTESIAN_POINT ( 'NONE',  ( 7.125000001229033764, 2.886751345948126879, 4.999999999999999112 ) ) ;
#72931 = CARTESIAN_POINT ( 'NONE',  ( 16.86562500061451786, -6.054752690667223547, -1.112240025338166033E-15 ) ) ;
#72932 = CARTESIAN_POINT ( 'NONE',  ( 14.87812500061451537, 4.541064518000418104, 2.621784821874999949 ) ) ;
#72933 = CARTESIAN_POINT ( 'NONE',  ( 24.90937500061451715, 0.000000000000000000, 4.756430356249998326 ) ) ;
#72934 = CARTESIAN_POINT ( 'NONE',  ( 15.41250000000000142, 2.886751345948129099, -4.999999999999998224 ) ) ;
#72935 = CARTESIAN_POINT ( 'NONE',  ( 9.975000001229034297, -5.773502691896255534, -1.060575238724906372E-15 ) ) ;
#72936 = VECTOR ( 'NONE', #39699, 1000.000000000000000 ) ;
#72937 = CARTESIAN_POINT ( 'NONE',  ( 5.428125000614517859, 4.541064518000418104, 2.621784821874999949 ) ) ;
#72938 = CARTESIAN_POINT ( 'NONE',  ( 19.98750000122903359, 6.123233995736764310E-16, -4.999999999999998224 ) ) ;
#72939 = CARTESIAN_POINT ( 'NONE',  ( 25.94999999999999929, 0.000000000000000000, 4.999999999999998224 ) ) ;
#72940 = CARTESIAN_POINT ( 'NONE',  ( 4.243569643749999898, 10.18437500061451750, -30.00000000000000000 ) ) ;
#72941 = CARTESIAN_POINT ( 'NONE',  ( 4.999999999999050537, 0.1750410927365727287, 5.155377002944480758 ) ) ;
#72942 = EDGE_CURVE ( 'NONE', #70914, #53615, #42973, .T. ) ;
#72943 = CARTESIAN_POINT ( 'NONE',  ( 24.11249999999999716, 2.886751345948161074, 4.999999999999941380 ) ) ;
#72944 = CARTESIAN_POINT ( 'NONE',  ( 3.196875000614516793, 6.054752690667223547, 3.707466751127219781E-16 ) ) ;
#72945 = CARTESIAN_POINT ( 'NONE',  ( 21.08437500061451786, 6.421520780324663323E-16, -5.243569643749999010 ) ) ;
#72946 = CARTESIAN_POINT ( 'NONE',  ( 12.26249999999999929, 2.886751345948062486, -5.000000000000113687 ) ) ;
#72947 = CARTESIAN_POINT ( 'NONE',  ( 17.57812500061451644, 4.541064518000418104, 2.621784821874999949 ) ) ;
#72948 = CARTESIAN_POINT ( 'NONE',  ( 12.76875000122903181, 2.886751345948129099, -4.999999999999998224 ) ) ;
#72949 = CARTESIAN_POINT ( 'NONE',  ( 23.06250000000000355, 2.886751345948162850, -4.999999999999940492 ) ) ;
#72950 = FACE_OUTER_BOUND ( 'NONE', #43189, .T. ) ;
#72951 = CARTESIAN_POINT ( 'NONE',  ( 28.77187500061451431, 3.027376345333613106, -5.243569643749998122 ) ) ;
#72952 = CARTESIAN_POINT ( 'NONE',  ( 19.65937500061451360, 2.746126346562645981, -4.756430356249997438 ) ) ;
#72953 = CARTESIAN_POINT ( 'NONE',  ( 11.72812500061451857, 4.541064518000418104, 2.621784821874999949 ) ) ;
#72954 = CARTESIAN_POINT ( 'NONE',  ( 11.18437500061451928, 6.421520780324663323E-16, -5.243569643749999010 ) ) ;
#72955 = EDGE_LOOP ( 'NONE', ( #11194, #16551 ) ) ;
#72956 = CARTESIAN_POINT ( 'NONE',  ( 28.71562500061451573, 3.027376345333613106, -5.243569643749998122 ) ) ;
#72957 = CARTESIAN_POINT ( 'NONE',  ( 22.07812500061451644, 4.541064518000418104, 2.621784821874999949 ) ) ;
#72958 = CARTESIAN_POINT ( 'NONE',  ( 1.626862140677534273E-15, 11.11250000000000071, -26.00000000000000355 ) ) ;
#72959 = CARTESIAN_POINT ( 'NONE',  ( 19.08750000122903145, 6.123233995736764310E-16, -4.999999999999998224 ) ) ;
#72960 = CARTESIAN_POINT ( 'NONE',  ( 11.43750000000000000, 5.773502691896255534, 3.535250795749688894E-16 ) ) ;
#72961 = CARTESIAN_POINT ( 'NONE',  ( 21.03750000122903074, 4.330127018922191873, 2.499999999999999556 ) ) ;
#72962 = CARTESIAN_POINT ( 'NONE',  ( 16.82812500061451644, -4.541064518000419881, 2.621784821874995952 ) ) ;
#72963 = CARTESIAN_POINT ( 'NONE',  ( 14.03437500061451892, -2.746126346562646425, 4.756430356249996549 ) ) ;
#72964 = ORIENTED_EDGE ( 'NONE', *, *, #54007, .T. ) ;
#72965 = CARTESIAN_POINT ( 'NONE',  ( 20.77500000000000213, 6.123233995736764310E-16, -4.999999999999998224 ) ) ;
#72966 = CARTESIAN_POINT ( 'NONE',  ( 23.36250000000000071, -5.773502691896255534, -1.060575238724906372E-15 ) ) ;
#72967 = CARTESIAN_POINT ( 'NONE',  ( 20.37187500061451573, 3.027376345333611329, 5.243569643749999010 ) ) ;
#72968 = CARTESIAN_POINT ( 'NONE',  ( 26.46562500061451573, 3.027376345333613106, -5.243569643749998122 ) ) ;
#72969 = VERTEX_POINT ( 'NONE', #37553 ) ;
#72970 = CARTESIAN_POINT ( 'NONE',  ( 21.24375000122903145, -2.886751345948126435, -5.000000000000000000 ) ) ;
#72971 = CARTESIAN_POINT ( 'NONE',  ( 7.828125000614517326, -4.541064518000419881, 2.621784821874995952 ) ) ;
#72972 = CARTESIAN_POINT ( 'NONE',  ( 3.347192403100067715, 3.714448376624780224, 3.458182559776492138 ) ) ;
#72973 = CARTESIAN_POINT ( 'NONE',  ( 16.38749999999999929, 5.773502691896255534, 3.535250795749688894E-16 ) ) ;
#72974 = CARTESIAN_POINT ( 'NONE',  ( 4.243569643749999010, 19.61562500061451431, 27.54997392385601174 ) ) ;
#72975 = CARTESIAN_POINT ( 'NONE',  ( 4.246875000614519280, -3.027376345333614438, 5.243569643749998122 ) ) ;
#72976 = CARTESIAN_POINT ( 'NONE',  ( 28.92187500061451644, 3.027376345333611329, 5.243569643749999010 ) ) ;
#72977 = ORIENTED_EDGE ( 'NONE', *, *, #38408, .F. ) ;
#72978 = CARTESIAN_POINT ( 'NONE',  ( 24.17812500061451786, 6.421520780324663323E-16, -5.243569643749999010 ) ) ;
#72979 = CARTESIAN_POINT ( 'NONE',  ( 25.50937500061451502, -4.541064518000417216, -2.621784821875001281 ) ) ;
#72980 = CARTESIAN_POINT ( 'NONE',  ( 2.121784821874999061, 19.65312500061459389, -33.67503911421598417 ) ) ;
#72981 = CARTESIAN_POINT ( 'NONE',  ( 12.44999999999999929, 0.000000000000000000, 4.999999999999998224 ) ) ;
#72982 = CARTESIAN_POINT ( 'NONE',  ( 8.653125000614515727, 0.000000000000000000, 5.243569643749999010 ) ) ;
#72983 = CARTESIAN_POINT ( 'NONE',  ( 4.898587196589411843E-16, 20.00000000000000000, -26.00000000000000000 ) ) ;
#72984 = CARTESIAN_POINT ( 'NONE',  ( 13.50000000000000178, -4.330127018922190985, -2.500000000000001332 ) ) ;
#72985 = CARTESIAN_POINT ( 'NONE',  ( 27.02812500061451573, 4.541064518000418104, 2.621784821874999949 ) ) ;
#72986 = CARTESIAN_POINT ( 'NONE',  ( 12.75000000122903465, -2.886751345948126435, -5.000000000000000000 ) ) ;
#72987 = CARTESIAN_POINT ( 'NONE',  ( 14.22187500061451537, -5.492252693125287522, -1.008910452111647106E-15 ) ) ;
#72988 = CARTESIAN_POINT ( 'NONE',  ( 3.290625000614516793, -3.027376345333614438, 5.243569643749998122 ) ) ;
#72989 = CARTESIAN_POINT ( 'NONE',  ( 19.13437500061451857, -4.541064518000419881, 2.621784821874995952 ) ) ;
#72991 = CARTESIAN_POINT ( 'NONE',  ( -4.243569643749999898, 14.90937500061451715, 30.00000000000000000 ) ) ;
#72990 =( BOUNDED_CURVE ( )  B_SPLINE_CURVE ( 2, ( #18170, #68094, #6753, #7836, #46275, #861, #1219 ),
 .UNSPECIFIED., .F., .F. ) 
 B_SPLINE_CURVE_WITH_KNOTS ( ( 3, 2, 2, 3 ),
 ( 0.01666666666666663174, 0.01944444444444440312, 0.02222222222222217797, 0.02499999999999994935 ),
 .UNSPECIFIED. ) 
 CURVE ( )  GEOMETRIC_REPRESENTATION_ITEM ( )  RATIONAL_B_SPLINE_CURVE ( ( 1.000000000000001554, 0.8660254037844370423, 1.000000000000000000, 0.8660254037844387076, 1.000000000000000000, 0.8660254037844412611, 0.9999999999999974465 ) ) 
 REPRESENTATION_ITEM ( '' )  );
#72992 = CARTESIAN_POINT ( 'NONE',  ( 21.72187500061451715, 3.027376345333611329, 5.243569643749999010 ) ) ;
#72993 = CARTESIAN_POINT ( 'NONE',  ( 3.225000000000002309, 6.123233995736764310E-16, -4.999999999999998224 ) ) ;
#72994 = CARTESIAN_POINT ( 'NONE',  ( 10.42500000000000071, 6.123233995736764310E-16, -4.999999999999998224 ) ) ;
#72995 = CARTESIAN_POINT ( 'NONE',  ( 9.440625000614517148, 6.054752690667223547, 3.707466751127219781E-16 ) ) ;
#72996 = CARTESIAN_POINT ( 'NONE',  ( 1.071796769724493892, 17.27990381179670010, 26.00000000000000711 ) ) ;
#72997 = CARTESIAN_POINT ( 'NONE',  ( 6.046875000614519102, -3.027376345333614438, 5.243569643749998122 ) ) ;
#72998 = CARTESIAN_POINT ( 'NONE',  ( 7.453125000614516438, -4.541064518000417216, -2.621784821875001281 ) ) ;
#72999 = CARTESIAN_POINT ( 'NONE',  ( 12.64687500061451608, 6.054752690667223547, 3.707466751127219781E-16 ) ) ;
#73000 = CARTESIAN_POINT ( 'NONE',  ( 19.38750000122903216, -4.330127018922194537, 2.499999999999995559 ) ) ;
#73001 = CARTESIAN_POINT ( 'NONE',  ( 8.221875000614518925, 3.027376345333611329, 5.243569643749999010 ) ) ;
#73002 = CARTESIAN_POINT ( 'NONE',  ( 9.215625000614515727, -6.054752690667223547, -1.112240025338166033E-15 ) ) ;
#73003 = CARTESIAN_POINT ( 'NONE',  ( 45.00000000000000000, 0.000000000000000000, 0.000000000000000000 ) ) ;
#73004 = CARTESIAN_POINT ( 'NONE',  ( 26.79375000122903216, 5.773502691896255534, 3.535250795749688894E-16 ) ) ;
#73005 = CARTESIAN_POINT ( 'NONE',  ( 18.12187500061451573, 3.027376345333611329, 5.243569643749999010 ) ) ;
#73006 = CARTESIAN_POINT ( 'NONE',  ( 18.26249999999999929, 2.886751345948126879, 4.999999999999998224 ) ) ;
#73007 = CARTESIAN_POINT ( 'NONE',  ( 28.19062500061451715, -3.027376345333610441, -5.243569643749999898 ) ) ;
#73008 = CARTESIAN_POINT ( 'NONE',  ( 11.05312500061451608, -4.541064518000417216, -2.621784821875001281 ) ) ;
#73009 = CARTESIAN_POINT ( 'NONE',  ( 28.20937500061451786, -4.541064518000417216, -2.621784821875001281 ) ) ;
#73010 = CARTESIAN_POINT ( 'NONE',  ( -3.000416591977282496E-16, 12.09687500061451892, -34.90005215228797653 ) ) ;
#73011 = CARTESIAN_POINT ( 'NONE',  ( 12.22500000122903430, -5.773502691896255534, -1.060575238724906372E-15 ) ) ;
#73012 = EDGE_CURVE ( 'NONE', #24228, #24506, #489, .T. ) ;
#73013 = CARTESIAN_POINT ( 'NONE',  ( 27.77812500061451573, 6.421520780324663323E-16, -5.243569643749999010 ) ) ;
#73014 = CARTESIAN_POINT ( 'NONE',  ( -4.243569643749997233, 16.24062500061451431, -27.54997392385601174 ) ) ;
#73015 = CARTESIAN_POINT ( 'NONE',  ( 15.97500000122903430, 2.886751345948129099, -4.999999999999998224 ) ) ;
#73016 = CARTESIAN_POINT ( 'NONE',  ( 12.41249999999999964, 2.886751345948126879, 4.999999999999999112 ) ) ;
#73017 = CARTESIAN_POINT ( 'NONE',  ( -3.999999999999999112, 13.70000000000000107, 30.00000000000000000 ) ) ;
#73018 = CARTESIAN_POINT ( 'NONE',  ( 22.64062500061451644, -3.027376345333614438, 5.243569643749998122 ) ) ;
#73019 = CARTESIAN_POINT ( 'NONE',  ( 7.546875000614515550, -3.027376345333610441, -5.243569643749999898 ) ) ;
#73020 = CARTESIAN_POINT ( 'NONE',  ( 8.100000001229034297, -2.886751345948129988, 4.999999999999997335 ) ) ;
#73021 = CARTESIAN_POINT ( 'NONE',  ( 16.23750000122903359, -4.330127018922194537, 2.499999999999995559 ) ) ;
#73022 = CARTESIAN_POINT ( 'NONE',  ( 13.75312500061451715, -4.541064518000417216, -2.621784821875001281 ) ) ;
#73023 = EDGE_CURVE ( 'NONE', #54151, #55851, #5041, .T. ) ;
#73024 = CARTESIAN_POINT ( 'NONE',  ( 17.35312500061451502, -4.541064518000417216, -2.621784821875001281 ) ) ;
#73025 = CARTESIAN_POINT ( 'NONE',  ( 25.05000000122903714, 5.773502691896255534, 3.535250795749688894E-16 ) ) ;
#73026 = CARTESIAN_POINT ( 'NONE',  ( 28.72500000122903074, 2.886751345948126879, 4.999999999999999112 ) ) ;
#73027 = CARTESIAN_POINT ( 'NONE',  ( 22.57499999999999929, 6.123233995736764310E-16, -4.999999999999998224 ) ) ;
#73028 = CARTESIAN_POINT ( 'NONE',  ( 25.62187500061451573, 3.027376345333613106, -5.243569643749998122 ) ) ;
#73029 = CYLINDRICAL_SURFACE ( 'NONE', #26425, 4.999999999999998224 ) ;
#73030 = CARTESIAN_POINT ( 'NONE',  ( 9.600000001229034297, -2.886751345948125991, -5.000000000000000000 ) ) ;
#73031 = CARTESIAN_POINT ( 'NONE',  ( 28.69687500061451502, -3.027376345333610441, -5.243569643749999898 ) ) ;
#73032 =( BOUNDED_CURVE ( )  B_SPLINE_CURVE ( 2, ( #36616, #28102, #10376, #5196, #39185, #22183, #55445, #49904, #21812 ),
 .UNSPECIFIED., .F., .F. ) 
 B_SPLINE_CURVE_WITH_KNOTS ( ( 3, 2, 2, 2, 3 ),
 ( 0.9456521739130434590, 0.9492753623188405765, 0.9565217391304348116, 0.9637681159420289356, 0.9662083058201528241 ),
 .UNSPECIFIED. ) 
 CURVE ( )  GEOMETRIC_REPRESENTATION_ITEM ( )  RATIONAL_B_SPLINE_CURVE ( ( 0.9330127018922194093, 0.9330127018922194093, 1.000000000000000000, 0.8660254037844387076, 1.000000000000000000, 0.8660254037844387076, 1.000000000000000000, 0.9548845634016894790, 0.9401540307620559478 ) ) 
 REPRESENTATION_ITEM ( '' )  );
#73033 = CARTESIAN_POINT ( 'NONE',  ( 6.084375000614518747, -4.541064518000419881, 2.621784821874995952 ) ) ;
#73034 = CARTESIAN_POINT ( 'NONE',  ( 22.56562500061451715, 3.027376345333611329, 5.243569643749999010 ) ) ;
#73035 = CARTESIAN_POINT ( 'NONE',  ( 3.756430356250000102, 15.45312499938548356, 30.00000000000000000 ) ) ;
#73036 = CARTESIAN_POINT ( 'NONE',  ( 1.138803498474273873E-14, 15.48124999877096641, 34.00000000000000000 ) ) ;
#73037 = CARTESIAN_POINT ( 'NONE',  ( 9.571875000614518569, 3.027376345333611329, 5.243569643749999010 ) ) ;
#73038 = CARTESIAN_POINT ( 'NONE',  ( 10.53750000122903252, 6.123233995736764310E-16, -4.999999999999998224 ) ) ;
#73039 = CARTESIAN_POINT ( 'NONE',  ( 3.496875000614518836, -3.027376345333610441, -5.243569643749999898 ) ) ;
#73040 = CARTESIAN_POINT ( 'NONE',  ( 5.334375000614517859, 6.421520780324663323E-16, -5.243569643749999010 ) ) ;
#73041 = CARTESIAN_POINT ( 'NONE',  ( -1.071796769724496556, 16.60490381179669939, -26.00000000000000355 ) ) ;
#73042 = CARTESIAN_POINT ( 'NONE',  ( 27.53437500061451360, 4.541064518000418104, 2.621784821874999949 ) ) ;
#73043 = EDGE_CURVE ( 'NONE', #53411, #32794, #18370, .T. ) ;
#73044 = CARTESIAN_POINT ( 'NONE',  ( -2.121784821874999949, 9.828125000614594597, 26.32496088578401938 ) ) ;
#73045 = CARTESIAN_POINT ( 'NONE',  ( 20.43749999999999645, 5.773502691896255534, 3.535250795749688894E-16 ) ) ;
#73046 = ORIENTED_EDGE ( 'NONE', *, *, #60961, .F. ) ;
#73047 = CARTESIAN_POINT ( 'NONE',  ( 26.92499999999999716, -4.330127018922194537, 2.499999999999995559 ) ) ;
#73048 = CARTESIAN_POINT ( 'NONE',  ( 28.05937500061451573, 0.000000000000000000, 5.243569643749999010 ) ) ;
#73049 = ORIENTED_EDGE ( 'NONE', *, *, #24709, .T. ) ;
#73050 = CARTESIAN_POINT ( 'NONE',  ( 14.84062500061451750, 6.054752690667223547, 3.707466751127219781E-16 ) ) ;
#73051 = CARTESIAN_POINT ( 'NONE',  ( 9.253125000614517148, -4.541064518000417216, -2.621784821875001281 ) ) ;
#73052 = CARTESIAN_POINT ( 'NONE',  ( 20.48437500061451644, -2.746126346562642428, -4.756430356249999214 ) ) ;
#73053 = CARTESIAN_POINT ( 'NONE',  ( 5.859375000614519102, 4.541064518000418104, -2.621784821874998173 ) ) ;
#73054 = CARTESIAN_POINT ( 'NONE',  ( 18.52500000122903145, -5.773502691896255534, -1.060575238724906372E-15 ) ) ;
#73055 = CARTESIAN_POINT ( 'NONE',  ( 24.29999999999999716, -4.330127018922190985, -2.500000000000001332 ) ) ;
#73056 = CARTESIAN_POINT ( 'NONE',  ( 11.32500000000000107, 6.123233995736764310E-16, -4.999999999999998224 ) ) ;
#73057 = CARTESIAN_POINT ( 'NONE',  ( 6.796875000614516438, 6.054752690667223547, 3.707466751127219781E-16 ) ) ;
#73058 = CARTESIAN_POINT ( 'NONE',  ( 11.18437500061451928, 6.421520780324663323E-16, -5.243569643749999010 ) ) ;
#73059 = CARTESIAN_POINT ( 'NONE',  ( 21.38437500061451502, -4.541064518000419881, 2.621784821874995952 ) ) ;
#73060 = CARTESIAN_POINT ( 'NONE',  ( 1.626862140677534273E-15, 16.51249999999999929, 34.00000000000000000 ) ) ;
#73061 = ORIENTED_EDGE ( 'NONE', *, *, #67636, .F. ) ;
#73062 = CARTESIAN_POINT ( 'NONE',  ( 4.546875000614517326, 6.054752690667223547, 3.707466751127219781E-16 ) ) ;
#73063 = CARTESIAN_POINT ( 'NONE',  ( 11.47499999999999964, 4.330127018922191873, 2.499999999999999556 ) ) ;
#73064 = CARTESIAN_POINT ( 'NONE',  ( 7.621875000614519280, 3.027376345333613106, -5.243569643749998122 ) ) ;
#73065 = CARTESIAN_POINT ( 'NONE',  ( 20.73750000000000071, -2.886751345948125991, -5.000000000000000000 ) ) ;
#73066 = CARTESIAN_POINT ( 'NONE',  ( 16.45312500061451289, -4.541064518000417216, -2.621784821875001281 ) ) ;
#73067 = CARTESIAN_POINT ( 'NONE',  ( -4.000000000000000000, 17.67500000000000071, 30.00000000000000000 ) ) ;
#73068 = CARTESIAN_POINT ( 'NONE',  ( 4.243387908797823016, 2.644552713687023271, 4.380842878058396117 ) ) ;
#73069 = CARTESIAN_POINT ( 'NONE',  ( 21.60937500061451644, 4.119189519843966529, -2.378215178124998275 ) ) ;
#73070 = CARTESIAN_POINT ( 'NONE',  ( 10.75312500061451715, 4.541064518000418104, -2.621784821874998173 ) ) ;
#73071 = CARTESIAN_POINT ( 'NONE',  ( 26.10937500061451644, 4.541064518000418104, -2.621784821874998173 ) ) ;
#73072 = DIRECTION ( 'NONE',  ( -0.000000000000000000, -1.000000000000000000, -0.000000000000000000 ) ) ;
#73073 = CARTESIAN_POINT ( 'NONE',  ( 28.32187500061451502, 3.027376345333613106, -5.243569643749998122 ) ) ;
#73074 = CARTESIAN_POINT ( 'NONE',  ( 9.037499999999999645, -2.886751345948125991, -5.000000000000000000 ) ) ;
#73075 = CARTESIAN_POINT ( 'NONE',  ( 3.999999999999999112, 14.93750000122903288, 30.00000000000000000 ) ) ;
#73076 = CARTESIAN_POINT ( 'NONE',  ( 8.737500001229033586, 6.123233995736764310E-16, -4.999999999999998224 ) ) ;
#73077 = CARTESIAN_POINT ( 'NONE',  ( 18.98437500061451644, 4.541064518000418104, 2.621784821874999949 ) ) ;
#73078 = CARTESIAN_POINT ( 'NONE',  ( 14.78437500061451715, 6.421520780324663323E-16, -5.243569643749999010 ) ) ;
#73079 = CARTESIAN_POINT ( 'NONE',  ( 9.187500001229034652, 6.123233995736764310E-16, -4.999999999999998224 ) ) ;
#73080 = ORIENTED_EDGE ( 'NONE', *, *, #27328, .T. ) ;
#73081 = CARTESIAN_POINT ( 'NONE',  ( 14.65312500061451573, -4.541064518000417216, -2.621784821875001281 ) ) ;
#73082 = CARTESIAN_POINT ( 'NONE',  ( 25.20000000122903216, -2.886751345948129988, 4.999999999999997335 ) ) ;
#73083 = CARTESIAN_POINT ( 'NONE',  ( 14.67187500061451821, -6.054752690667223547, -1.112240025338166033E-15 ) ) ;
#73084 = CARTESIAN_POINT ( 'NONE',  ( 3.328125000614516438, -4.541064518000419881, 2.621784821874995952 ) ) ;
#73085 = CARTESIAN_POINT ( 'NONE',  ( 16.79062500061451857, -3.027376345333614438, 5.243569643749998122 ) ) ;
#73086 = CARTESIAN_POINT ( 'NONE',  ( 18.52499999999999858, 6.123233995736764310E-16, -4.999999999999998224 ) ) ;
#73087 = CARTESIAN_POINT ( 'NONE',  ( 25.84687500061451360, -3.027376345333614438, 5.243569643749998122 ) ) ;
#73088 = CARTESIAN_POINT ( 'NONE',  ( 9.001249775931846008E-16, 11.36562500061451786, 34.90005215228797653 ) ) ;
#73089 = CARTESIAN_POINT ( 'NONE',  ( 14.63437500061451679, -4.541064518000419881, 2.621784821874995952 ) ) ;
#73090 = CARTESIAN_POINT ( 'NONE',  ( 14.58750000122903323, 6.123233995736764310E-16, -4.999999999999998224 ) ) ;
#73091 = CARTESIAN_POINT ( 'NONE',  ( 7.884375000614517681, -4.119189519843968306, 2.378215178124996054 ) ) ;
#73092 = CARTESIAN_POINT ( 'NONE',  ( -4.243569643749998122, 18.99687500061451928, -27.54997392385601174 ) ) ;
#73093 = CARTESIAN_POINT ( 'NONE',  ( 21.30937500061451573, 0.000000000000000000, 5.243569643749999010 ) ) ;
#73094 = CARTESIAN_POINT ( 'NONE',  ( 20.96250000122903145, 4.330127018922192761, -2.499999999999997780 ) ) ;
#73095 = CARTESIAN_POINT ( 'NONE',  ( 13.58437500061451786, 4.541064518000418104, 2.621784821874999949 ) ) ;
#73096 = CARTESIAN_POINT ( 'NONE',  ( 2.121784821874999061, 11.60937500061451821, 26.32496088578401583 ) ) ;
#73097 = CARTESIAN_POINT ( 'NONE',  ( 21.75000000122903288, -2.886751345948125991, -5.000000000000000000 ) ) ;
#73098 = CARTESIAN_POINT ( 'NONE',  ( 18.29062500061451502, -3.027376345333610441, -5.243569643749999898 ) ) ;
#73099 = EDGE_LOOP ( 'NONE', ( #11929, #59178, #27988, #24516 ) ) ;
#73100 = ORIENTED_EDGE ( 'NONE', *, *, #48794, .T. ) ;
#73101 = CARTESIAN_POINT ( 'NONE',  ( 21.48750000000000071, -2.886751345948129988, 4.999999999999997335 ) ) ;
#73102 = CARTESIAN_POINT ( 'NONE',  ( 30.00000000000000000, 0.000000000000000000, 0.000000000000000000 ) ) ;
#73103 = CARTESIAN_POINT ( 'NONE',  ( 25.04062500061451502, -3.027376345333610441, -5.243569643749999898 ) ) ;
#73104 = CARTESIAN_POINT ( 'NONE',  ( 3.943546631589880391, 3.074146327801218437, 30.68299680867395907 ) ) ;
#73105 = CARTESIAN_POINT ( 'NONE',  ( 18.52500000122903145, -5.773502691896255534, -1.060575238724906372E-15 ) ) ;
#73106 = CARTESIAN_POINT ( 'NONE',  ( 21.55312500061451431, 4.541064518000418104, -2.621784821874998173 ) ) ;
#73107 = EDGE_CURVE ( 'NONE', #37048, #48891, #47355, .T. ) ;
#73108 = CARTESIAN_POINT ( 'NONE',  ( 24.92812500061451431, -4.541064518000419881, 2.621784821874995952 ) ) ;
#73109 = CARTESIAN_POINT ( 'NONE',  ( 5.053125000614517859, 0.000000000000000000, 5.243569643749999010 ) ) ;
#73110 = EDGE_LOOP ( 'NONE', ( #47495, #330, #25184, #41516 ) ) ;
#73111 = CARTESIAN_POINT ( 'NONE',  ( 26.88750000122903216, 4.330127018922191873, 2.499999999999999556 ) ) ;
#73112 = CARTESIAN_POINT ( 'NONE',  ( -1.071796769724488563, 10.30490381179670045, -26.00000000000000000 ) ) ;
#73113 = CARTESIAN_POINT ( 'NONE',  ( 11.33437500061451608, 4.119189519843966529, 2.378215178124999607 ) ) ;
#73114 = CYLINDRICAL_SURFACE ( 'NONE', #50058, 4.999999999999998224 ) ;
#73115 = CARTESIAN_POINT ( 'NONE',  ( 3.999999999999998668, 10.92500000122903536, -32.30940107675850470 ) ) ;
#73116 = CARTESIAN_POINT ( 'NONE',  ( -2.121784821874999949, 19.33437500061451786, -33.67503911421598417 ) ) ;
#73117 = CARTESIAN_POINT ( 'NONE',  ( 7.387500000000001066, 5.773502691896255534, 3.535250795749688894E-16 ) ) ;
#73118 = CARTESIAN_POINT ( 'NONE',  ( 29.55000000122903003, 5.773502691896255534, 3.535250795749688401E-16 ) ) ;
#73119 = NEXT_ASSEMBLY_USAGE_OCCURRENCE ( 'NAUO1', ' ', ' ', #36353, #45867, $ ) ;
#73120 = NEXT_ASSEMBLY_USAGE_OCCURRENCE ( 'NAUO2', ' ', ' ', #36353, #3433, $ ) ;
#73121 = NEXT_ASSEMBLY_USAGE_OCCURRENCE ( 'NAUO3', ' ', ' ', #36353, #2500, $ ) ;
#73122 = NEXT_ASSEMBLY_USAGE_OCCURRENCE ( 'NAUO4', ' ', ' ', #36353, #58930, $ ) ;
#73123 = NEXT_ASSEMBLY_USAGE_OCCURRENCE ( 'NAUO5', ' ', ' ', #36353, #3433, $ ) ;
#73124=COLOUR_RGB('Dark Blue',0.08,0.2,0.34);
#73125=FILL_AREA_STYLE_COLOUR('',#73124);
#73126=FILL_AREA_STYLE('',(#73125));
#73127=SURFACE_STYLE_FILL_AREA(#73126);
#73128=SURFACE_SIDE_STYLE('',(#73127));
#73129=SURFACE_STYLE_USAGE(.BOTH.,#73128);
#73130=PRESENTATION_STYLE_ASSIGNMENT((#73129));
#73131=COLOUR_RGB('Light Blue',0.38,0.62,0.78);
#73132=FILL_AREA_STYLE_COLOUR('',#73131);
#73133=FILL_AREA_STYLE('',(#73132));
#73134=SURFACE_STYLE_FILL_AREA(#73133);
#73135=SURFACE_SIDE_STYLE('',(#73134));
#73136=SURFACE_STYLE_USAGE(.BOTH.,#73135);
#73137=PRESENTATION_STYLE_ASSIGNMENT((#73136));
#73138=COLOUR_RGB('Sky Blue',0.24,0.69,0.87);
#73139=FILL_AREA_STYLE_COLOUR('',#73138);
#73140=FILL_AREA_STYLE('',(#73139));
#73141=SURFACE_STYLE_FILL_AREA(#73140);
#73142=SURFACE_SIDE_STYLE('',(#73141));
#73143=SURFACE_STYLE_USAGE(.BOTH.,#73142);
#73144=PRESENTATION_STYLE_ASSIGNMENT((#73143));
#73145=COLOUR_RGB('Grey',0.48,0.52,0.57);
#73146=FILL_AREA_STYLE_COLOUR('',#73145);
#73147=FILL_AREA_STYLE('',(#73146));
#73148=SURFACE_STYLE_FILL_AREA(#73147);
#73149=SURFACE_SIDE_STYLE('',(#73148));
#73150=SURFACE_STYLE_USAGE(.BOTH.,#73149);
#73151=PRESENTATION_STYLE_ASSIGNMENT((#73150));
#73152=COLOUR_RGB('Black',0.12,0.14,0.17);
#73153=FILL_AREA_STYLE_COLOUR('',#73152);
#73154=FILL_AREA_STYLE('',(#73153));
#73155=SURFACE_STYLE_FILL_AREA(#73154);
#73156=SURFACE_SIDE_STYLE('',(#73155));
#73157=SURFACE_STYLE_USAGE(.BOTH.,#73156);
#73158=PRESENTATION_STYLE_ASSIGNMENT((#73157));
#73159=COLOUR_RGB('Off White',0.89,0.88,0.83);
#73160=FILL_AREA_STYLE_COLOUR('',#73159);
#73161=FILL_AREA_STYLE('',(#73160));
#73162=SURFACE_STYLE_FILL_AREA(#73161);
#73163=SURFACE_SIDE_STYLE('',(#73162));
#73164=SURFACE_STYLE_USAGE(.BOTH.,#73163);
#73165=PRESENTATION_STYLE_ASSIGNMENT((#73164));
ENDSEC;
END-ISO-10303-21;
